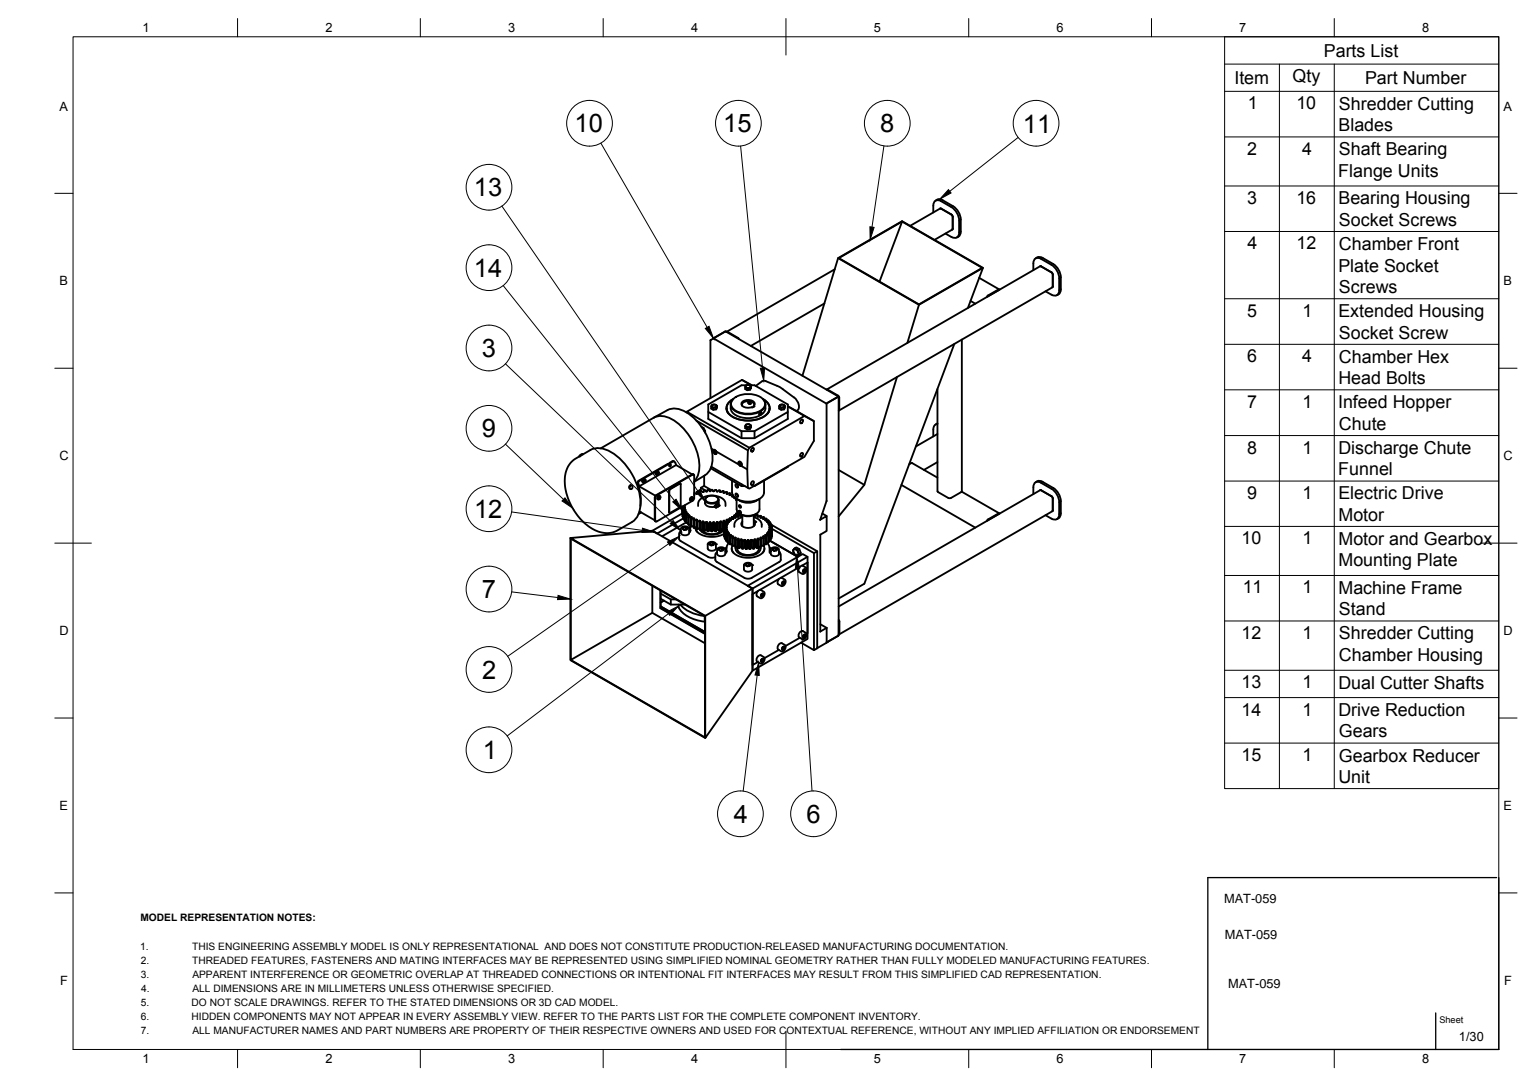
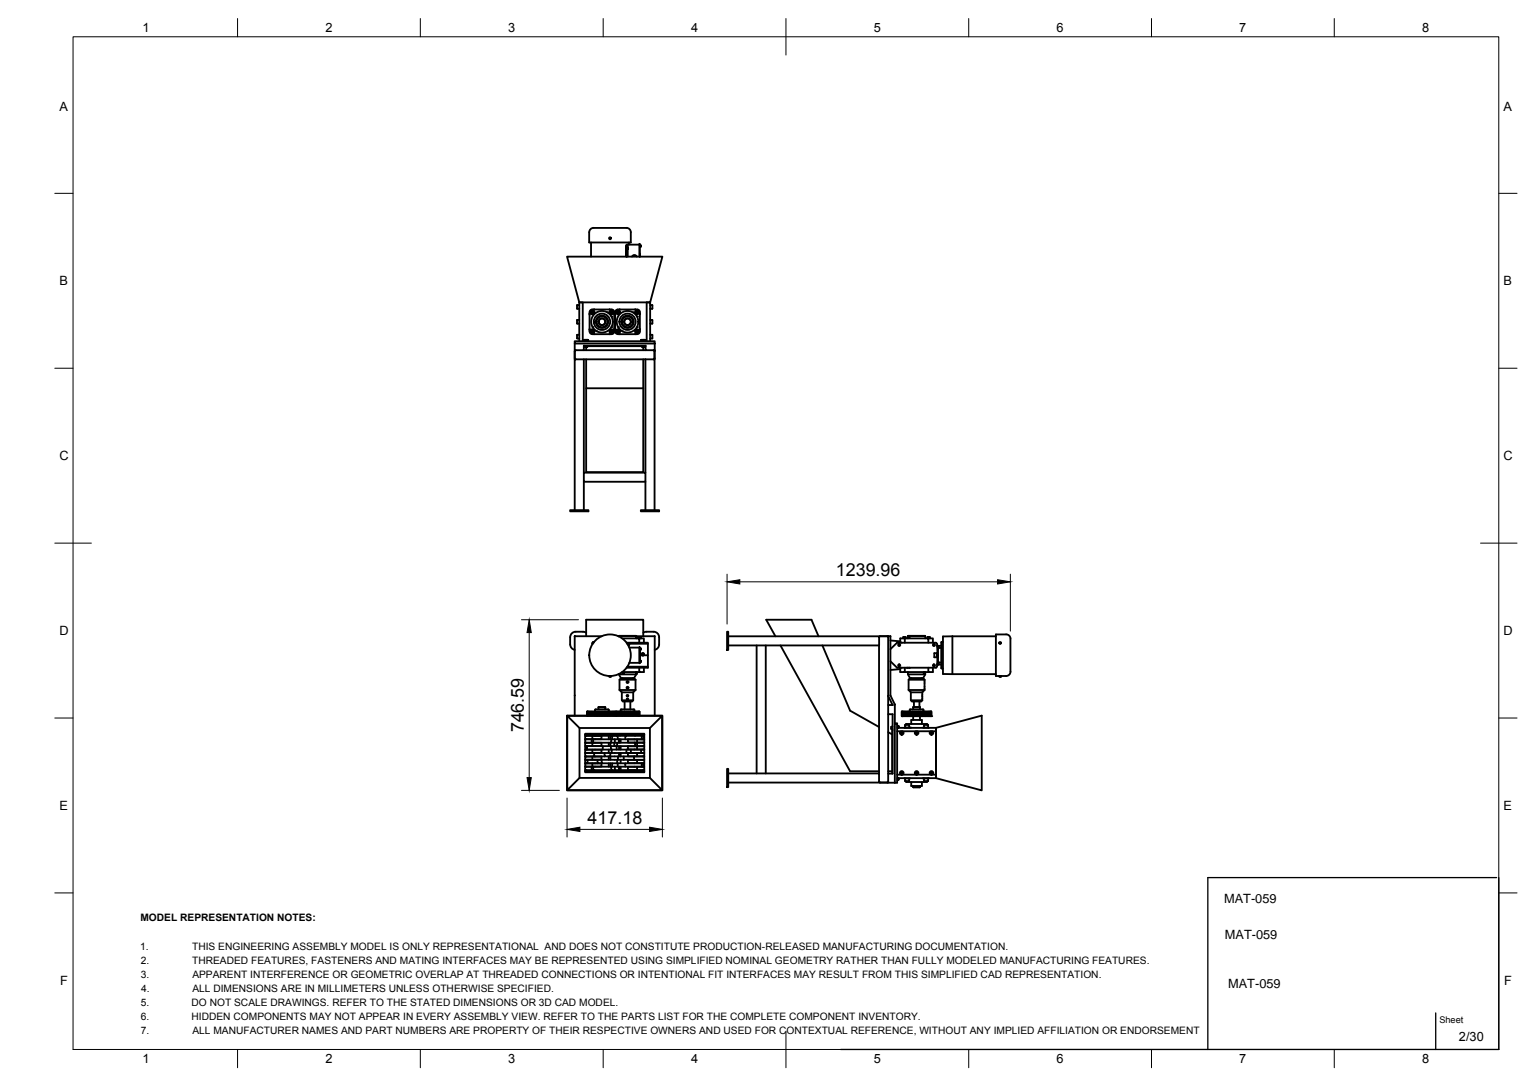
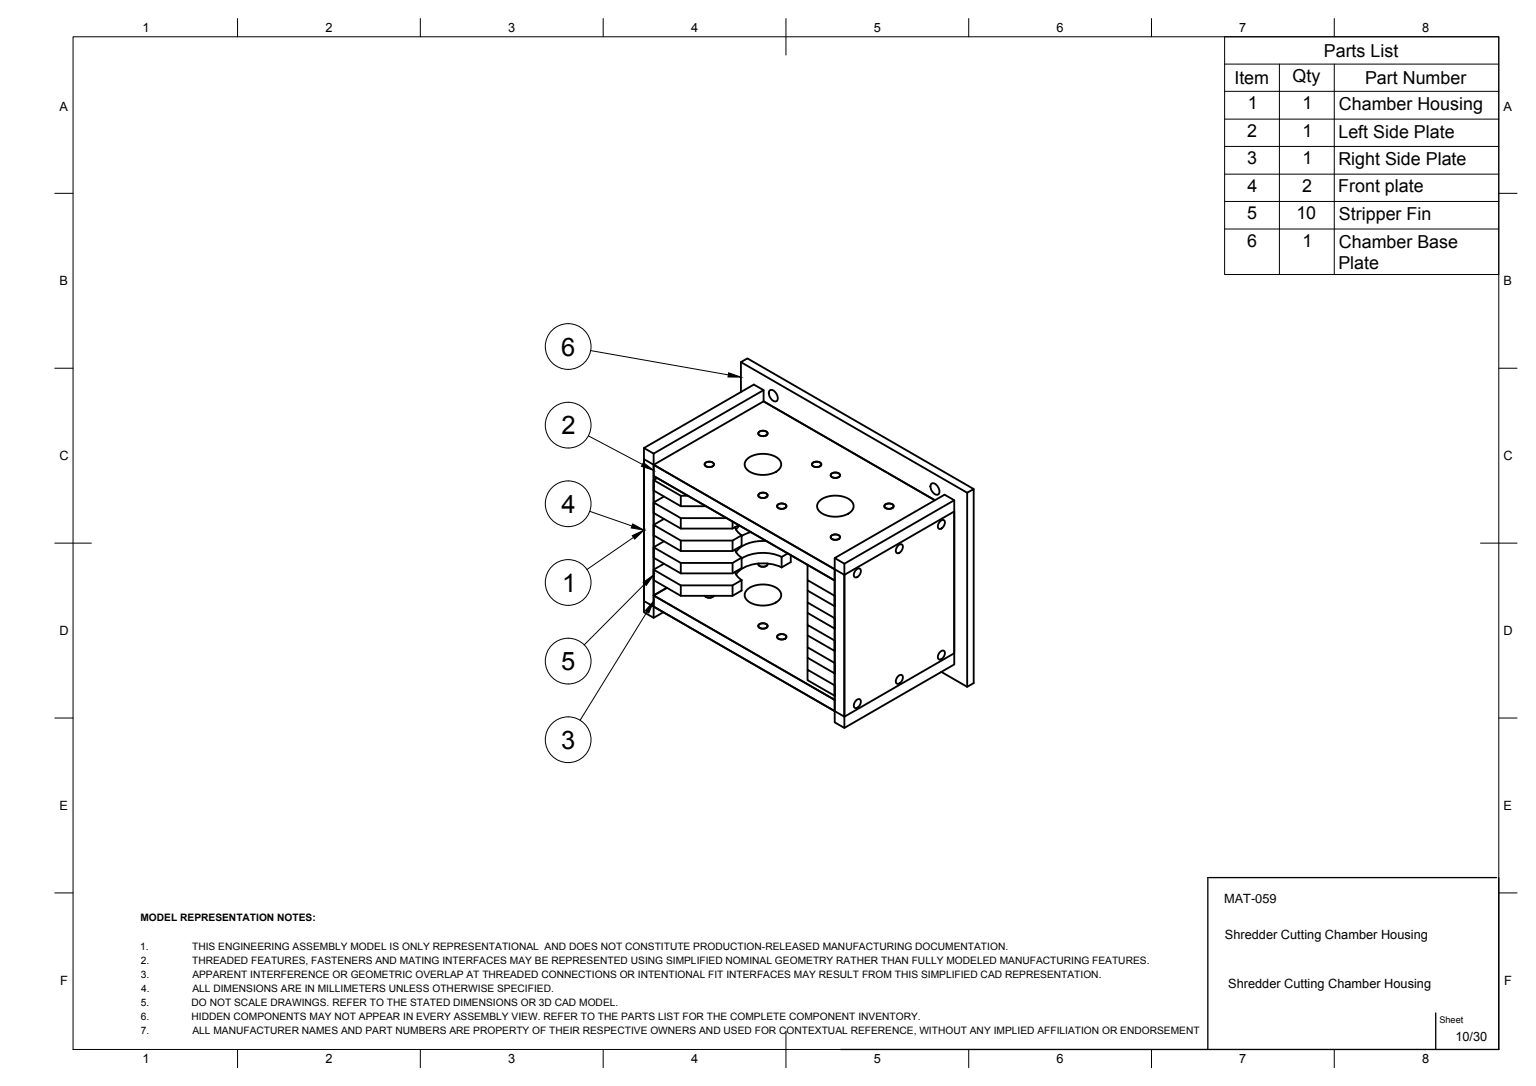
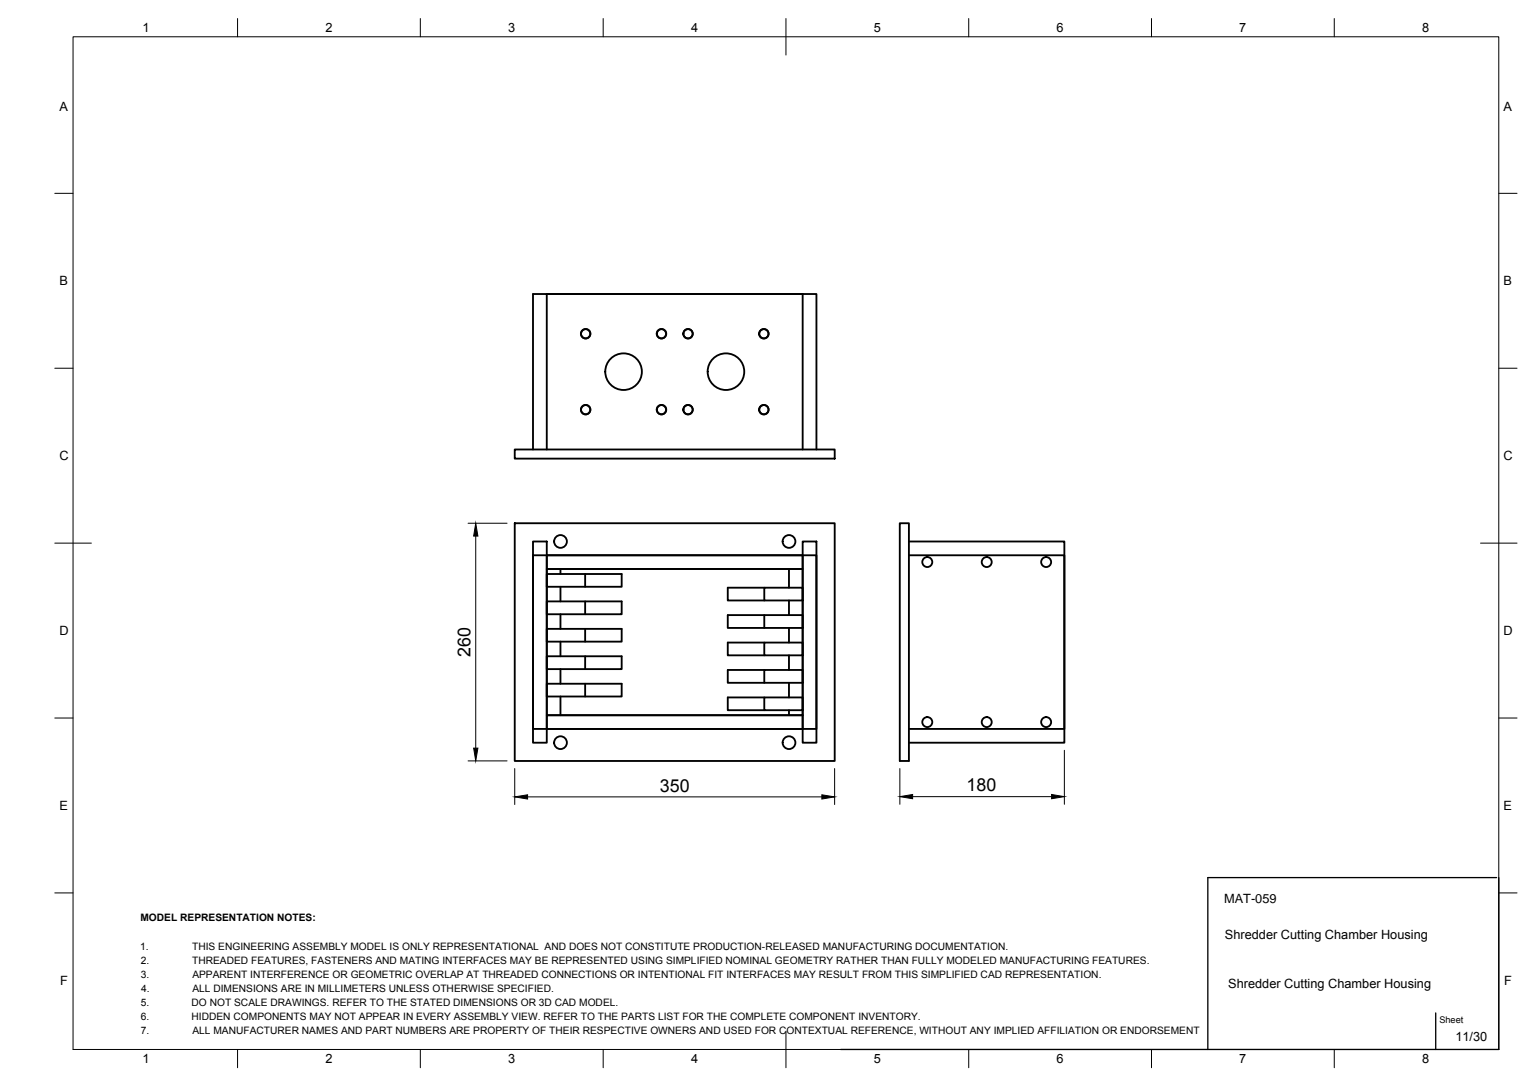
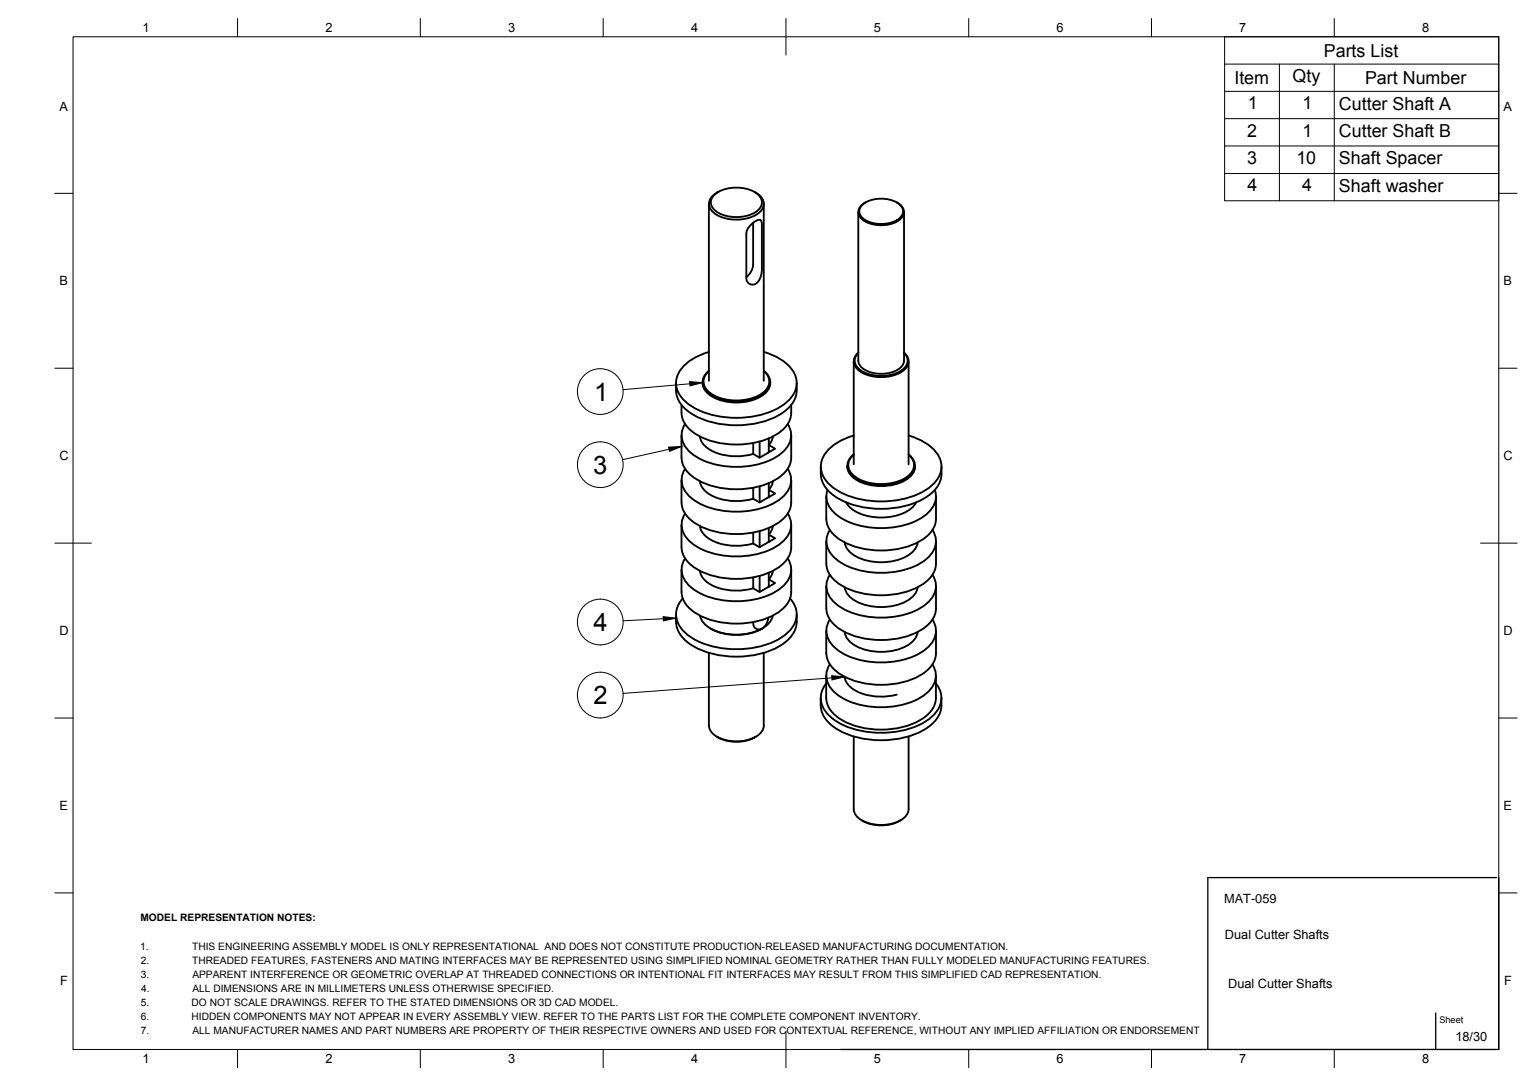
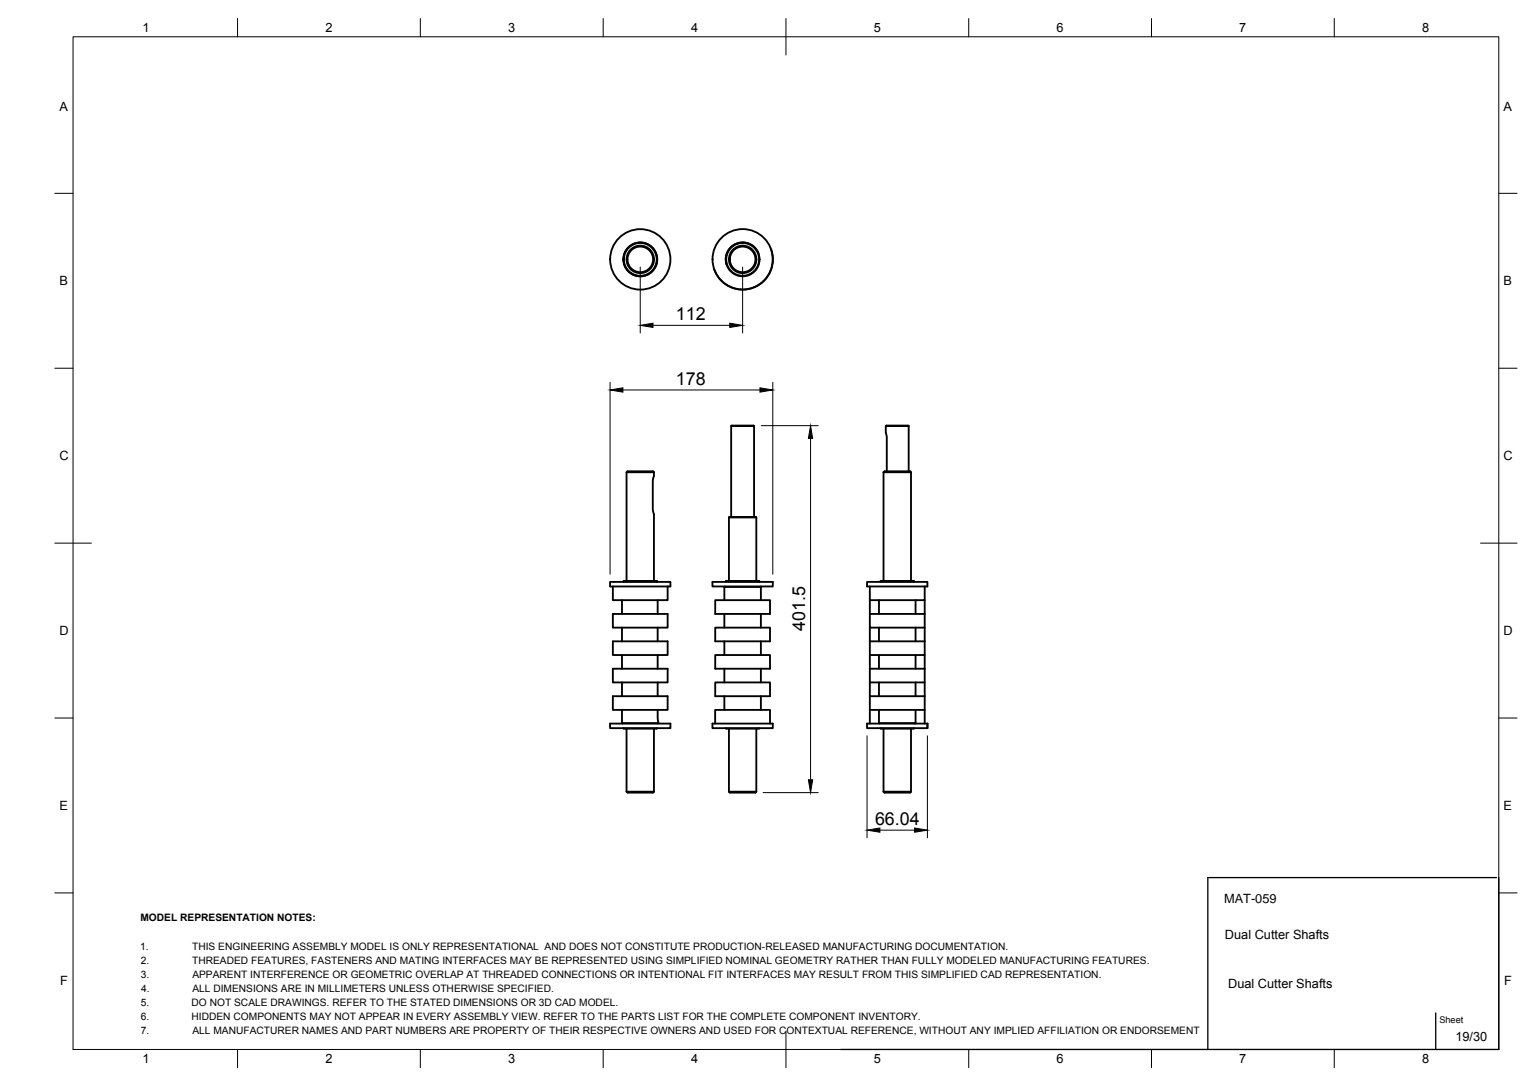
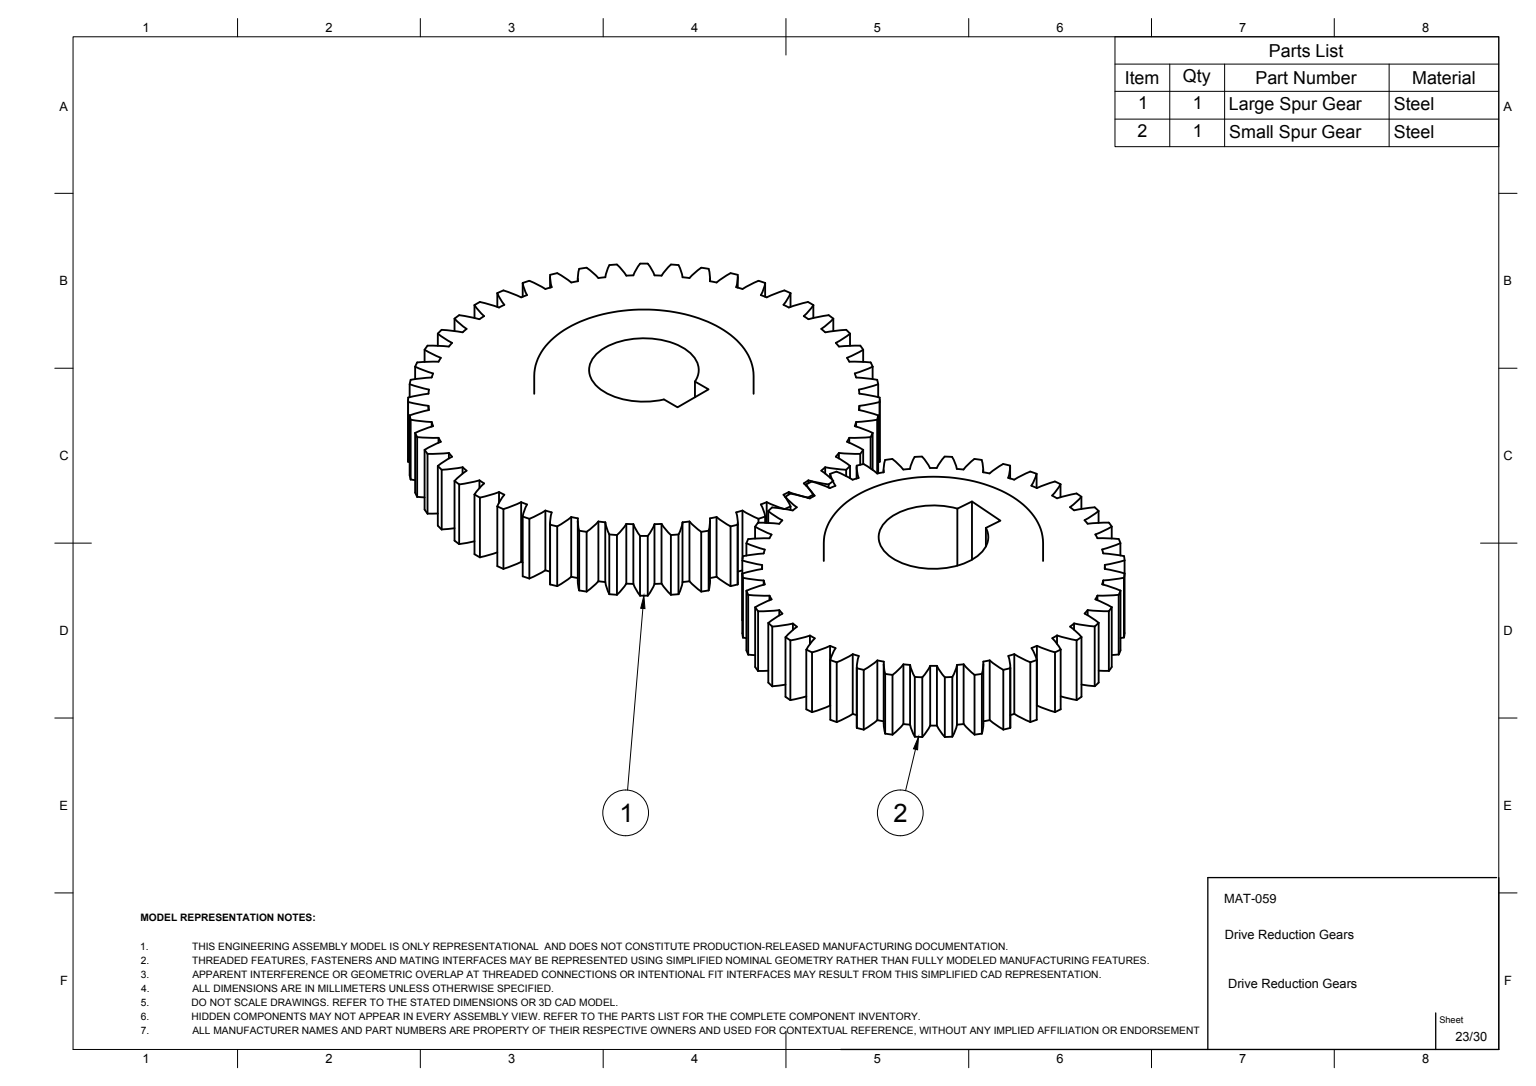
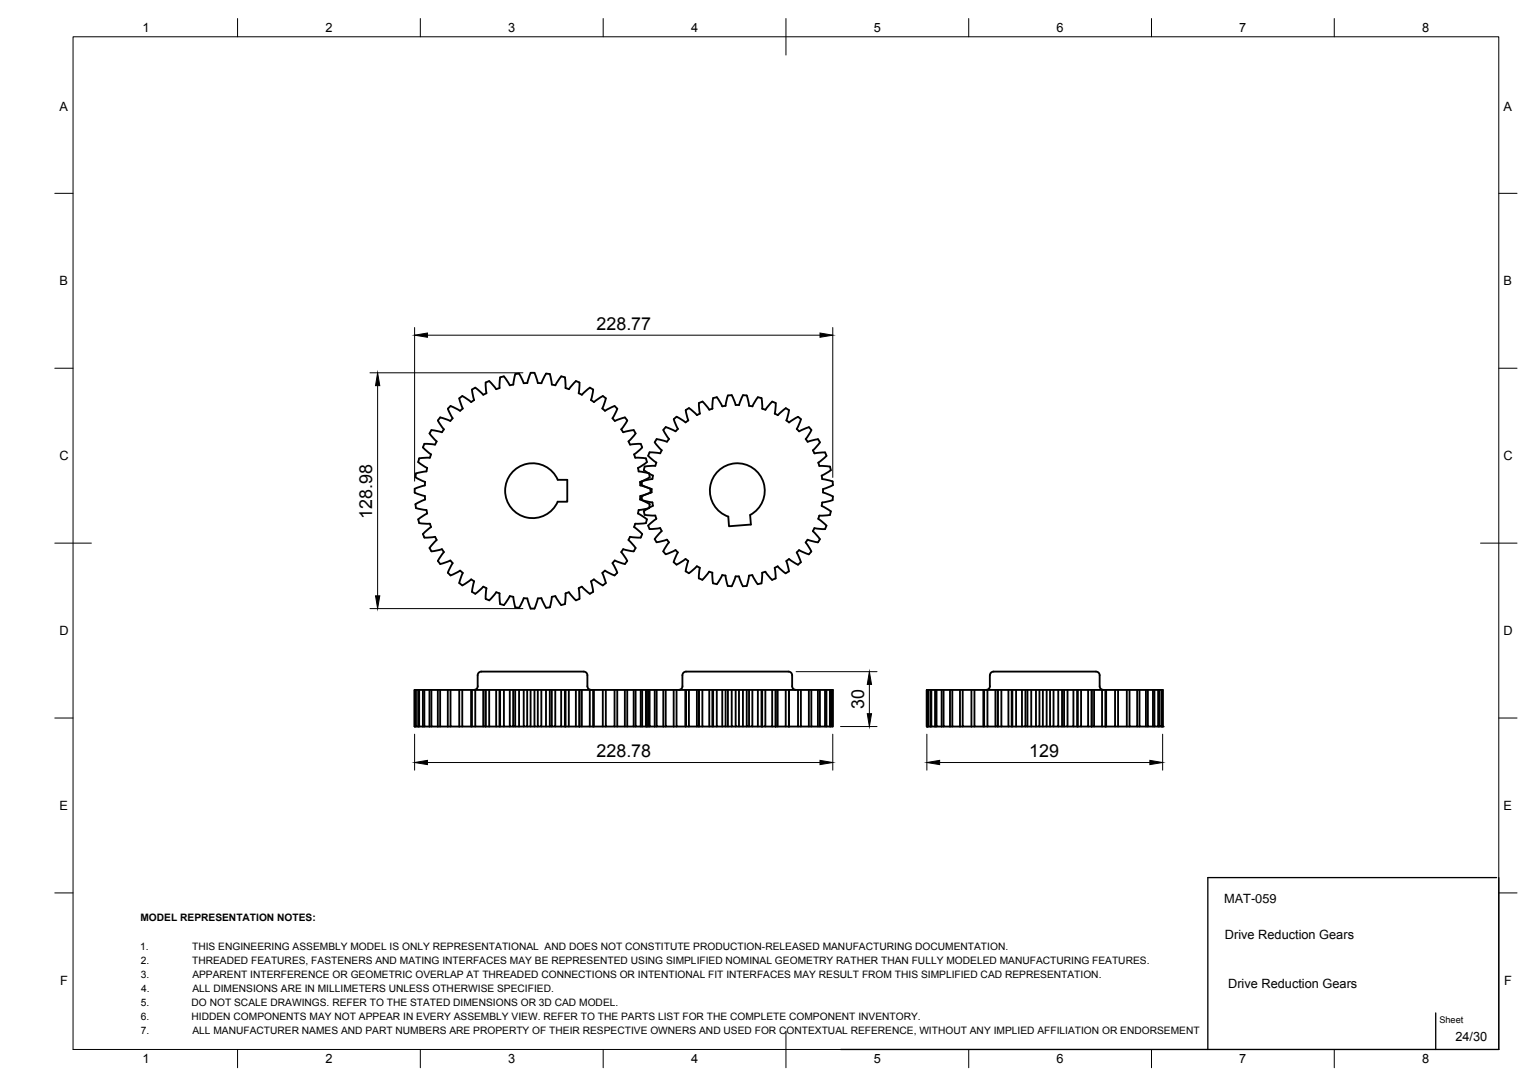
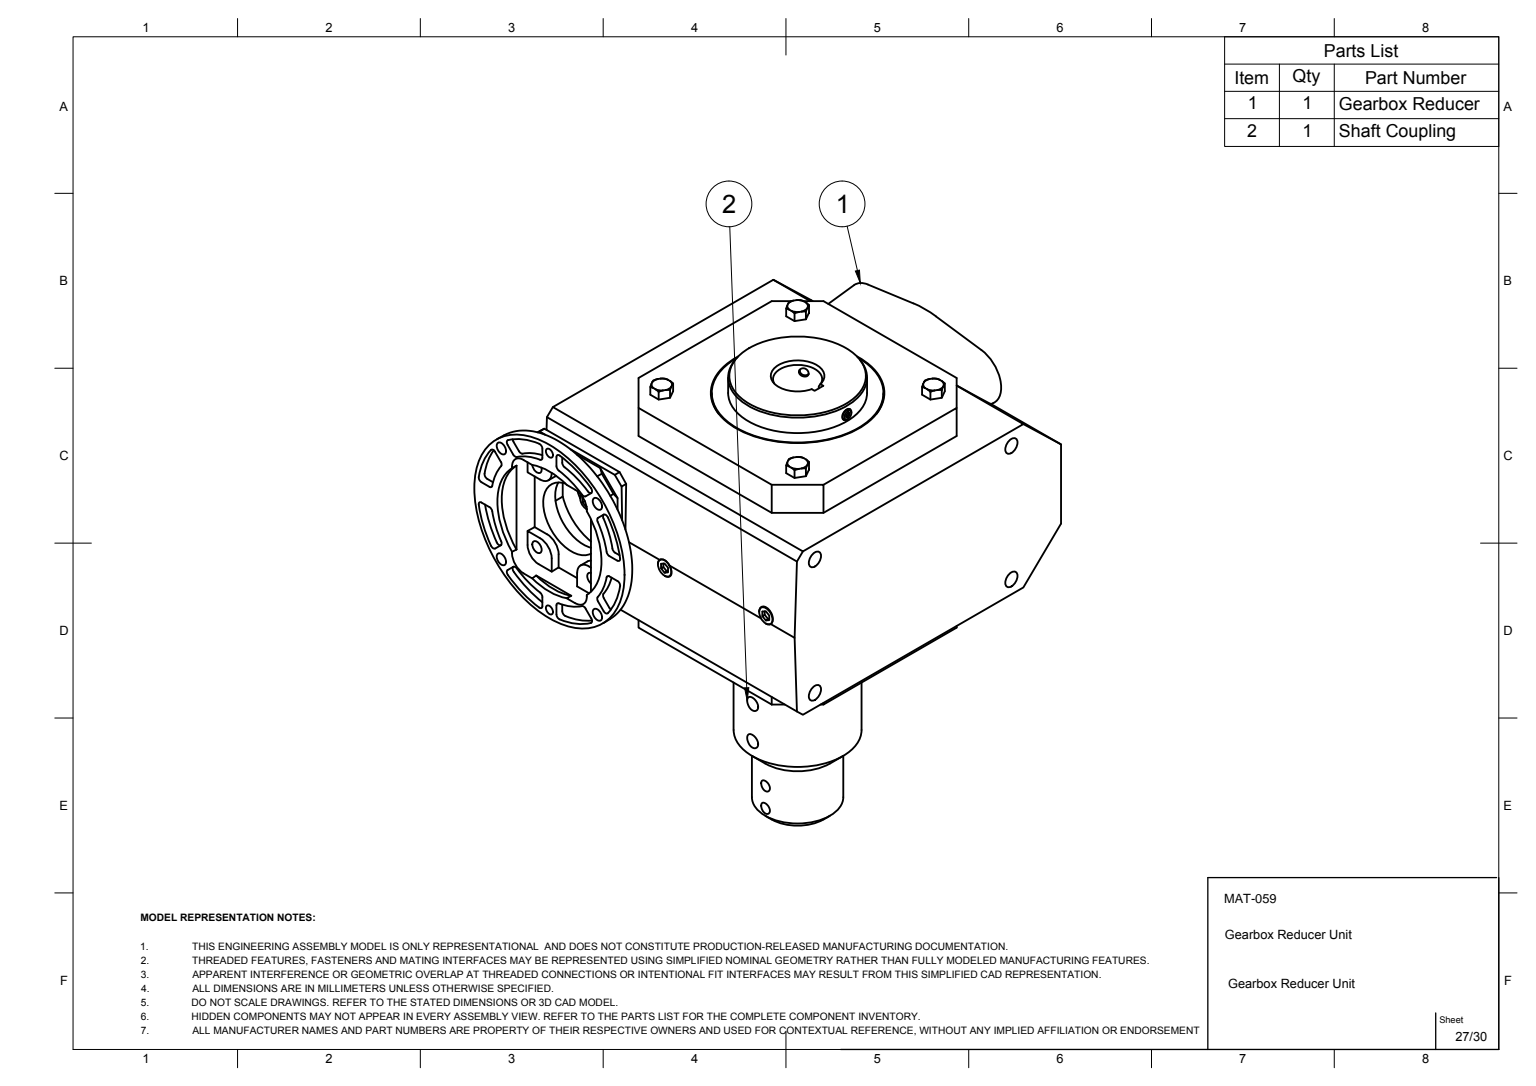
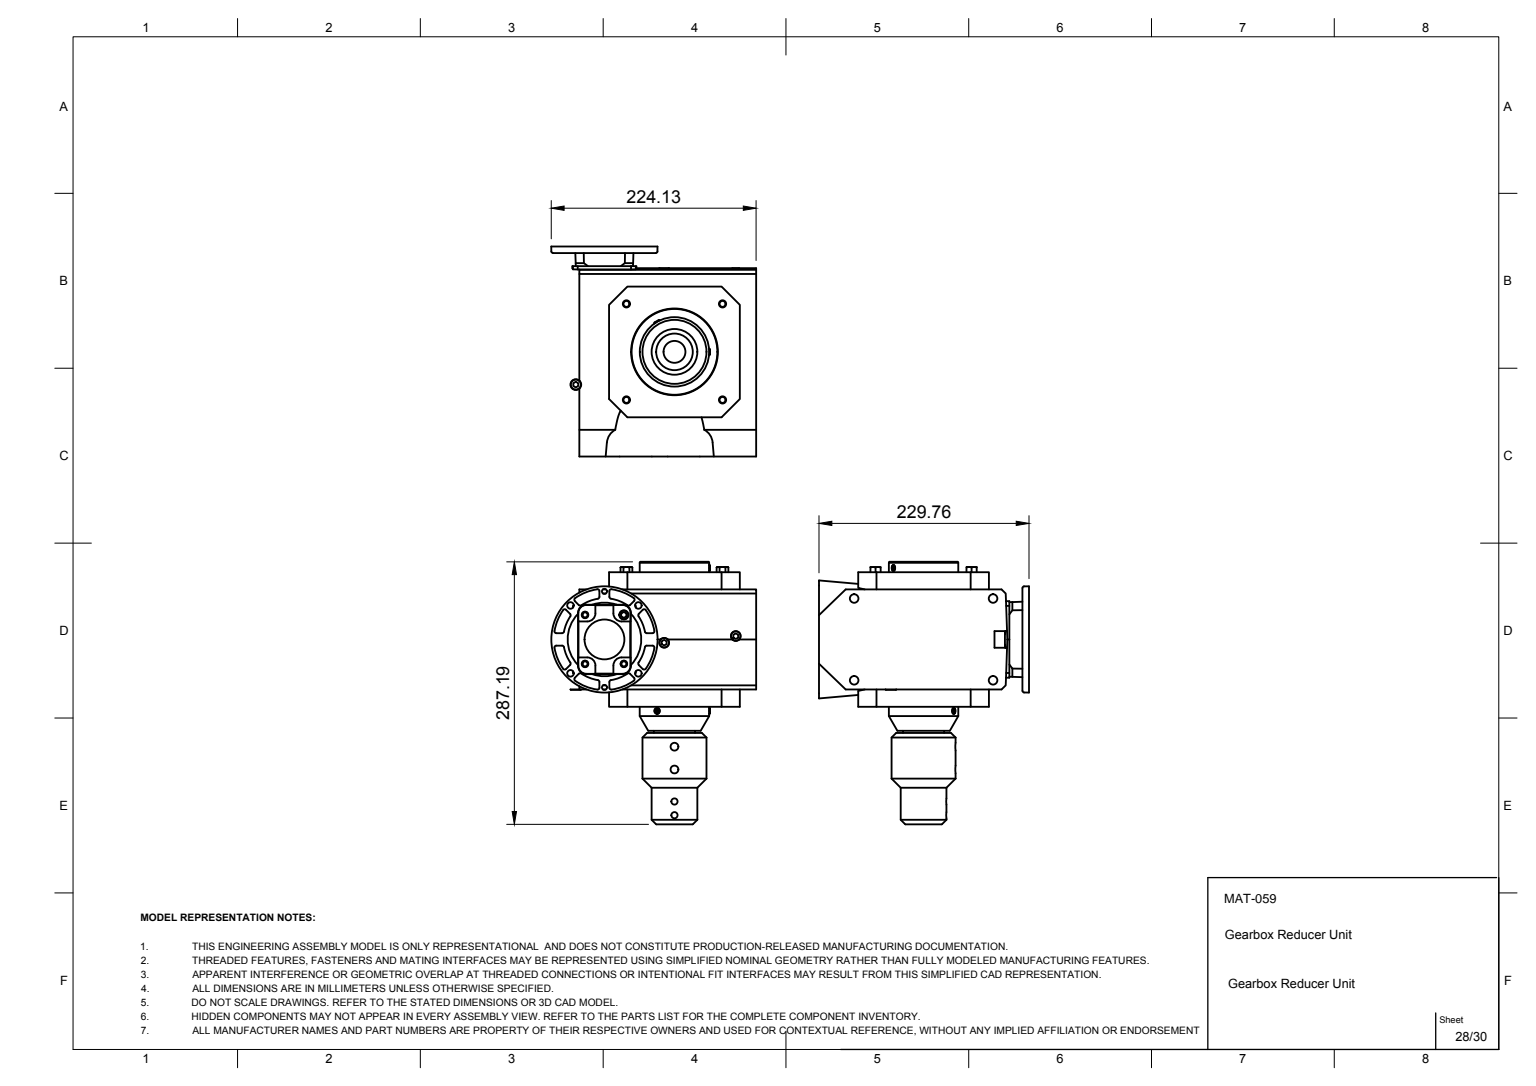
ISO-10303-21;
HEADER;
/* Generated by software containing ST-Developer
 * from STEP Tools, Inc. (www.steptools.com) 
 */

FILE_DESCRIPTION(
/* description */ ('', 'CAx-IF Rec.Pracs.---Representation and Presentation of Product Manufa
cturing Information (PMI)---4.0---2014-10-13'),
/* implementation_level */ '2;1');

FILE_NAME(
/* name */ 'MAT-059',
/* time_stamp */ '2026-10-28T23:00:48+01:00',
/* author */ (''),
/* organization */ (''),
/* preprocessor_version */ 'ST-DEVELOPER v20.2',
/* originating_system */ 'Autodesk Translation Framework v15.17.0.0',
/* authorisation */ '');

FILE_SCHEMA (('AP242_MANAGED_MODEL_BASED_3D_ENGINEERING_MIM_LF { 1 0 10303 442 2 1 4 }'));
ENDSEC;

DATA;
#10=MECHANICAL_DESIGN_GEOMETRIC_PRESENTATION_REPRESENTATION('',(#961,#962,
#963,#964,#965,#966,#967,#968,#969,#970,#971,#972,#973,#974,#975,#976,#977,
#978,#979,#980,#981,#982,#983,#984,#985,#986,#987,#988,#989,#990,#991,#992,
#993,#994,#995,#996,#997,#998,#999),#61811);
#11=ORIENTED_CLOSED_SHELL('',*,#33828,.F.);
#12=ORIENTED_CLOSED_SHELL('',*,#33829,.F.);
#13=ORIENTED_CLOSED_SHELL('',*,#33830,.F.);
#14=ORIENTED_CLOSED_SHELL('',*,#33831,.F.);
#15=ORIENTED_CLOSED_SHELL('',*,#33832,.F.);
#16=ORIENTED_CLOSED_SHELL('',*,#33833,.F.);
#17=ORIENTED_CLOSED_SHELL('',*,#33834,.F.);
#18=ORIENTED_CLOSED_SHELL('',*,#33835,.F.);
#19=ORIENTED_CLOSED_SHELL('',*,#33836,.F.);
#20=ORIENTED_CLOSED_SHELL('',*,#33837,.F.);
#21=BREP_WITH_VOIDS('Body1',#33838,(#11,#12,#13,#14,#15,#16,#17,#18,#19,
#20));
#22=ITEM_DEFINED_TRANSFORMATION($,$,#35703,#35945);
#23=ITEM_DEFINED_TRANSFORMATION($,$,#35762,#35946);
#24=ITEM_DEFINED_TRANSFORMATION($,$,#35823,#35947);
#25=ITEM_DEFINED_TRANSFORMATION($,$,#35884,#35948);
#26=ITEM_DEFINED_TRANSFORMATION($,$,#35884,#35949);
#27=ITEM_DEFINED_TRANSFORMATION($,$,#35909,#35950);
#28=ITEM_DEFINED_TRANSFORMATION($,$,#35909,#35951);
#29=ITEM_DEFINED_TRANSFORMATION($,$,#35909,#35952);
#30=ITEM_DEFINED_TRANSFORMATION($,$,#35909,#35953);
#31=ITEM_DEFINED_TRANSFORMATION($,$,#35909,#35954);
#32=ITEM_DEFINED_TRANSFORMATION($,$,#35909,#35955);
#33=ITEM_DEFINED_TRANSFORMATION($,$,#35909,#35956);
#34=ITEM_DEFINED_TRANSFORMATION($,$,#35909,#35957);
#35=ITEM_DEFINED_TRANSFORMATION($,$,#35909,#35958);
#36=ITEM_DEFINED_TRANSFORMATION($,$,#35909,#35959);
#37=ITEM_DEFINED_TRANSFORMATION($,$,#35922,#35960);
#38=ITEM_DEFINED_TRANSFORMATION($,$,#35962,#36131);
#39=ITEM_DEFINED_TRANSFORMATION($,$,#36032,#36132);
#40=ITEM_DEFINED_TRANSFORMATION($,$,#36110,#36133);
#41=ITEM_DEFINED_TRANSFORMATION($,$,#36110,#36134);
#42=ITEM_DEFINED_TRANSFORMATION($,$,#36110,#36135);
#43=ITEM_DEFINED_TRANSFORMATION($,$,#36110,#36136);
#44=ITEM_DEFINED_TRANSFORMATION($,$,#36110,#36137);
#45=ITEM_DEFINED_TRANSFORMATION($,$,#36110,#36138);
#46=ITEM_DEFINED_TRANSFORMATION($,$,#36110,#36139);
#47=ITEM_DEFINED_TRANSFORMATION($,$,#36110,#36140);
#48=ITEM_DEFINED_TRANSFORMATION($,$,#36110,#36141);
#49=ITEM_DEFINED_TRANSFORMATION($,$,#36110,#36142);
#50=ITEM_DEFINED_TRANSFORMATION($,$,#36122,#36143);
#51=ITEM_DEFINED_TRANSFORMATION($,$,#36122,#36144);
#52=ITEM_DEFINED_TRANSFORMATION($,$,#36122,#36145);
#53=ITEM_DEFINED_TRANSFORMATION($,$,#36122,#36146);
#54=ITEM_DEFINED_TRANSFORMATION($,$,#36148,#37244);
#55=ITEM_DEFINED_TRANSFORMATION($,$,#36744,#37245);
#56=ITEM_DEFINED_TRANSFORMATION($,$,#37247,#38116);
#57=ITEM_DEFINED_TRANSFORMATION($,$,#38087,#38117);
#58=ITEM_DEFINED_TRANSFORMATION($,$,#34117,#38118);
#59=ITEM_DEFINED_TRANSFORMATION($,$,#34117,#38119);
#60=ITEM_DEFINED_TRANSFORMATION($,$,#34117,#38120);
#61=ITEM_DEFINED_TRANSFORMATION($,$,#34117,#38121);
#62=ITEM_DEFINED_TRANSFORMATION($,$,#34117,#38122);
#63=ITEM_DEFINED_TRANSFORMATION($,$,#34117,#38123);
#64=ITEM_DEFINED_TRANSFORMATION($,$,#34117,#38124);
#65=ITEM_DEFINED_TRANSFORMATION($,$,#34117,#38125);
#66=ITEM_DEFINED_TRANSFORMATION($,$,#34117,#38126);
#67=ITEM_DEFINED_TRANSFORMATION($,$,#34117,#38127);
#68=ITEM_DEFINED_TRANSFORMATION($,$,#34153,#38128);
#69=ITEM_DEFINED_TRANSFORMATION($,$,#34153,#38129);
#70=ITEM_DEFINED_TRANSFORMATION($,$,#34153,#38130);
#71=ITEM_DEFINED_TRANSFORMATION($,$,#34153,#38131);
#72=ITEM_DEFINED_TRANSFORMATION($,$,#34392,#38132);
#73=ITEM_DEFINED_TRANSFORMATION($,$,#34392,#38133);
#74=ITEM_DEFINED_TRANSFORMATION($,$,#34392,#38134);
#75=ITEM_DEFINED_TRANSFORMATION($,$,#34392,#38135);
#76=ITEM_DEFINED_TRANSFORMATION($,$,#34392,#38136);
#77=ITEM_DEFINED_TRANSFORMATION($,$,#34392,#38137);
#78=ITEM_DEFINED_TRANSFORMATION($,$,#34392,#38138);
#79=ITEM_DEFINED_TRANSFORMATION($,$,#34392,#38139);
#80=ITEM_DEFINED_TRANSFORMATION($,$,#34392,#38140);
#81=ITEM_DEFINED_TRANSFORMATION($,$,#34392,#38141);
#82=ITEM_DEFINED_TRANSFORMATION($,$,#34392,#38142);
#83=ITEM_DEFINED_TRANSFORMATION($,$,#34392,#38143);
#84=ITEM_DEFINED_TRANSFORMATION($,$,#34392,#38144);
#85=ITEM_DEFINED_TRANSFORMATION($,$,#34392,#38145);
#86=ITEM_DEFINED_TRANSFORMATION($,$,#34392,#38146);
#87=ITEM_DEFINED_TRANSFORMATION($,$,#34392,#38147);
#88=ITEM_DEFINED_TRANSFORMATION($,$,#34420,#38148);
#89=ITEM_DEFINED_TRANSFORMATION($,$,#34420,#38149);
#90=ITEM_DEFINED_TRANSFORMATION($,$,#34420,#38150);
#91=ITEM_DEFINED_TRANSFORMATION($,$,#34420,#38151);
#92=ITEM_DEFINED_TRANSFORMATION($,$,#34420,#38152);
#93=ITEM_DEFINED_TRANSFORMATION($,$,#34420,#38153);
#94=ITEM_DEFINED_TRANSFORMATION($,$,#34420,#38154);
#95=ITEM_DEFINED_TRANSFORMATION($,$,#34420,#38155);
#96=ITEM_DEFINED_TRANSFORMATION($,$,#34420,#38156);
#97=ITEM_DEFINED_TRANSFORMATION($,$,#34420,#38157);
#98=ITEM_DEFINED_TRANSFORMATION($,$,#34420,#38158);
#99=ITEM_DEFINED_TRANSFORMATION($,$,#34420,#38159);
#100=ITEM_DEFINED_TRANSFORMATION($,$,#34448,#38160);
#101=ITEM_DEFINED_TRANSFORMATION($,$,#34476,#38161);
#102=ITEM_DEFINED_TRANSFORMATION($,$,#34476,#38162);
#103=ITEM_DEFINED_TRANSFORMATION($,$,#34476,#38163);
#104=ITEM_DEFINED_TRANSFORMATION($,$,#34476,#38164);
#105=ITEM_DEFINED_TRANSFORMATION($,$,#34512,#38165);
#106=ITEM_DEFINED_TRANSFORMATION($,$,#34528,#38166);
#107=ITEM_DEFINED_TRANSFORMATION($,$,#34568,#38167);
#108=ITEM_DEFINED_TRANSFORMATION($,$,#35040,#38168);
#109=ITEM_DEFINED_TRANSFORMATION($,$,#35191,#38169);
#110=ITEM_DEFINED_TRANSFORMATION($,$,#35702,#38170);
#111=ITEM_DEFINED_TRANSFORMATION($,$,#35961,#38171);
#112=ITEM_DEFINED_TRANSFORMATION($,$,#36147,#38172);
#113=ITEM_DEFINED_TRANSFORMATION($,$,#37246,#38173);
#114=(
REPRESENTATION_RELATIONSHIP($,$,#61981,#61980)
REPRESENTATION_RELATIONSHIP_WITH_TRANSFORMATION(#22)
SHAPE_REPRESENTATION_RELATIONSHIP()
);
#115=(
REPRESENTATION_RELATIONSHIP($,$,#61982,#61980)
REPRESENTATION_RELATIONSHIP_WITH_TRANSFORMATION(#23)
SHAPE_REPRESENTATION_RELATIONSHIP()
);
#116=(
REPRESENTATION_RELATIONSHIP($,$,#61983,#61980)
REPRESENTATION_RELATIONSHIP_WITH_TRANSFORMATION(#24)
SHAPE_REPRESENTATION_RELATIONSHIP()
);
#117=(
REPRESENTATION_RELATIONSHIP($,$,#61984,#61980)
REPRESENTATION_RELATIONSHIP_WITH_TRANSFORMATION(#25)
SHAPE_REPRESENTATION_RELATIONSHIP()
);
#118=(
REPRESENTATION_RELATIONSHIP($,$,#61984,#61980)
REPRESENTATION_RELATIONSHIP_WITH_TRANSFORMATION(#26)
SHAPE_REPRESENTATION_RELATIONSHIP()
);
#119=(
REPRESENTATION_RELATIONSHIP($,$,#61985,#61980)
REPRESENTATION_RELATIONSHIP_WITH_TRANSFORMATION(#27)
SHAPE_REPRESENTATION_RELATIONSHIP()
);
#120=(
REPRESENTATION_RELATIONSHIP($,$,#61985,#61980)
REPRESENTATION_RELATIONSHIP_WITH_TRANSFORMATION(#28)
SHAPE_REPRESENTATION_RELATIONSHIP()
);
#121=(
REPRESENTATION_RELATIONSHIP($,$,#61985,#61980)
REPRESENTATION_RELATIONSHIP_WITH_TRANSFORMATION(#29)
SHAPE_REPRESENTATION_RELATIONSHIP()
);
#122=(
REPRESENTATION_RELATIONSHIP($,$,#61985,#61980)
REPRESENTATION_RELATIONSHIP_WITH_TRANSFORMATION(#30)
SHAPE_REPRESENTATION_RELATIONSHIP()
);
#123=(
REPRESENTATION_RELATIONSHIP($,$,#61985,#61980)
REPRESENTATION_RELATIONSHIP_WITH_TRANSFORMATION(#31)
SHAPE_REPRESENTATION_RELATIONSHIP()
);
#124=(
REPRESENTATION_RELATIONSHIP($,$,#61985,#61980)
REPRESENTATION_RELATIONSHIP_WITH_TRANSFORMATION(#32)
SHAPE_REPRESENTATION_RELATIONSHIP()
);
#125=(
REPRESENTATION_RELATIONSHIP($,$,#61985,#61980)
REPRESENTATION_RELATIONSHIP_WITH_TRANSFORMATION(#33)
SHAPE_REPRESENTATION_RELATIONSHIP()
);
#126=(
REPRESENTATION_RELATIONSHIP($,$,#61985,#61980)
REPRESENTATION_RELATIONSHIP_WITH_TRANSFORMATION(#34)
SHAPE_REPRESENTATION_RELATIONSHIP()
);
#127=(
REPRESENTATION_RELATIONSHIP($,$,#61985,#61980)
REPRESENTATION_RELATIONSHIP_WITH_TRANSFORMATION(#35)
SHAPE_REPRESENTATION_RELATIONSHIP()
);
#128=(
REPRESENTATION_RELATIONSHIP($,$,#61985,#61980)
REPRESENTATION_RELATIONSHIP_WITH_TRANSFORMATION(#36)
SHAPE_REPRESENTATION_RELATIONSHIP()
);
#129=(
REPRESENTATION_RELATIONSHIP($,$,#61986,#61980)
REPRESENTATION_RELATIONSHIP_WITH_TRANSFORMATION(#37)
SHAPE_REPRESENTATION_RELATIONSHIP()
);
#130=(
REPRESENTATION_RELATIONSHIP($,$,#61988,#61987)
REPRESENTATION_RELATIONSHIP_WITH_TRANSFORMATION(#38)
SHAPE_REPRESENTATION_RELATIONSHIP()
);
#131=(
REPRESENTATION_RELATIONSHIP($,$,#61989,#61987)
REPRESENTATION_RELATIONSHIP_WITH_TRANSFORMATION(#39)
SHAPE_REPRESENTATION_RELATIONSHIP()
);
#132=(
REPRESENTATION_RELATIONSHIP($,$,#61990,#61987)
REPRESENTATION_RELATIONSHIP_WITH_TRANSFORMATION(#40)
SHAPE_REPRESENTATION_RELATIONSHIP()
);
#133=(
REPRESENTATION_RELATIONSHIP($,$,#61990,#61987)
REPRESENTATION_RELATIONSHIP_WITH_TRANSFORMATION(#41)
SHAPE_REPRESENTATION_RELATIONSHIP()
);
#134=(
REPRESENTATION_RELATIONSHIP($,$,#61990,#61987)
REPRESENTATION_RELATIONSHIP_WITH_TRANSFORMATION(#42)
SHAPE_REPRESENTATION_RELATIONSHIP()
);
#135=(
REPRESENTATION_RELATIONSHIP($,$,#61990,#61987)
REPRESENTATION_RELATIONSHIP_WITH_TRANSFORMATION(#43)
SHAPE_REPRESENTATION_RELATIONSHIP()
);
#136=(
REPRESENTATION_RELATIONSHIP($,$,#61990,#61987)
REPRESENTATION_RELATIONSHIP_WITH_TRANSFORMATION(#44)
SHAPE_REPRESENTATION_RELATIONSHIP()
);
#137=(
REPRESENTATION_RELATIONSHIP($,$,#61990,#61987)
REPRESENTATION_RELATIONSHIP_WITH_TRANSFORMATION(#45)
SHAPE_REPRESENTATION_RELATIONSHIP()
);
#138=(
REPRESENTATION_RELATIONSHIP($,$,#61990,#61987)
REPRESENTATION_RELATIONSHIP_WITH_TRANSFORMATION(#46)
SHAPE_REPRESENTATION_RELATIONSHIP()
);
#139=(
REPRESENTATION_RELATIONSHIP($,$,#61990,#61987)
REPRESENTATION_RELATIONSHIP_WITH_TRANSFORMATION(#47)
SHAPE_REPRESENTATION_RELATIONSHIP()
);
#140=(
REPRESENTATION_RELATIONSHIP($,$,#61990,#61987)
REPRESENTATION_RELATIONSHIP_WITH_TRANSFORMATION(#48)
SHAPE_REPRESENTATION_RELATIONSHIP()
);
#141=(
REPRESENTATION_RELATIONSHIP($,$,#61990,#61987)
REPRESENTATION_RELATIONSHIP_WITH_TRANSFORMATION(#49)
SHAPE_REPRESENTATION_RELATIONSHIP()
);
#142=(
REPRESENTATION_RELATIONSHIP($,$,#61991,#61987)
REPRESENTATION_RELATIONSHIP_WITH_TRANSFORMATION(#50)
SHAPE_REPRESENTATION_RELATIONSHIP()
);
#143=(
REPRESENTATION_RELATIONSHIP($,$,#61991,#61987)
REPRESENTATION_RELATIONSHIP_WITH_TRANSFORMATION(#51)
SHAPE_REPRESENTATION_RELATIONSHIP()
);
#144=(
REPRESENTATION_RELATIONSHIP($,$,#61991,#61987)
REPRESENTATION_RELATIONSHIP_WITH_TRANSFORMATION(#52)
SHAPE_REPRESENTATION_RELATIONSHIP()
);
#145=(
REPRESENTATION_RELATIONSHIP($,$,#61991,#61987)
REPRESENTATION_RELATIONSHIP_WITH_TRANSFORMATION(#53)
SHAPE_REPRESENTATION_RELATIONSHIP()
);
#146=(
REPRESENTATION_RELATIONSHIP($,$,#61993,#61992)
REPRESENTATION_RELATIONSHIP_WITH_TRANSFORMATION(#54)
SHAPE_REPRESENTATION_RELATIONSHIP()
);
#147=(
REPRESENTATION_RELATIONSHIP($,$,#61994,#61992)
REPRESENTATION_RELATIONSHIP_WITH_TRANSFORMATION(#55)
SHAPE_REPRESENTATION_RELATIONSHIP()
);
#148=(
REPRESENTATION_RELATIONSHIP($,$,#61996,#61995)
REPRESENTATION_RELATIONSHIP_WITH_TRANSFORMATION(#56)
SHAPE_REPRESENTATION_RELATIONSHIP()
);
#149=(
REPRESENTATION_RELATIONSHIP($,$,#61997,#61995)
REPRESENTATION_RELATIONSHIP_WITH_TRANSFORMATION(#57)
SHAPE_REPRESENTATION_RELATIONSHIP()
);
#150=(
REPRESENTATION_RELATIONSHIP($,$,#61969,#61968)
REPRESENTATION_RELATIONSHIP_WITH_TRANSFORMATION(#58)
SHAPE_REPRESENTATION_RELATIONSHIP()
);
#151=(
REPRESENTATION_RELATIONSHIP($,$,#61969,#61968)
REPRESENTATION_RELATIONSHIP_WITH_TRANSFORMATION(#59)
SHAPE_REPRESENTATION_RELATIONSHIP()
);
#152=(
REPRESENTATION_RELATIONSHIP($,$,#61969,#61968)
REPRESENTATION_RELATIONSHIP_WITH_TRANSFORMATION(#60)
SHAPE_REPRESENTATION_RELATIONSHIP()
);
#153=(
REPRESENTATION_RELATIONSHIP($,$,#61969,#61968)
REPRESENTATION_RELATIONSHIP_WITH_TRANSFORMATION(#61)
SHAPE_REPRESENTATION_RELATIONSHIP()
);
#154=(
REPRESENTATION_RELATIONSHIP($,$,#61969,#61968)
REPRESENTATION_RELATIONSHIP_WITH_TRANSFORMATION(#62)
SHAPE_REPRESENTATION_RELATIONSHIP()
);
#155=(
REPRESENTATION_RELATIONSHIP($,$,#61969,#61968)
REPRESENTATION_RELATIONSHIP_WITH_TRANSFORMATION(#63)
SHAPE_REPRESENTATION_RELATIONSHIP()
);
#156=(
REPRESENTATION_RELATIONSHIP($,$,#61969,#61968)
REPRESENTATION_RELATIONSHIP_WITH_TRANSFORMATION(#64)
SHAPE_REPRESENTATION_RELATIONSHIP()
);
#157=(
REPRESENTATION_RELATIONSHIP($,$,#61969,#61968)
REPRESENTATION_RELATIONSHIP_WITH_TRANSFORMATION(#65)
SHAPE_REPRESENTATION_RELATIONSHIP()
);
#158=(
REPRESENTATION_RELATIONSHIP($,$,#61969,#61968)
REPRESENTATION_RELATIONSHIP_WITH_TRANSFORMATION(#66)
SHAPE_REPRESENTATION_RELATIONSHIP()
);
#159=(
REPRESENTATION_RELATIONSHIP($,$,#61969,#61968)
REPRESENTATION_RELATIONSHIP_WITH_TRANSFORMATION(#67)
SHAPE_REPRESENTATION_RELATIONSHIP()
);
#160=(
REPRESENTATION_RELATIONSHIP($,$,#61970,#61968)
REPRESENTATION_RELATIONSHIP_WITH_TRANSFORMATION(#68)
SHAPE_REPRESENTATION_RELATIONSHIP()
);
#161=(
REPRESENTATION_RELATIONSHIP($,$,#61970,#61968)
REPRESENTATION_RELATIONSHIP_WITH_TRANSFORMATION(#69)
SHAPE_REPRESENTATION_RELATIONSHIP()
);
#162=(
REPRESENTATION_RELATIONSHIP($,$,#61970,#61968)
REPRESENTATION_RELATIONSHIP_WITH_TRANSFORMATION(#70)
SHAPE_REPRESENTATION_RELATIONSHIP()
);
#163=(
REPRESENTATION_RELATIONSHIP($,$,#61970,#61968)
REPRESENTATION_RELATIONSHIP_WITH_TRANSFORMATION(#71)
SHAPE_REPRESENTATION_RELATIONSHIP()
);
#164=(
REPRESENTATION_RELATIONSHIP($,$,#61971,#61968)
REPRESENTATION_RELATIONSHIP_WITH_TRANSFORMATION(#72)
SHAPE_REPRESENTATION_RELATIONSHIP()
);
#165=(
REPRESENTATION_RELATIONSHIP($,$,#61971,#61968)
REPRESENTATION_RELATIONSHIP_WITH_TRANSFORMATION(#73)
SHAPE_REPRESENTATION_RELATIONSHIP()
);
#166=(
REPRESENTATION_RELATIONSHIP($,$,#61971,#61968)
REPRESENTATION_RELATIONSHIP_WITH_TRANSFORMATION(#74)
SHAPE_REPRESENTATION_RELATIONSHIP()
);
#167=(
REPRESENTATION_RELATIONSHIP($,$,#61971,#61968)
REPRESENTATION_RELATIONSHIP_WITH_TRANSFORMATION(#75)
SHAPE_REPRESENTATION_RELATIONSHIP()
);
#168=(
REPRESENTATION_RELATIONSHIP($,$,#61971,#61968)
REPRESENTATION_RELATIONSHIP_WITH_TRANSFORMATION(#76)
SHAPE_REPRESENTATION_RELATIONSHIP()
);
#169=(
REPRESENTATION_RELATIONSHIP($,$,#61971,#61968)
REPRESENTATION_RELATIONSHIP_WITH_TRANSFORMATION(#77)
SHAPE_REPRESENTATION_RELATIONSHIP()
);
#170=(
REPRESENTATION_RELATIONSHIP($,$,#61971,#61968)
REPRESENTATION_RELATIONSHIP_WITH_TRANSFORMATION(#78)
SHAPE_REPRESENTATION_RELATIONSHIP()
);
#171=(
REPRESENTATION_RELATIONSHIP($,$,#61971,#61968)
REPRESENTATION_RELATIONSHIP_WITH_TRANSFORMATION(#79)
SHAPE_REPRESENTATION_RELATIONSHIP()
);
#172=(
REPRESENTATION_RELATIONSHIP($,$,#61971,#61968)
REPRESENTATION_RELATIONSHIP_WITH_TRANSFORMATION(#80)
SHAPE_REPRESENTATION_RELATIONSHIP()
);
#173=(
REPRESENTATION_RELATIONSHIP($,$,#61971,#61968)
REPRESENTATION_RELATIONSHIP_WITH_TRANSFORMATION(#81)
SHAPE_REPRESENTATION_RELATIONSHIP()
);
#174=(
REPRESENTATION_RELATIONSHIP($,$,#61971,#61968)
REPRESENTATION_RELATIONSHIP_WITH_TRANSFORMATION(#82)
SHAPE_REPRESENTATION_RELATIONSHIP()
);
#175=(
REPRESENTATION_RELATIONSHIP($,$,#61971,#61968)
REPRESENTATION_RELATIONSHIP_WITH_TRANSFORMATION(#83)
SHAPE_REPRESENTATION_RELATIONSHIP()
);
#176=(
REPRESENTATION_RELATIONSHIP($,$,#61971,#61968)
REPRESENTATION_RELATIONSHIP_WITH_TRANSFORMATION(#84)
SHAPE_REPRESENTATION_RELATIONSHIP()
);
#177=(
REPRESENTATION_RELATIONSHIP($,$,#61971,#61968)
REPRESENTATION_RELATIONSHIP_WITH_TRANSFORMATION(#85)
SHAPE_REPRESENTATION_RELATIONSHIP()
);
#178=(
REPRESENTATION_RELATIONSHIP($,$,#61971,#61968)
REPRESENTATION_RELATIONSHIP_WITH_TRANSFORMATION(#86)
SHAPE_REPRESENTATION_RELATIONSHIP()
);
#179=(
REPRESENTATION_RELATIONSHIP($,$,#61971,#61968)
REPRESENTATION_RELATIONSHIP_WITH_TRANSFORMATION(#87)
SHAPE_REPRESENTATION_RELATIONSHIP()
);
#180=(
REPRESENTATION_RELATIONSHIP($,$,#61972,#61968)
REPRESENTATION_RELATIONSHIP_WITH_TRANSFORMATION(#88)
SHAPE_REPRESENTATION_RELATIONSHIP()
);
#181=(
REPRESENTATION_RELATIONSHIP($,$,#61972,#61968)
REPRESENTATION_RELATIONSHIP_WITH_TRANSFORMATION(#89)
SHAPE_REPRESENTATION_RELATIONSHIP()
);
#182=(
REPRESENTATION_RELATIONSHIP($,$,#61972,#61968)
REPRESENTATION_RELATIONSHIP_WITH_TRANSFORMATION(#90)
SHAPE_REPRESENTATION_RELATIONSHIP()
);
#183=(
REPRESENTATION_RELATIONSHIP($,$,#61972,#61968)
REPRESENTATION_RELATIONSHIP_WITH_TRANSFORMATION(#91)
SHAPE_REPRESENTATION_RELATIONSHIP()
);
#184=(
REPRESENTATION_RELATIONSHIP($,$,#61972,#61968)
REPRESENTATION_RELATIONSHIP_WITH_TRANSFORMATION(#92)
SHAPE_REPRESENTATION_RELATIONSHIP()
);
#185=(
REPRESENTATION_RELATIONSHIP($,$,#61972,#61968)
REPRESENTATION_RELATIONSHIP_WITH_TRANSFORMATION(#93)
SHAPE_REPRESENTATION_RELATIONSHIP()
);
#186=(
REPRESENTATION_RELATIONSHIP($,$,#61972,#61968)
REPRESENTATION_RELATIONSHIP_WITH_TRANSFORMATION(#94)
SHAPE_REPRESENTATION_RELATIONSHIP()
);
#187=(
REPRESENTATION_RELATIONSHIP($,$,#61972,#61968)
REPRESENTATION_RELATIONSHIP_WITH_TRANSFORMATION(#95)
SHAPE_REPRESENTATION_RELATIONSHIP()
);
#188=(
REPRESENTATION_RELATIONSHIP($,$,#61972,#61968)
REPRESENTATION_RELATIONSHIP_WITH_TRANSFORMATION(#96)
SHAPE_REPRESENTATION_RELATIONSHIP()
);
#189=(
REPRESENTATION_RELATIONSHIP($,$,#61972,#61968)
REPRESENTATION_RELATIONSHIP_WITH_TRANSFORMATION(#97)
SHAPE_REPRESENTATION_RELATIONSHIP()
);
#190=(
REPRESENTATION_RELATIONSHIP($,$,#61972,#61968)
REPRESENTATION_RELATIONSHIP_WITH_TRANSFORMATION(#98)
SHAPE_REPRESENTATION_RELATIONSHIP()
);
#191=(
REPRESENTATION_RELATIONSHIP($,$,#61972,#61968)
REPRESENTATION_RELATIONSHIP_WITH_TRANSFORMATION(#99)
SHAPE_REPRESENTATION_RELATIONSHIP()
);
#192=(
REPRESENTATION_RELATIONSHIP($,$,#61973,#61968)
REPRESENTATION_RELATIONSHIP_WITH_TRANSFORMATION(#100)
SHAPE_REPRESENTATION_RELATIONSHIP()
);
#193=(
REPRESENTATION_RELATIONSHIP($,$,#61974,#61968)
REPRESENTATION_RELATIONSHIP_WITH_TRANSFORMATION(#101)
SHAPE_REPRESENTATION_RELATIONSHIP()
);
#194=(
REPRESENTATION_RELATIONSHIP($,$,#61974,#61968)
REPRESENTATION_RELATIONSHIP_WITH_TRANSFORMATION(#102)
SHAPE_REPRESENTATION_RELATIONSHIP()
);
#195=(
REPRESENTATION_RELATIONSHIP($,$,#61974,#61968)
REPRESENTATION_RELATIONSHIP_WITH_TRANSFORMATION(#103)
SHAPE_REPRESENTATION_RELATIONSHIP()
);
#196=(
REPRESENTATION_RELATIONSHIP($,$,#61974,#61968)
REPRESENTATION_RELATIONSHIP_WITH_TRANSFORMATION(#104)
SHAPE_REPRESENTATION_RELATIONSHIP()
);
#197=(
REPRESENTATION_RELATIONSHIP($,$,#61975,#61968)
REPRESENTATION_RELATIONSHIP_WITH_TRANSFORMATION(#105)
SHAPE_REPRESENTATION_RELATIONSHIP()
);
#198=(
REPRESENTATION_RELATIONSHIP($,$,#61976,#61968)
REPRESENTATION_RELATIONSHIP_WITH_TRANSFORMATION(#106)
SHAPE_REPRESENTATION_RELATIONSHIP()
);
#199=(
REPRESENTATION_RELATIONSHIP($,$,#61977,#61968)
REPRESENTATION_RELATIONSHIP_WITH_TRANSFORMATION(#107)
SHAPE_REPRESENTATION_RELATIONSHIP()
);
#200=(
REPRESENTATION_RELATIONSHIP($,$,#61978,#61968)
REPRESENTATION_RELATIONSHIP_WITH_TRANSFORMATION(#108)
SHAPE_REPRESENTATION_RELATIONSHIP()
);
#201=(
REPRESENTATION_RELATIONSHIP($,$,#61979,#61968)
REPRESENTATION_RELATIONSHIP_WITH_TRANSFORMATION(#109)
SHAPE_REPRESENTATION_RELATIONSHIP()
);
#202=(
REPRESENTATION_RELATIONSHIP($,$,#61980,#61968)
REPRESENTATION_RELATIONSHIP_WITH_TRANSFORMATION(#110)
SHAPE_REPRESENTATION_RELATIONSHIP()
);
#203=(
REPRESENTATION_RELATIONSHIP($,$,#61987,#61968)
REPRESENTATION_RELATIONSHIP_WITH_TRANSFORMATION(#111)
SHAPE_REPRESENTATION_RELATIONSHIP()
);
#204=(
REPRESENTATION_RELATIONSHIP($,$,#61992,#61968)
REPRESENTATION_RELATIONSHIP_WITH_TRANSFORMATION(#112)
SHAPE_REPRESENTATION_RELATIONSHIP()
);
#205=(
REPRESENTATION_RELATIONSHIP($,$,#61995,#61968)
REPRESENTATION_RELATIONSHIP_WITH_TRANSFORMATION(#113)
SHAPE_REPRESENTATION_RELATIONSHIP()
);
#206=CONTEXT_DEPENDENT_SHAPE_REPRESENTATION(#114,#61865);
#207=CONTEXT_DEPENDENT_SHAPE_REPRESENTATION(#115,#61866);
#208=CONTEXT_DEPENDENT_SHAPE_REPRESENTATION(#116,#61867);
#209=CONTEXT_DEPENDENT_SHAPE_REPRESENTATION(#117,#61868);
#210=CONTEXT_DEPENDENT_SHAPE_REPRESENTATION(#118,#61869);
#211=CONTEXT_DEPENDENT_SHAPE_REPRESENTATION(#119,#61870);
#212=CONTEXT_DEPENDENT_SHAPE_REPRESENTATION(#120,#61871);
#213=CONTEXT_DEPENDENT_SHAPE_REPRESENTATION(#121,#61872);
#214=CONTEXT_DEPENDENT_SHAPE_REPRESENTATION(#122,#61873);
#215=CONTEXT_DEPENDENT_SHAPE_REPRESENTATION(#123,#61874);
#216=CONTEXT_DEPENDENT_SHAPE_REPRESENTATION(#124,#61875);
#217=CONTEXT_DEPENDENT_SHAPE_REPRESENTATION(#125,#61876);
#218=CONTEXT_DEPENDENT_SHAPE_REPRESENTATION(#126,#61877);
#219=CONTEXT_DEPENDENT_SHAPE_REPRESENTATION(#127,#61878);
#220=CONTEXT_DEPENDENT_SHAPE_REPRESENTATION(#128,#61879);
#221=CONTEXT_DEPENDENT_SHAPE_REPRESENTATION(#129,#61880);
#222=CONTEXT_DEPENDENT_SHAPE_REPRESENTATION(#130,#61886);
#223=CONTEXT_DEPENDENT_SHAPE_REPRESENTATION(#131,#61887);
#224=CONTEXT_DEPENDENT_SHAPE_REPRESENTATION(#132,#61888);
#225=CONTEXT_DEPENDENT_SHAPE_REPRESENTATION(#133,#61889);
#226=CONTEXT_DEPENDENT_SHAPE_REPRESENTATION(#134,#61890);
#227=CONTEXT_DEPENDENT_SHAPE_REPRESENTATION(#135,#61891);
#228=CONTEXT_DEPENDENT_SHAPE_REPRESENTATION(#136,#61892);
#229=CONTEXT_DEPENDENT_SHAPE_REPRESENTATION(#137,#61893);
#230=CONTEXT_DEPENDENT_SHAPE_REPRESENTATION(#138,#61894);
#231=CONTEXT_DEPENDENT_SHAPE_REPRESENTATION(#139,#61895);
#232=CONTEXT_DEPENDENT_SHAPE_REPRESENTATION(#140,#61896);
#233=CONTEXT_DEPENDENT_SHAPE_REPRESENTATION(#141,#61897);
#234=CONTEXT_DEPENDENT_SHAPE_REPRESENTATION(#142,#61898);
#235=CONTEXT_DEPENDENT_SHAPE_REPRESENTATION(#143,#61899);
#236=CONTEXT_DEPENDENT_SHAPE_REPRESENTATION(#144,#61900);
#237=CONTEXT_DEPENDENT_SHAPE_REPRESENTATION(#145,#61901);
#238=CONTEXT_DEPENDENT_SHAPE_REPRESENTATION(#146,#61905);
#239=CONTEXT_DEPENDENT_SHAPE_REPRESENTATION(#147,#61906);
#240=CONTEXT_DEPENDENT_SHAPE_REPRESENTATION(#148,#61910);
#241=CONTEXT_DEPENDENT_SHAPE_REPRESENTATION(#149,#61911);
#242=CONTEXT_DEPENDENT_SHAPE_REPRESENTATION(#150,#61912);
#243=CONTEXT_DEPENDENT_SHAPE_REPRESENTATION(#151,#61913);
#244=CONTEXT_DEPENDENT_SHAPE_REPRESENTATION(#152,#61914);
#245=CONTEXT_DEPENDENT_SHAPE_REPRESENTATION(#153,#61915);
#246=CONTEXT_DEPENDENT_SHAPE_REPRESENTATION(#154,#61916);
#247=CONTEXT_DEPENDENT_SHAPE_REPRESENTATION(#155,#61917);
#248=CONTEXT_DEPENDENT_SHAPE_REPRESENTATION(#156,#61918);
#249=CONTEXT_DEPENDENT_SHAPE_REPRESENTATION(#157,#61919);
#250=CONTEXT_DEPENDENT_SHAPE_REPRESENTATION(#158,#61920);
#251=CONTEXT_DEPENDENT_SHAPE_REPRESENTATION(#159,#61921);
#252=CONTEXT_DEPENDENT_SHAPE_REPRESENTATION(#160,#61922);
#253=CONTEXT_DEPENDENT_SHAPE_REPRESENTATION(#161,#61923);
#254=CONTEXT_DEPENDENT_SHAPE_REPRESENTATION(#162,#61924);
#255=CONTEXT_DEPENDENT_SHAPE_REPRESENTATION(#163,#61925);
#256=CONTEXT_DEPENDENT_SHAPE_REPRESENTATION(#164,#61926);
#257=CONTEXT_DEPENDENT_SHAPE_REPRESENTATION(#165,#61927);
#258=CONTEXT_DEPENDENT_SHAPE_REPRESENTATION(#166,#61928);
#259=CONTEXT_DEPENDENT_SHAPE_REPRESENTATION(#167,#61929);
#260=CONTEXT_DEPENDENT_SHAPE_REPRESENTATION(#168,#61930);
#261=CONTEXT_DEPENDENT_SHAPE_REPRESENTATION(#169,#61931);
#262=CONTEXT_DEPENDENT_SHAPE_REPRESENTATION(#170,#61932);
#263=CONTEXT_DEPENDENT_SHAPE_REPRESENTATION(#171,#61933);
#264=CONTEXT_DEPENDENT_SHAPE_REPRESENTATION(#172,#61934);
#265=CONTEXT_DEPENDENT_SHAPE_REPRESENTATION(#173,#61935);
#266=CONTEXT_DEPENDENT_SHAPE_REPRESENTATION(#174,#61936);
#267=CONTEXT_DEPENDENT_SHAPE_REPRESENTATION(#175,#61937);
#268=CONTEXT_DEPENDENT_SHAPE_REPRESENTATION(#176,#61938);
#269=CONTEXT_DEPENDENT_SHAPE_REPRESENTATION(#177,#61939);
#270=CONTEXT_DEPENDENT_SHAPE_REPRESENTATION(#178,#61940);
#271=CONTEXT_DEPENDENT_SHAPE_REPRESENTATION(#179,#61941);
#272=CONTEXT_DEPENDENT_SHAPE_REPRESENTATION(#180,#61942);
#273=CONTEXT_DEPENDENT_SHAPE_REPRESENTATION(#181,#61943);
#274=CONTEXT_DEPENDENT_SHAPE_REPRESENTATION(#182,#61944);
#275=CONTEXT_DEPENDENT_SHAPE_REPRESENTATION(#183,#61945);
#276=CONTEXT_DEPENDENT_SHAPE_REPRESENTATION(#184,#61946);
#277=CONTEXT_DEPENDENT_SHAPE_REPRESENTATION(#185,#61947);
#278=CONTEXT_DEPENDENT_SHAPE_REPRESENTATION(#186,#61948);
#279=CONTEXT_DEPENDENT_SHAPE_REPRESENTATION(#187,#61949);
#280=CONTEXT_DEPENDENT_SHAPE_REPRESENTATION(#188,#61950);
#281=CONTEXT_DEPENDENT_SHAPE_REPRESENTATION(#189,#61951);
#282=CONTEXT_DEPENDENT_SHAPE_REPRESENTATION(#190,#61952);
#283=CONTEXT_DEPENDENT_SHAPE_REPRESENTATION(#191,#61953);
#284=CONTEXT_DEPENDENT_SHAPE_REPRESENTATION(#192,#61954);
#285=CONTEXT_DEPENDENT_SHAPE_REPRESENTATION(#193,#61955);
#286=CONTEXT_DEPENDENT_SHAPE_REPRESENTATION(#194,#61956);
#287=CONTEXT_DEPENDENT_SHAPE_REPRESENTATION(#195,#61957);
#288=CONTEXT_DEPENDENT_SHAPE_REPRESENTATION(#196,#61958);
#289=CONTEXT_DEPENDENT_SHAPE_REPRESENTATION(#197,#61959);
#290=CONTEXT_DEPENDENT_SHAPE_REPRESENTATION(#198,#61960);
#291=CONTEXT_DEPENDENT_SHAPE_REPRESENTATION(#199,#61961);
#292=CONTEXT_DEPENDENT_SHAPE_REPRESENTATION(#200,#61962);
#293=CONTEXT_DEPENDENT_SHAPE_REPRESENTATION(#201,#61963);
#294=CONTEXT_DEPENDENT_SHAPE_REPRESENTATION(#202,#61964);
#295=CONTEXT_DEPENDENT_SHAPE_REPRESENTATION(#203,#61965);
#296=CONTEXT_DEPENDENT_SHAPE_REPRESENTATION(#204,#61966);
#297=CONTEXT_DEPENDENT_SHAPE_REPRESENTATION(#205,#61967);
#298=NEXT_ASSEMBLY_USAGE_OCCURRENCE('Chamber Housing:1',
'Chamber Housing:1','Chamber Housing:1',#62011,#62012,
'Chamber Housing:1');
#299=NEXT_ASSEMBLY_USAGE_OCCURRENCE('Left Side Plate:1',
'Left Side Plate:1','Left Side Plate:1',#62011,#62013,
'Left Side Plate:1');
#300=NEXT_ASSEMBLY_USAGE_OCCURRENCE('Right Side Plate:1',
'Right Side Plate:1','Right Side Plate:1',#62011,#62014,
'Right Side Plate:1');
#301=NEXT_ASSEMBLY_USAGE_OCCURRENCE('Front Plate:1','Front Plate:1',
'Front Plate:1',#62011,#62015,'Front Plate:1');
#302=NEXT_ASSEMBLY_USAGE_OCCURRENCE('Front Plate:2','Front Plate:2',
'Front Plate:2',#62011,#62015,'Front Plate:2');
#303=NEXT_ASSEMBLY_USAGE_OCCURRENCE('Stripper Fin:1','Stripper Fin:1',
'Stripper Fin:1',#62011,#62016,'Stripper Fin:1');
#304=NEXT_ASSEMBLY_USAGE_OCCURRENCE('Stripper Fin:2','Stripper Fin:2',
'Stripper Fin:2',#62011,#62016,'Stripper Fin:2');
#305=NEXT_ASSEMBLY_USAGE_OCCURRENCE('Stripper Fin:3','Stripper Fin:3',
'Stripper Fin:3',#62011,#62016,'Stripper Fin:3');
#306=NEXT_ASSEMBLY_USAGE_OCCURRENCE('Stripper Fin:4','Stripper Fin:4',
'Stripper Fin:4',#62011,#62016,'Stripper Fin:4');
#307=NEXT_ASSEMBLY_USAGE_OCCURRENCE('Stripper Fin:5','Stripper Fin:5',
'Stripper Fin:5',#62011,#62016,'Stripper Fin:5');
#308=NEXT_ASSEMBLY_USAGE_OCCURRENCE('Stripper Fin:6','Stripper Fin:6',
'Stripper Fin:6',#62011,#62016,'Stripper Fin:6');
#309=NEXT_ASSEMBLY_USAGE_OCCURRENCE('Stripper Fin:7','Stripper Fin:7',
'Stripper Fin:7',#62011,#62016,'Stripper Fin:7');
#310=NEXT_ASSEMBLY_USAGE_OCCURRENCE('Stripper Fin:8','Stripper Fin:8',
'Stripper Fin:8',#62011,#62016,'Stripper Fin:8');
#311=NEXT_ASSEMBLY_USAGE_OCCURRENCE('Stripper Fin:9','Stripper Fin:9',
'Stripper Fin:9',#62011,#62016,'Stripper Fin:9');
#312=NEXT_ASSEMBLY_USAGE_OCCURRENCE('Stripper Fin:10','Stripper Fin:10',
'Stripper Fin:10',#62011,#62016,'Stripper Fin:10');
#313=NEXT_ASSEMBLY_USAGE_OCCURRENCE('Chamber Base Plate:1',
'Chamber Base Plate:1','Chamber Base Plate:1',#62011,#62017,
'Chamber Base Plate:1');
#314=NEXT_ASSEMBLY_USAGE_OCCURRENCE('Cutter Shaft A:1',
'Cutter Shaft A:1','Cutter Shaft A:1',#62018,#62019,'Cutter Shaft A:1');
#315=NEXT_ASSEMBLY_USAGE_OCCURRENCE('Cutter Shaft B:1',
'Cutter Shaft B:1','Cutter Shaft B:1',#62018,#62020,'Cutter Shaft B:1');
#316=NEXT_ASSEMBLY_USAGE_OCCURRENCE('Shaft Spacer:1','Shaft Spacer:1',
'Shaft Spacer:1',#62018,#62021,'Shaft Spacer:1');
#317=NEXT_ASSEMBLY_USAGE_OCCURRENCE('Shaft Spacer:2','Shaft Spacer:2',
'Shaft Spacer:2',#62018,#62021,'Shaft Spacer:2');
#318=NEXT_ASSEMBLY_USAGE_OCCURRENCE('Shaft Spacer:3','Shaft Spacer:3',
'Shaft Spacer:3',#62018,#62021,'Shaft Spacer:3');
#319=NEXT_ASSEMBLY_USAGE_OCCURRENCE('Shaft Spacer:4','Shaft Spacer:4',
'Shaft Spacer:4',#62018,#62021,'Shaft Spacer:4');
#320=NEXT_ASSEMBLY_USAGE_OCCURRENCE('Shaft Spacer:5','Shaft Spacer:5',
'Shaft Spacer:5',#62018,#62021,'Shaft Spacer:5');
#321=NEXT_ASSEMBLY_USAGE_OCCURRENCE('Shaft Spacer:6','Shaft Spacer:6',
'Shaft Spacer:6',#62018,#62021,'Shaft Spacer:6');
#322=NEXT_ASSEMBLY_USAGE_OCCURRENCE('Shaft Spacer:7','Shaft Spacer:7',
'Shaft Spacer:7',#62018,#62021,'Shaft Spacer:7');
#323=NEXT_ASSEMBLY_USAGE_OCCURRENCE('Shaft Spacer:8','Shaft Spacer:8',
'Shaft Spacer:8',#62018,#62021,'Shaft Spacer:8');
#324=NEXT_ASSEMBLY_USAGE_OCCURRENCE('Shaft Spacer:9','Shaft Spacer:9',
'Shaft Spacer:9',#62018,#62021,'Shaft Spacer:9');
#325=NEXT_ASSEMBLY_USAGE_OCCURRENCE('Shaft Spacer:10','Shaft Spacer:10',
'Shaft Spacer:10',#62018,#62021,'Shaft Spacer:10');
#326=NEXT_ASSEMBLY_USAGE_OCCURRENCE('Shaft Washer:1','Shaft Washer:1',
'Shaft Washer:1',#62018,#62022,'Shaft Washer:1');
#327=NEXT_ASSEMBLY_USAGE_OCCURRENCE('Shaft Washer:2','Shaft Washer:2',
'Shaft Washer:2',#62018,#62022,'Shaft Washer:2');
#328=NEXT_ASSEMBLY_USAGE_OCCURRENCE('Shaft Washer:3','Shaft Washer:3',
'Shaft Washer:3',#62018,#62022,'Shaft Washer:3');
#329=NEXT_ASSEMBLY_USAGE_OCCURRENCE('Shaft Washer:4','Shaft Washer:4',
'Shaft Washer:4',#62018,#62022,'Shaft Washer:4');
#330=NEXT_ASSEMBLY_USAGE_OCCURRENCE('Large Spur Gear:1',
'Large Spur Gear:1','Large Spur Gear:1',#62023,#62024,
'Large Spur Gear:1');
#331=NEXT_ASSEMBLY_USAGE_OCCURRENCE('Small Spur Gear:1',
'Small Spur Gear:1','Small Spur Gear:1',#62023,#62025,
'Small Spur Gear:1');
#332=NEXT_ASSEMBLY_USAGE_OCCURRENCE('Gearbox Reducer:1',
'Gearbox Reducer:1','Gearbox Reducer:1',#62026,#62027,
'Gearbox Reducer:1');
#333=NEXT_ASSEMBLY_USAGE_OCCURRENCE('Shaft Coupling:1',
'Shaft Coupling:1','Shaft Coupling:1',#62026,#62028,'Shaft Coupling:1');
#334=NEXT_ASSEMBLY_USAGE_OCCURRENCE('Shredder Cutting Blades:1',
'Shredder Cutting Blades:1','Shredder Cutting Blades:1',#61999,#62000,
'Shredder Cutting Blades:1');
#335=NEXT_ASSEMBLY_USAGE_OCCURRENCE('Shredder Cutting Blades:2',
'Shredder Cutting Blades:2','Shredder Cutting Blades:2',#61999,#62000,
'Shredder Cutting Blades:2');
#336=NEXT_ASSEMBLY_USAGE_OCCURRENCE('Shredder Cutting Blades:3',
'Shredder Cutting Blades:3','Shredder Cutting Blades:3',#61999,#62000,
'Shredder Cutting Blades:3');
#337=NEXT_ASSEMBLY_USAGE_OCCURRENCE('Shredder Cutting Blades:4',
'Shredder Cutting Blades:4','Shredder Cutting Blades:4',#61999,#62000,
'Shredder Cutting Blades:4');
#338=NEXT_ASSEMBLY_USAGE_OCCURRENCE('Shredder Cutting Blades:5',
'Shredder Cutting Blades:5','Shredder Cutting Blades:5',#61999,#62000,
'Shredder Cutting Blades:5');
#339=NEXT_ASSEMBLY_USAGE_OCCURRENCE('Shredder Cutting Blades:6',
'Shredder Cutting Blades:6','Shredder Cutting Blades:6',#61999,#62000,
'Shredder Cutting Blades:6');
#340=NEXT_ASSEMBLY_USAGE_OCCURRENCE('Shredder Cutting Blades:7',
'Shredder Cutting Blades:7','Shredder Cutting Blades:7',#61999,#62000,
'Shredder Cutting Blades:7');
#341=NEXT_ASSEMBLY_USAGE_OCCURRENCE('Shredder Cutting Blades:8',
'Shredder Cutting Blades:8','Shredder Cutting Blades:8',#61999,#62000,
'Shredder Cutting Blades:8');
#342=NEXT_ASSEMBLY_USAGE_OCCURRENCE('Shredder Cutting Blades:9',
'Shredder Cutting Blades:9','Shredder Cutting Blades:9',#61999,#62000,
'Shredder Cutting Blades:9');
#343=NEXT_ASSEMBLY_USAGE_OCCURRENCE('Shredder Cutting Blades:10',
'Shredder Cutting Blades:10','Shredder Cutting Blades:10',#61999,#62000,
'Shredder Cutting Blades:10');
#344=NEXT_ASSEMBLY_USAGE_OCCURRENCE('Shaft Bearing Flange Units:1',
'Shaft Bearing Flange Units:1','Shaft Bearing Flange Units:1',#61999,#62001,
'Shaft Bearing Flange Units:1');
#345=NEXT_ASSEMBLY_USAGE_OCCURRENCE('Shaft Bearing Flange Units:2',
'Shaft Bearing Flange Units:2','Shaft Bearing Flange Units:2',#61999,#62001,
'Shaft Bearing Flange Units:2');
#346=NEXT_ASSEMBLY_USAGE_OCCURRENCE('Shaft Bearing Flange Units:3',
'Shaft Bearing Flange Units:3','Shaft Bearing Flange Units:3',#61999,#62001,
'Shaft Bearing Flange Units:3');
#347=NEXT_ASSEMBLY_USAGE_OCCURRENCE('Shaft Bearing Flange Units:4',
'Shaft Bearing Flange Units:4','Shaft Bearing Flange Units:4',#61999,#62001,
'Shaft Bearing Flange Units:4');
#348=NEXT_ASSEMBLY_USAGE_OCCURRENCE('Bearing Housing Socket Screws:1',
'Bearing Housing Socket Screws:1','Bearing Housing Socket Screws:1',#61999,
#62002,'Bearing Housing Socket Screws:1');
#349=NEXT_ASSEMBLY_USAGE_OCCURRENCE('Bearing Housing Socket Screws:2',
'Bearing Housing Socket Screws:2','Bearing Housing Socket Screws:2',#61999,
#62002,'Bearing Housing Socket Screws:2');
#350=NEXT_ASSEMBLY_USAGE_OCCURRENCE('Bearing Housing Socket Screws:3',
'Bearing Housing Socket Screws:3','Bearing Housing Socket Screws:3',#61999,
#62002,'Bearing Housing Socket Screws:3');
#351=NEXT_ASSEMBLY_USAGE_OCCURRENCE('Bearing Housing Socket Screws:4',
'Bearing Housing Socket Screws:4','Bearing Housing Socket Screws:4',#61999,
#62002,'Bearing Housing Socket Screws:4');
#352=NEXT_ASSEMBLY_USAGE_OCCURRENCE('Bearing Housing Socket Screws:5',
'Bearing Housing Socket Screws:5','Bearing Housing Socket Screws:5',#61999,
#62002,'Bearing Housing Socket Screws:5');
#353=NEXT_ASSEMBLY_USAGE_OCCURRENCE('Bearing Housing Socket Screws:6',
'Bearing Housing Socket Screws:6','Bearing Housing Socket Screws:6',#61999,
#62002,'Bearing Housing Socket Screws:6');
#354=NEXT_ASSEMBLY_USAGE_OCCURRENCE('Bearing Housing Socket Screws:7',
'Bearing Housing Socket Screws:7','Bearing Housing Socket Screws:7',#61999,
#62002,'Bearing Housing Socket Screws:7');
#355=NEXT_ASSEMBLY_USAGE_OCCURRENCE('Bearing Housing Socket Screws:8',
'Bearing Housing Socket Screws:8','Bearing Housing Socket Screws:8',#61999,
#62002,'Bearing Housing Socket Screws:8');
#356=NEXT_ASSEMBLY_USAGE_OCCURRENCE('Bearing Housing Socket Screws:9',
'Bearing Housing Socket Screws:9','Bearing Housing Socket Screws:9',#61999,
#62002,'Bearing Housing Socket Screws:9');
#357=NEXT_ASSEMBLY_USAGE_OCCURRENCE('Bearing Housing Socket Screws:10',
'Bearing Housing Socket Screws:10','Bearing Housing Socket Screws:10',#61999,
#62002,'Bearing Housing Socket Screws:10');
#358=NEXT_ASSEMBLY_USAGE_OCCURRENCE('Bearing Housing Socket Screws:11',
'Bearing Housing Socket Screws:11','Bearing Housing Socket Screws:11',#61999,
#62002,'Bearing Housing Socket Screws:11');
#359=NEXT_ASSEMBLY_USAGE_OCCURRENCE('Bearing Housing Socket Screws:12',
'Bearing Housing Socket Screws:12','Bearing Housing Socket Screws:12',#61999,
#62002,'Bearing Housing Socket Screws:12');
#360=NEXT_ASSEMBLY_USAGE_OCCURRENCE('Bearing Housing Socket Screws:13',
'Bearing Housing Socket Screws:13','Bearing Housing Socket Screws:13',#61999,
#62002,'Bearing Housing Socket Screws:13');
#361=NEXT_ASSEMBLY_USAGE_OCCURRENCE('Bearing Housing Socket Screws:14',
'Bearing Housing Socket Screws:14','Bearing Housing Socket Screws:14',#61999,
#62002,'Bearing Housing Socket Screws:14');
#362=NEXT_ASSEMBLY_USAGE_OCCURRENCE('Bearing Housing Socket Screws:15',
'Bearing Housing Socket Screws:15','Bearing Housing Socket Screws:15',#61999,
#62002,'Bearing Housing Socket Screws:15');
#363=NEXT_ASSEMBLY_USAGE_OCCURRENCE('Bearing Housing Socket Screws:16',
'Bearing Housing Socket Screws:16','Bearing Housing Socket Screws:16',#61999,
#62002,'Bearing Housing Socket Screws:16');
#364=NEXT_ASSEMBLY_USAGE_OCCURRENCE(
'Chamber Front Plate Socket Screws:1',
'Chamber Front Plate Socket Screws:1',
'Chamber Front Plate Socket Screws:1',#61999,#62003,
'Chamber Front Plate Socket Screws:1');
#365=NEXT_ASSEMBLY_USAGE_OCCURRENCE(
'Chamber Front Plate Socket Screws:2',
'Chamber Front Plate Socket Screws:2',
'Chamber Front Plate Socket Screws:2',#61999,#62003,
'Chamber Front Plate Socket Screws:2');
#366=NEXT_ASSEMBLY_USAGE_OCCURRENCE(
'Chamber Front Plate Socket Screws:3',
'Chamber Front Plate Socket Screws:3',
'Chamber Front Plate Socket Screws:3',#61999,#62003,
'Chamber Front Plate Socket Screws:3');
#367=NEXT_ASSEMBLY_USAGE_OCCURRENCE(
'Chamber Front Plate Socket Screws:4',
'Chamber Front Plate Socket Screws:4',
'Chamber Front Plate Socket Screws:4',#61999,#62003,
'Chamber Front Plate Socket Screws:4');
#368=NEXT_ASSEMBLY_USAGE_OCCURRENCE(
'Chamber Front Plate Socket Screws:5',
'Chamber Front Plate Socket Screws:5',
'Chamber Front Plate Socket Screws:5',#61999,#62003,
'Chamber Front Plate Socket Screws:5');
#369=NEXT_ASSEMBLY_USAGE_OCCURRENCE(
'Chamber Front Plate Socket Screws:6',
'Chamber Front Plate Socket Screws:6',
'Chamber Front Plate Socket Screws:6',#61999,#62003,
'Chamber Front Plate Socket Screws:6');
#370=NEXT_ASSEMBLY_USAGE_OCCURRENCE(
'Chamber Front Plate Socket Screws:7',
'Chamber Front Plate Socket Screws:7',
'Chamber Front Plate Socket Screws:7',#61999,#62003,
'Chamber Front Plate Socket Screws:7');
#371=NEXT_ASSEMBLY_USAGE_OCCURRENCE(
'Chamber Front Plate Socket Screws:8',
'Chamber Front Plate Socket Screws:8',
'Chamber Front Plate Socket Screws:8',#61999,#62003,
'Chamber Front Plate Socket Screws:8');
#372=NEXT_ASSEMBLY_USAGE_OCCURRENCE(
'Chamber Front Plate Socket Screws:9',
'Chamber Front Plate Socket Screws:9',
'Chamber Front Plate Socket Screws:9',#61999,#62003,
'Chamber Front Plate Socket Screws:9');
#373=NEXT_ASSEMBLY_USAGE_OCCURRENCE(
'Chamber Front Plate Socket Screws:10',
'Chamber Front Plate Socket Screws:10',
'Chamber Front Plate Socket Screws:10',#61999,#62003,
'Chamber Front Plate Socket Screws:10');
#374=NEXT_ASSEMBLY_USAGE_OCCURRENCE(
'Chamber Front Plate Socket Screws:11',
'Chamber Front Plate Socket Screws:11',
'Chamber Front Plate Socket Screws:11',#61999,#62003,
'Chamber Front Plate Socket Screws:11');
#375=NEXT_ASSEMBLY_USAGE_OCCURRENCE(
'Chamber Front Plate Socket Screws:12',
'Chamber Front Plate Socket Screws:12',
'Chamber Front Plate Socket Screws:12',#61999,#62003,
'Chamber Front Plate Socket Screws:12');
#376=NEXT_ASSEMBLY_USAGE_OCCURRENCE('Extended Housing Socket Screw:1',
'Extended Housing Socket Screw:1','Extended Housing Socket Screw:1',#61999,
#62004,'Extended Housing Socket Screw:1');
#377=NEXT_ASSEMBLY_USAGE_OCCURRENCE('Chamber Hex Head Bolts:1',
'Chamber Hex Head Bolts:1','Chamber Hex Head Bolts:1',#61999,#62005,
'Chamber Hex Head Bolts:1');
#378=NEXT_ASSEMBLY_USAGE_OCCURRENCE('Chamber Hex Head Bolts:2',
'Chamber Hex Head Bolts:2','Chamber Hex Head Bolts:2',#61999,#62005,
'Chamber Hex Head Bolts:2');
#379=NEXT_ASSEMBLY_USAGE_OCCURRENCE('Chamber Hex Head Bolts:3',
'Chamber Hex Head Bolts:3','Chamber Hex Head Bolts:3',#61999,#62005,
'Chamber Hex Head Bolts:3');
#380=NEXT_ASSEMBLY_USAGE_OCCURRENCE('Chamber Hex Head Bolts:4',
'Chamber Hex Head Bolts:4','Chamber Hex Head Bolts:4',#61999,#62005,
'Chamber Hex Head Bolts:4');
#381=NEXT_ASSEMBLY_USAGE_OCCURRENCE('Infeed Hopper Chute:1',
'Infeed Hopper Chute:1','Infeed Hopper Chute:1',#61999,#62006,
'Infeed Hopper Chute:1');
#382=NEXT_ASSEMBLY_USAGE_OCCURRENCE('Discharge Chute Funnel:1',
'Discharge Chute Funnel:1','Discharge Chute Funnel:1',#61999,#62007,
'Discharge Chute Funnel:1');
#383=NEXT_ASSEMBLY_USAGE_OCCURRENCE('Electric Drive Motor:1',
'Electric Drive Motor:1','Electric Drive Motor:1',#61999,#62008,
'Electric Drive Motor:1');
#384=NEXT_ASSEMBLY_USAGE_OCCURRENCE(
'Motor and Gearbox Mounting Plate:1',
'Motor and Gearbox Mounting Plate:1',
'Motor and Gearbox Mounting Plate:1',#61999,#62009,
'Motor and Gearbox Mounting Plate:1');
#385=NEXT_ASSEMBLY_USAGE_OCCURRENCE('Machine Frame Stand:1',
'Machine Frame Stand:1','Machine Frame Stand:1',#61999,#62010,
'Machine Frame Stand:1');
#386=NEXT_ASSEMBLY_USAGE_OCCURRENCE(
'Shredder Cutting Chamber Housing:1',
'Shredder Cutting Chamber Housing:1',
'Shredder Cutting Chamber Housing:1',#61999,#62011,
'Shredder Cutting Chamber Housing:1');
#387=NEXT_ASSEMBLY_USAGE_OCCURRENCE('Dual Cutter Shafts:1',
'Dual Cutter Shafts:1','Dual Cutter Shafts:1',#61999,#62018,
'Dual Cutter Shafts:1');
#388=NEXT_ASSEMBLY_USAGE_OCCURRENCE('Drive Reduction Gears:1',
'Drive Reduction Gears:1','Drive Reduction Gears:1',#61999,#62023,
'Drive Reduction Gears:1');
#389=NEXT_ASSEMBLY_USAGE_OCCURRENCE('Gearbox Reducer Unit:1',
'Gearbox Reducer Unit:1','Gearbox Reducer Unit:1',#61999,#62026,
'Gearbox Reducer Unit:1');
#390=ELLIPSE('',#35059,1.14442790218193,0.499999999899238);
#391=ELLIPSE('',#35060,1.14442790225741,0.499999999917943);
#392=ELLIPSE('',#35063,0.555857993550966,0.5);
#393=ELLIPSE('',#35139,0.555857993550966,0.5);
#394=ELLIPSE('',#35329,5.65685424949238,4.);
#395=ELLIPSE('',#35330,5.65685424949238,4.);
#396=ELLIPSE('',#35331,5.65685424949238,4.);
#397=ELLIPSE('',#35332,5.65685424949238,4.);
#398=ELLIPSE('',#35333,2.82842712474619,2.);
#399=ELLIPSE('',#35334,2.82842712474619,2.);
#400=ELLIPSE('',#35335,2.82842712474619,2.);
#401=ELLIPSE('',#35336,2.82842712474619,2.);
#402=ELLIPSE('',#35339,2.82842712474716,2.);
#403=ELLIPSE('',#35342,2.82842712474716,2.);
#404=ELLIPSE('',#35344,5.65685424949433,4.);
#405=ELLIPSE('',#35346,5.65685424949433,4.);
#406=ELLIPSE('',#35349,5.65685424949433,4.);
#407=ELLIPSE('',#35350,5.65685424949433,4.);
#408=ELLIPSE('',#35351,2.82842712474716,2.);
#409=ELLIPSE('',#35352,2.82842712474716,2.);
#410=ELLIPSE('',#35363,5.65685424949238,4.);
#411=ELLIPSE('',#35364,5.65685424949238,4.);
#412=ELLIPSE('',#35365,5.65685424949238,4.);
#413=ELLIPSE('',#35366,5.65685424949238,4.);
#414=ELLIPSE('',#35367,2.82842712474619,2.);
#415=ELLIPSE('',#35368,2.82842712474619,2.);
#416=ELLIPSE('',#35369,2.82842712474619,2.);
#417=ELLIPSE('',#35370,2.82842712474619,2.);
#418=ELLIPSE('',#35373,2.82842712474716,2.);
#419=ELLIPSE('',#35376,2.82842712474716,2.);
#420=ELLIPSE('',#35378,5.65685424949433,4.);
#421=ELLIPSE('',#35381,5.65685424949433,4.);
#422=ELLIPSE('',#35384,5.65685424949433,4.);
#423=ELLIPSE('',#35385,5.65685424949433,4.);
#424=ELLIPSE('',#35386,2.82842712474716,2.);
#425=ELLIPSE('',#35387,2.82842712474716,2.);
#426=ELLIPSE('',#35397,5.65685424949043,4.);
#427=ELLIPSE('',#35398,5.65685424949043,4.);
#428=ELLIPSE('',#35399,5.65685424949043,4.);
#429=ELLIPSE('',#35400,5.65685424949043,4.);
#430=ELLIPSE('',#35401,2.82842712474521,2.);
#431=ELLIPSE('',#35402,2.82842712474521,2.);
#432=ELLIPSE('',#35403,2.82842712474521,2.);
#433=ELLIPSE('',#35404,2.82842712474521,2.);
#434=ELLIPSE('',#35407,2.82842712474521,2.);
#435=ELLIPSE('',#35410,2.82842712474521,2.);
#436=ELLIPSE('',#35413,5.65685424949043,4.);
#437=ELLIPSE('',#35416,5.65685424949043,4.);
#438=ELLIPSE('',#35418,5.65685424949043,4.);
#439=ELLIPSE('',#35419,5.65685424949043,4.);
#440=ELLIPSE('',#35420,2.82842712474521,2.);
#441=ELLIPSE('',#35421,2.82842712474521,2.);
#442=ELLIPSE('',#35431,5.65685424949238,4.);
#443=ELLIPSE('',#35432,5.65685424949238,4.);
#444=ELLIPSE('',#35433,5.65685424949238,4.);
#445=ELLIPSE('',#35434,5.65685424949238,4.);
#446=ELLIPSE('',#35435,2.82842712474619,2.);
#447=ELLIPSE('',#35436,2.82842712474619,2.);
#448=ELLIPSE('',#35437,2.82842712474619,2.);
#449=ELLIPSE('',#35438,2.82842712474619,2.);
#450=ELLIPSE('',#35441,2.82842712474619,2.);
#451=ELLIPSE('',#35444,2.82842712474619,2.);
#452=ELLIPSE('',#35447,5.65685424949238,4.);
#453=ELLIPSE('',#35450,5.65685424949238,4.);
#454=ELLIPSE('',#35452,5.65685424949238,4.);
#455=ELLIPSE('',#35453,5.65685424949238,4.);
#456=ELLIPSE('',#35454,2.82842712474619,2.);
#457=ELLIPSE('',#35455,2.82842712474619,2.);
#458=ELLIPSE('',#37359,23.7795204048042,16.4507119775366);
#459=ELLIPSE('',#37368,23.7795204048042,16.4507119775362);
#460=ELLIPSE('',#37370,5.0654611915013,5.05947474242203);
#461=ELLIPSE('',#37371,5.307986116055,5.30171304685244);
#462=ELLIPSE('',#37381,5.06546119150016,5.0594747424216);
#463=ELLIPSE('',#37382,5.30798611605508,5.3017130468524);
#464=ELLIPSE('',#37390,28.8874406483305,28.8698432);
#465=ELLIPSE('',#37391,28.8874406483305,28.8698432);
#466=ELLIPSE('',#37396,28.8695481487031,28.8519616);
#467=ELLIPSE('',#37397,28.8695481487031,28.8519616);
#468=ELLIPSE('',#37482,23.7795204048045,16.4507119775369);
#469=ELLIPSE('',#37484,23.7795204048049,16.4507119775379);
#470=ELLIPSE('',#37887,838.618438479801,28.7580992116283);
#471=ELLIPSE('',#37889,839.102181389802,28.77690685743);
#472=ELLIPSE('',#37898,838.752454381848,28.7633083459289);
#473=ELLIPSE('',#37900,838.930999847209,28.7702505633731);
#474=B_SPLINE_SURFACE_WITH_KNOTS('',3,3,((#53444,#53445,#53446,#53447),
(#53448,#53449,#53450,#53451),(#53452,#53453,#53454,#53455),(#53456,#53457,
#53458,#53459)),.UNSPECIFIED.,.F.,.F.,.F.,(4,4),(4,4),(0.513291621409645,
1.),(-0.0253523930614869,0.),.UNSPECIFIED.);
#475=B_SPLINE_SURFACE_WITH_KNOTS('',3,3,((#53472,#53473,#53474,#53475),
(#53476,#53477,#53478,#53479),(#53480,#53481,#53482,#53483),(#53484,#53485,
#53486,#53487)),.UNSPECIFIED.,.F.,.F.,.F.,(4,4),(4,4),(0.513291621409645,
1.),(0.,0.0253730124676109),.UNSPECIFIED.);
#476=(
BOUNDED_CURVE()
B_SPLINE_CURVE(2,(#51009,#51010,#51011),.UNSPECIFIED.,.F.,.F.)
B_SPLINE_CURVE_WITH_KNOTS((3,3),(0.,0.58421806903896),.UNSPECIFIED.)
CURVE()
GEOMETRIC_REPRESENTATION_ITEM()
RATIONAL_B_SPLINE_CURVE((1.,1.15470053837925,1.))
REPRESENTATION_ITEM('')
);
#477=(
BOUNDED_CURVE()
B_SPLINE_CURVE(2,(#51016,#51017,#51018),.UNSPECIFIED.,.F.,.F.)
B_SPLINE_CURVE_WITH_KNOTS((3,3),(0.,0.584218069038959),.UNSPECIFIED.)
CURVE()
GEOMETRIC_REPRESENTATION_ITEM()
RATIONAL_B_SPLINE_CURVE((1.,1.15470053837925,1.))
REPRESENTATION_ITEM('')
);
#478=(
BOUNDED_CURVE()
B_SPLINE_CURVE(2,(#51022,#51023,#51024),.UNSPECIFIED.,.F.,.F.)
B_SPLINE_CURVE_WITH_KNOTS((3,3),(0.,0.584218069038959),.UNSPECIFIED.)
CURVE()
GEOMETRIC_REPRESENTATION_ITEM()
RATIONAL_B_SPLINE_CURVE((1.,1.15470053837925,1.))
REPRESENTATION_ITEM('')
);
#479=(
BOUNDED_CURVE()
B_SPLINE_CURVE(2,(#51028,#51029,#51030),.UNSPECIFIED.,.F.,.F.)
B_SPLINE_CURVE_WITH_KNOTS((3,3),(0.,0.58421806903896),.UNSPECIFIED.)
CURVE()
GEOMETRIC_REPRESENTATION_ITEM()
RATIONAL_B_SPLINE_CURVE((1.,1.15470053837925,1.))
REPRESENTATION_ITEM('')
);
#480=(
BOUNDED_CURVE()
B_SPLINE_CURVE(2,(#51034,#51035,#51036),.UNSPECIFIED.,.F.,.F.)
B_SPLINE_CURVE_WITH_KNOTS((3,3),(0.,0.292109034519478),.UNSPECIFIED.)
CURVE()
GEOMETRIC_REPRESENTATION_ITEM()
RATIONAL_B_SPLINE_CURVE((1.,1.07735026918962,1.07735026918962))
REPRESENTATION_ITEM('')
);
#481=(
BOUNDED_CURVE()
B_SPLINE_CURVE(2,(#51039,#51040,#51041),.UNSPECIFIED.,.F.,.F.)
B_SPLINE_CURVE_WITH_KNOTS((3,3),(0.292109034519478,0.584218069038959),
 .UNSPECIFIED.)
CURVE()
GEOMETRIC_REPRESENTATION_ITEM()
RATIONAL_B_SPLINE_CURVE((1.07735026918962,1.07735026918963,1.))
REPRESENTATION_ITEM('')
);
#482=(
BOUNDED_CURVE()
B_SPLINE_CURVE(2,(#51043,#51044,#51045),.UNSPECIFIED.,.F.,.F.)
B_SPLINE_CURVE_WITH_KNOTS((3,3),(0.,0.584218069038959),.UNSPECIFIED.)
CURVE()
GEOMETRIC_REPRESENTATION_ITEM()
RATIONAL_B_SPLINE_CURVE((1.,1.15470053837925,1.))
REPRESENTATION_ITEM('')
);
#483=(
BOUNDED_CURVE()
B_SPLINE_CURVE(2,(#51098,#51099,#51100),.UNSPECIFIED.,.F.,.F.)
B_SPLINE_CURVE_WITH_KNOTS((3,3),(0.,0.467374455231167),.UNSPECIFIED.)
CURVE()
GEOMETRIC_REPRESENTATION_ITEM()
RATIONAL_B_SPLINE_CURVE((1.,1.15470053837925,1.))
REPRESENTATION_ITEM('')
);
#484=(
BOUNDED_CURVE()
B_SPLINE_CURVE(2,(#51105,#51106,#51107),.UNSPECIFIED.,.F.,.F.)
B_SPLINE_CURVE_WITH_KNOTS((3,3),(0.,0.467374455231167),.UNSPECIFIED.)
CURVE()
GEOMETRIC_REPRESENTATION_ITEM()
RATIONAL_B_SPLINE_CURVE((1.,1.15470053837925,1.))
REPRESENTATION_ITEM('')
);
#485=(
BOUNDED_CURVE()
B_SPLINE_CURVE(2,(#51111,#51112,#51113),.UNSPECIFIED.,.F.,.F.)
B_SPLINE_CURVE_WITH_KNOTS((3,3),(0.,0.467374455231166),.UNSPECIFIED.)
CURVE()
GEOMETRIC_REPRESENTATION_ITEM()
RATIONAL_B_SPLINE_CURVE((1.,1.15470053837925,1.))
REPRESENTATION_ITEM('')
);
#486=(
BOUNDED_CURVE()
B_SPLINE_CURVE(2,(#51117,#51118,#51119),.UNSPECIFIED.,.F.,.F.)
B_SPLINE_CURVE_WITH_KNOTS((3,3),(0.,0.467374455231167),.UNSPECIFIED.)
CURVE()
GEOMETRIC_REPRESENTATION_ITEM()
RATIONAL_B_SPLINE_CURVE((1.,1.15470053837926,1.))
REPRESENTATION_ITEM('')
);
#487=(
BOUNDED_CURVE()
B_SPLINE_CURVE(2,(#51123,#51124,#51125),.UNSPECIFIED.,.F.,.F.)
B_SPLINE_CURVE_WITH_KNOTS((3,3),(0.,0.233687227615585),.UNSPECIFIED.)
CURVE()
GEOMETRIC_REPRESENTATION_ITEM()
RATIONAL_B_SPLINE_CURVE((1.,1.07735026918963,1.07735026918963))
REPRESENTATION_ITEM('')
);
#488=(
BOUNDED_CURVE()
B_SPLINE_CURVE(2,(#51128,#51129,#51130),.UNSPECIFIED.,.F.,.F.)
B_SPLINE_CURVE_WITH_KNOTS((3,3),(0.233687227615585,0.467374455231167),
 .UNSPECIFIED.)
CURVE()
GEOMETRIC_REPRESENTATION_ITEM()
RATIONAL_B_SPLINE_CURVE((1.07735026918963,1.07735026918962,1.))
REPRESENTATION_ITEM('')
);
#489=(
BOUNDED_CURVE()
B_SPLINE_CURVE(2,(#51132,#51133,#51134),.UNSPECIFIED.,.F.,.F.)
B_SPLINE_CURVE_WITH_KNOTS((3,3),(0.,0.467374455231167),.UNSPECIFIED.)
CURVE()
GEOMETRIC_REPRESENTATION_ITEM()
RATIONAL_B_SPLINE_CURVE((1.,1.15470053837925,1.))
REPRESENTATION_ITEM('')
);
#490=(
BOUNDED_CURVE()
B_SPLINE_CURVE(2,(#51187,#51188,#51189),.UNSPECIFIED.,.F.,.F.)
B_SPLINE_CURVE_WITH_KNOTS((3,3),(0.,0.467374455231167),.UNSPECIFIED.)
CURVE()
GEOMETRIC_REPRESENTATION_ITEM()
RATIONAL_B_SPLINE_CURVE((1.,1.15470053837925,1.))
REPRESENTATION_ITEM('')
);
#491=(
BOUNDED_CURVE()
B_SPLINE_CURVE(2,(#51194,#51195,#51196),.UNSPECIFIED.,.F.,.F.)
B_SPLINE_CURVE_WITH_KNOTS((3,3),(0.,0.467374455231167),.UNSPECIFIED.)
CURVE()
GEOMETRIC_REPRESENTATION_ITEM()
RATIONAL_B_SPLINE_CURVE((1.,1.15470053837925,1.))
REPRESENTATION_ITEM('')
);
#492=(
BOUNDED_CURVE()
B_SPLINE_CURVE(2,(#51200,#51201,#51202),.UNSPECIFIED.,.F.,.F.)
B_SPLINE_CURVE_WITH_KNOTS((3,3),(0.,0.467374455231166),.UNSPECIFIED.)
CURVE()
GEOMETRIC_REPRESENTATION_ITEM()
RATIONAL_B_SPLINE_CURVE((1.,1.15470053837925,1.))
REPRESENTATION_ITEM('')
);
#493=(
BOUNDED_CURVE()
B_SPLINE_CURVE(2,(#51206,#51207,#51208),.UNSPECIFIED.,.F.,.F.)
B_SPLINE_CURVE_WITH_KNOTS((3,3),(0.,0.467374455231167),.UNSPECIFIED.)
CURVE()
GEOMETRIC_REPRESENTATION_ITEM()
RATIONAL_B_SPLINE_CURVE((1.,1.15470053837926,1.))
REPRESENTATION_ITEM('')
);
#494=(
BOUNDED_CURVE()
B_SPLINE_CURVE(2,(#51212,#51213,#51214),.UNSPECIFIED.,.F.,.F.)
B_SPLINE_CURVE_WITH_KNOTS((3,3),(0.,0.233687227615584),.UNSPECIFIED.)
CURVE()
GEOMETRIC_REPRESENTATION_ITEM()
RATIONAL_B_SPLINE_CURVE((1.,1.07735026918963,1.07735026918963))
REPRESENTATION_ITEM('')
);
#495=(
BOUNDED_CURVE()
B_SPLINE_CURVE(2,(#51217,#51218,#51219),.UNSPECIFIED.,.F.,.F.)
B_SPLINE_CURVE_WITH_KNOTS((3,3),(0.233687227615584,0.467374455231167),
 .UNSPECIFIED.)
CURVE()
GEOMETRIC_REPRESENTATION_ITEM()
RATIONAL_B_SPLINE_CURVE((1.07735026918963,1.07735026918962,1.))
REPRESENTATION_ITEM('')
);
#496=(
BOUNDED_CURVE()
B_SPLINE_CURVE(2,(#51221,#51222,#51223),.UNSPECIFIED.,.F.,.F.)
B_SPLINE_CURVE_WITH_KNOTS((3,3),(0.,0.467374455231167),.UNSPECIFIED.)
CURVE()
GEOMETRIC_REPRESENTATION_ITEM()
RATIONAL_B_SPLINE_CURVE((1.,1.15470053837925,1.))
REPRESENTATION_ITEM('')
);
#497=(
BOUNDED_CURVE()
B_SPLINE_CURVE(2,(#51253,#51254,#51255),.UNSPECIFIED.,.F.,.F.)
B_SPLINE_CURVE_WITH_KNOTS((3,3),(0.46856777502019,0.937135550040381),
 .UNSPECIFIED.)
CURVE()
GEOMETRIC_REPRESENTATION_ITEM()
RATIONAL_B_SPLINE_CURVE((1.,1.03795484930203,1.))
REPRESENTATION_ITEM('')
);
#498=(
BOUNDED_CURVE()
B_SPLINE_CURVE(2,(#51258,#51259,#51260),.UNSPECIFIED.,.F.,.F.)
B_SPLINE_CURVE_WITH_KNOTS((3,3),(0.,0.468567775020191),.UNSPECIFIED.)
CURVE()
GEOMETRIC_REPRESENTATION_ITEM()
RATIONAL_B_SPLINE_CURVE((1.,1.03795484930204,1.))
REPRESENTATION_ITEM('')
);
#499=(
BOUNDED_CURVE()
B_SPLINE_CURVE(2,(#51264,#51265,#51266),.UNSPECIFIED.,.F.,.F.)
B_SPLINE_CURVE_WITH_KNOTS((3,3),(0.,0.468567775020191),.UNSPECIFIED.)
CURVE()
GEOMETRIC_REPRESENTATION_ITEM()
RATIONAL_B_SPLINE_CURVE((1.,1.03795484930204,1.))
REPRESENTATION_ITEM('')
);
#500=(
BOUNDED_CURVE()
B_SPLINE_CURVE(2,(#51267,#51268,#51269),.UNSPECIFIED.,.F.,.F.)
B_SPLINE_CURVE_WITH_KNOTS((3,3),(0.468567775020191,0.937135550040382),
 .UNSPECIFIED.)
CURVE()
GEOMETRIC_REPRESENTATION_ITEM()
RATIONAL_B_SPLINE_CURVE((1.,1.03795484930205,1.))
REPRESENTATION_ITEM('')
);
#501=(
BOUNDED_CURVE()
B_SPLINE_CURVE(2,(#51274,#51275,#51276),.UNSPECIFIED.,.F.,.F.)
B_SPLINE_CURVE_WITH_KNOTS((3,3),(0.468567775020191,0.937135550040382),
 .UNSPECIFIED.)
CURVE()
GEOMETRIC_REPRESENTATION_ITEM()
RATIONAL_B_SPLINE_CURVE((1.,1.03795484930204,1.))
REPRESENTATION_ITEM('')
);
#502=(
BOUNDED_CURVE()
B_SPLINE_CURVE(2,(#51278,#51279,#51280),.UNSPECIFIED.,.F.,.F.)
B_SPLINE_CURVE_WITH_KNOTS((3,3),(0.,0.46856777502019),.UNSPECIFIED.)
CURVE()
GEOMETRIC_REPRESENTATION_ITEM()
RATIONAL_B_SPLINE_CURVE((1.,1.03795484930204,1.))
REPRESENTATION_ITEM('')
);
#503=(
BOUNDED_CURVE()
B_SPLINE_CURVE(2,(#51284,#51285,#51286),.UNSPECIFIED.,.F.,.F.)
B_SPLINE_CURVE_WITH_KNOTS((3,3),(0.,0.468567775020191),.UNSPECIFIED.)
CURVE()
GEOMETRIC_REPRESENTATION_ITEM()
RATIONAL_B_SPLINE_CURVE((1.,1.03795484930203,1.))
REPRESENTATION_ITEM('')
);
#504=(
BOUNDED_CURVE()
B_SPLINE_CURVE(2,(#51287,#51288,#51289),.UNSPECIFIED.,.F.,.F.)
B_SPLINE_CURVE_WITH_KNOTS((3,3),(0.468567775020191,0.937135550040381),
 .UNSPECIFIED.)
CURVE()
GEOMETRIC_REPRESENTATION_ITEM()
RATIONAL_B_SPLINE_CURVE((1.,1.03795484930204,1.))
REPRESENTATION_ITEM('')
);
#505=(
BOUNDED_CURVE()
B_SPLINE_CURVE(2,(#51294,#51295,#51296),.UNSPECIFIED.,.F.,.F.)
B_SPLINE_CURVE_WITH_KNOTS((3,3),(0.468567775020191,0.937135550040381),
 .UNSPECIFIED.)
CURVE()
GEOMETRIC_REPRESENTATION_ITEM()
RATIONAL_B_SPLINE_CURVE((1.,1.03795484930203,1.))
REPRESENTATION_ITEM('')
);
#506=(
BOUNDED_CURVE()
B_SPLINE_CURVE(2,(#51298,#51299,#51300),.UNSPECIFIED.,.F.,.F.)
B_SPLINE_CURVE_WITH_KNOTS((3,3),(0.,0.468567775020191),.UNSPECIFIED.)
CURVE()
GEOMETRIC_REPRESENTATION_ITEM()
RATIONAL_B_SPLINE_CURVE((1.,1.03795484930204,1.))
REPRESENTATION_ITEM('')
);
#507=(
BOUNDED_CURVE()
B_SPLINE_CURVE(2,(#51303,#51304,#51305),.UNSPECIFIED.,.F.,.F.)
B_SPLINE_CURVE_WITH_KNOTS((3,3),(0.,0.468567775020191),.UNSPECIFIED.)
CURVE()
GEOMETRIC_REPRESENTATION_ITEM()
RATIONAL_B_SPLINE_CURVE((1.,1.03795484930203,1.))
REPRESENTATION_ITEM('')
);
#508=(
BOUNDED_CURVE()
B_SPLINE_CURVE(2,(#51306,#51307,#51308),.UNSPECIFIED.,.F.,.F.)
B_SPLINE_CURVE_WITH_KNOTS((3,3),(0.468567775020191,0.937135550040382),
 .UNSPECIFIED.)
CURVE()
GEOMETRIC_REPRESENTATION_ITEM()
RATIONAL_B_SPLINE_CURVE((1.,1.03795484930205,1.))
REPRESENTATION_ITEM('')
);
#509=(
BOUNDED_CURVE()
B_SPLINE_CURVE(2,(#51599,#51600,#51601),.UNSPECIFIED.,.F.,.F.)
B_SPLINE_CURVE_WITH_KNOTS((3,3),(-1.09670001953998,-0.838836123214499),
 .UNSPECIFIED.)
CURVE()
GEOMETRIC_REPRESENTATION_ITEM()
RATIONAL_B_SPLINE_CURVE((0.975084512183132,0.979302933905043,1.))
REPRESENTATION_ITEM('')
);
#510=(
BOUNDED_CURVE()
B_SPLINE_CURVE(2,(#52725,#52726,#52727,#52728,#52729),.UNSPECIFIED.,.F.,
 .F.)
B_SPLINE_CURVE_WITH_KNOTS((3,2,3),(4.71238779043687,5.49778654880823,6.28318530717959),
 .UNSPECIFIED.)
CURVE()
GEOMETRIC_REPRESENTATION_ITEM()
RATIONAL_B_SPLINE_CURVE((1.,0.923879418659198,1.,0.923879418650411,1.))
REPRESENTATION_ITEM('')
);
#511=(
BOUNDED_CURVE()
B_SPLINE_CURVE(2,(#58779,#58780,#58781),.UNSPECIFIED.,.F.,.F.)
B_SPLINE_CURVE_WITH_KNOTS((3,3),(-1.96119676425552,-0.523147579176476),
 .UNSPECIFIED.)
CURVE()
GEOMETRIC_REPRESENTATION_ITEM()
RATIONAL_B_SPLINE_CURVE((1.06676786887492,1.04969648457804,1.02176211535249))
REPRESENTATION_ITEM('')
);
#512=(
BOUNDED_CURVE()
B_SPLINE_CURVE(2,(#58801,#58802,#58803),.UNSPECIFIED.,.F.,.F.)
B_SPLINE_CURVE_WITH_KNOTS((3,3),(-7.9190884120588,-5.23007186679282),
 .UNSPECIFIED.)
CURVE()
GEOMETRIC_REPRESENTATION_ITEM()
RATIONAL_B_SPLINE_CURVE((1.02176211535249,1.07399675503552,1.08824844879795))
REPRESENTATION_ITEM('')
);
#513=(
BOUNDED_CURVE()
B_SPLINE_CURVE(2,(#58988,#58989,#58990),.UNSPECIFIED.,.F.,.F.)
B_SPLINE_CURVE_WITH_KNOTS((3,3),(5.23007186679282,7.9190884120588),
 .UNSPECIFIED.)
CURVE()
GEOMETRIC_REPRESENTATION_ITEM()
RATIONAL_B_SPLINE_CURVE((1.08824844879795,1.07399675503552,1.02176211535249))
REPRESENTATION_ITEM('')
);
#514=(
BOUNDED_CURVE()
B_SPLINE_CURVE(2,(#59004,#59005,#59006),.UNSPECIFIED.,.F.,.F.)
B_SPLINE_CURVE_WITH_KNOTS((3,3),(0.523147579176475,1.96119676425551),
 .UNSPECIFIED.)
CURVE()
GEOMETRIC_REPRESENTATION_ITEM()
RATIONAL_B_SPLINE_CURVE((1.02176211535249,1.04969648457805,1.06676786887492))
REPRESENTATION_ITEM('')
);
#515=(
BOUNDED_CURVE()
B_SPLINE_CURVE(2,(#59072,#59073,#59074),.UNSPECIFIED.,.F.,.F.)
B_SPLINE_CURVE_WITH_KNOTS((3,3),(0.,0.357592968100342),.UNSPECIFIED.)
CURVE()
GEOMETRIC_REPRESENTATION_ITEM()
RATIONAL_B_SPLINE_CURVE((1.,1.00186100329507,1.))
REPRESENTATION_ITEM('')
);
#516=(
BOUNDED_CURVE()
B_SPLINE_CURVE(2,(#59077,#59078,#59079),.UNSPECIFIED.,.F.,.F.)
B_SPLINE_CURVE_WITH_KNOTS((3,3),(0.,0.357592968100342),.UNSPECIFIED.)
CURVE()
GEOMETRIC_REPRESENTATION_ITEM()
RATIONAL_B_SPLINE_CURVE((1.,1.00186100329509,1.))
REPRESENTATION_ITEM('')
);
#517=(
BOUNDED_CURVE()
B_SPLINE_CURVE(2,(#59162,#59163,#59164),.UNSPECIFIED.,.F.,.F.)
B_SPLINE_CURVE_WITH_KNOTS((3,3),(1.4922333840247,2.15631214646323),
 .UNSPECIFIED.)
CURVE()
GEOMETRIC_REPRESENTATION_ITEM()
RATIONAL_B_SPLINE_CURVE((1.8473383335981,1.95114786800464,1.97954092996664))
REPRESENTATION_ITEM('')
);
#518=(
BOUNDED_CURVE()
B_SPLINE_CURVE(2,(#59168,#59169,#59170),.UNSPECIFIED.,.F.,.F.)
B_SPLINE_CURVE_WITH_KNOTS((3,3),(2.65634161849746,3.32042038093599),
 .UNSPECIFIED.)
CURVE()
GEOMETRIC_REPRESENTATION_ITEM()
RATIONAL_B_SPLINE_CURVE((1.97954092996664,1.95114786800464,1.8473383335981))
REPRESENTATION_ITEM('')
);
#519=(
BOUNDED_CURVE()
B_SPLINE_CURVE(2,(#59179,#59180,#59181),.UNSPECIFIED.,.F.,.F.)
B_SPLINE_CURVE_WITH_KNOTS((3,3),(1.4922333840247,2.15631214646323),
 .UNSPECIFIED.)
CURVE()
GEOMETRIC_REPRESENTATION_ITEM()
RATIONAL_B_SPLINE_CURVE((1.8473383335981,1.95114786800464,1.97954092996664))
REPRESENTATION_ITEM('')
);
#520=(
BOUNDED_CURVE()
B_SPLINE_CURVE(2,(#59184,#59185,#59186),.UNSPECIFIED.,.F.,.F.)
B_SPLINE_CURVE_WITH_KNOTS((3,3),(2.65634161849746,3.32042038093599),
 .UNSPECIFIED.)
CURVE()
GEOMETRIC_REPRESENTATION_ITEM()
RATIONAL_B_SPLINE_CURVE((1.97954092996664,1.95114786800464,1.8473383335981))
REPRESENTATION_ITEM('')
);
#521=(
BOUNDED_CURVE()
B_SPLINE_CURVE(2,(#59193,#59194,#59195),.UNSPECIFIED.,.F.,.F.)
B_SPLINE_CURVE_WITH_KNOTS((3,3),(1.4922333840247,2.15631214646323),
 .UNSPECIFIED.)
CURVE()
GEOMETRIC_REPRESENTATION_ITEM()
RATIONAL_B_SPLINE_CURVE((1.8473383335981,1.95114786800464,1.97954092996664))
REPRESENTATION_ITEM('')
);
#522=(
BOUNDED_CURVE()
B_SPLINE_CURVE(2,(#59198,#59199,#59200),.UNSPECIFIED.,.F.,.F.)
B_SPLINE_CURVE_WITH_KNOTS((3,3),(2.65634161849746,3.32042038093599),
 .UNSPECIFIED.)
CURVE()
GEOMETRIC_REPRESENTATION_ITEM()
RATIONAL_B_SPLINE_CURVE((1.97954092996664,1.95114786800464,1.8473383335981))
REPRESENTATION_ITEM('')
);
#523=(
BOUNDED_CURVE()
B_SPLINE_CURVE(2,(#59207,#59208,#59209),.UNSPECIFIED.,.F.,.F.)
B_SPLINE_CURVE_WITH_KNOTS((3,3),(1.4922333840247,2.15631214646323),
 .UNSPECIFIED.)
CURVE()
GEOMETRIC_REPRESENTATION_ITEM()
RATIONAL_B_SPLINE_CURVE((1.8473383335981,1.95114786800464,1.97954092996664))
REPRESENTATION_ITEM('')
);
#524=(
BOUNDED_CURVE()
B_SPLINE_CURVE(2,(#59212,#59213,#59214),.UNSPECIFIED.,.F.,.F.)
B_SPLINE_CURVE_WITH_KNOTS((3,3),(2.65634161849746,3.32042038093599),
 .UNSPECIFIED.)
CURVE()
GEOMETRIC_REPRESENTATION_ITEM()
RATIONAL_B_SPLINE_CURVE((1.97954092996664,1.95114786800464,1.8473383335981))
REPRESENTATION_ITEM('')
);
#525=(
BOUNDED_CURVE()
B_SPLINE_CURVE(2,(#59220,#59221,#59222),.UNSPECIFIED.,.F.,.F.)
B_SPLINE_CURVE_WITH_KNOTS((3,3),(-2.15631214646323,-1.4922333840247),
 .UNSPECIFIED.)
CURVE()
GEOMETRIC_REPRESENTATION_ITEM()
RATIONAL_B_SPLINE_CURVE((1.97954092996664,1.95114786800464,1.8473383335981))
REPRESENTATION_ITEM('')
);
#526=(
BOUNDED_CURVE()
B_SPLINE_CURVE(2,(#59229,#59230,#59231),.UNSPECIFIED.,.F.,.F.)
B_SPLINE_CURVE_WITH_KNOTS((3,3),(-3.32042038093599,-2.65634161849746),
 .UNSPECIFIED.)
CURVE()
GEOMETRIC_REPRESENTATION_ITEM()
RATIONAL_B_SPLINE_CURVE((1.8473383335981,1.95114786800464,1.97954092996664))
REPRESENTATION_ITEM('')
);
#527=(
BOUNDED_CURVE()
B_SPLINE_CURVE(2,(#59233,#59234,#59235),.UNSPECIFIED.,.F.,.F.)
B_SPLINE_CURVE_WITH_KNOTS((3,3),(-2.15631214646323,-1.4922333840247),
 .UNSPECIFIED.)
CURVE()
GEOMETRIC_REPRESENTATION_ITEM()
RATIONAL_B_SPLINE_CURVE((1.97954092996664,1.95114786800464,1.8473383335981))
REPRESENTATION_ITEM('')
);
#528=(
BOUNDED_CURVE()
B_SPLINE_CURVE(2,(#59239,#59240,#59241),.UNSPECIFIED.,.F.,.F.)
B_SPLINE_CURVE_WITH_KNOTS((3,3),(-3.32042038093599,-2.65634161849746),
 .UNSPECIFIED.)
CURVE()
GEOMETRIC_REPRESENTATION_ITEM()
RATIONAL_B_SPLINE_CURVE((1.8473383335981,1.95114786800464,1.97954092996664))
REPRESENTATION_ITEM('')
);
#529=(
BOUNDED_CURVE()
B_SPLINE_CURVE(2,(#59259,#59260,#59261),.UNSPECIFIED.,.F.,.F.)
B_SPLINE_CURVE_WITH_KNOTS((3,3),(1.4922333840247,2.15631214646323),
 .UNSPECIFIED.)
CURVE()
GEOMETRIC_REPRESENTATION_ITEM()
RATIONAL_B_SPLINE_CURVE((1.8473383335981,1.95114786800464,1.97954092996664))
REPRESENTATION_ITEM('')
);
#530=(
BOUNDED_CURVE()
B_SPLINE_CURVE(2,(#59265,#59266,#59267),.UNSPECIFIED.,.F.,.F.)
B_SPLINE_CURVE_WITH_KNOTS((3,3),(2.65634161849746,3.32042038093599),
 .UNSPECIFIED.)
CURVE()
GEOMETRIC_REPRESENTATION_ITEM()
RATIONAL_B_SPLINE_CURVE((1.97954092996664,1.95114786800464,1.8473383335981))
REPRESENTATION_ITEM('')
);
#531=(
BOUNDED_CURVE()
B_SPLINE_CURVE(2,(#59276,#59277,#59278),.UNSPECIFIED.,.F.,.F.)
B_SPLINE_CURVE_WITH_KNOTS((3,3),(1.4922333840247,2.15631214646323),
 .UNSPECIFIED.)
CURVE()
GEOMETRIC_REPRESENTATION_ITEM()
RATIONAL_B_SPLINE_CURVE((1.8473383335981,1.95114786800464,1.97954092996664))
REPRESENTATION_ITEM('')
);
#532=(
BOUNDED_CURVE()
B_SPLINE_CURVE(2,(#59281,#59282,#59283),.UNSPECIFIED.,.F.,.F.)
B_SPLINE_CURVE_WITH_KNOTS((3,3),(2.65634161849746,3.32042038093599),
 .UNSPECIFIED.)
CURVE()
GEOMETRIC_REPRESENTATION_ITEM()
RATIONAL_B_SPLINE_CURVE((1.97954092996664,1.95114786800464,1.8473383335981))
REPRESENTATION_ITEM('')
);
#533=(
BOUNDED_CURVE()
B_SPLINE_CURVE(2,(#59290,#59291,#59292),.UNSPECIFIED.,.F.,.F.)
B_SPLINE_CURVE_WITH_KNOTS((3,3),(1.4922333840247,2.15631214646323),
 .UNSPECIFIED.)
CURVE()
GEOMETRIC_REPRESENTATION_ITEM()
RATIONAL_B_SPLINE_CURVE((1.8473383335981,1.95114786800464,1.97954092996664))
REPRESENTATION_ITEM('')
);
#534=(
BOUNDED_CURVE()
B_SPLINE_CURVE(2,(#59295,#59296,#59297),.UNSPECIFIED.,.F.,.F.)
B_SPLINE_CURVE_WITH_KNOTS((3,3),(2.65634161849746,3.32042038093599),
 .UNSPECIFIED.)
CURVE()
GEOMETRIC_REPRESENTATION_ITEM()
RATIONAL_B_SPLINE_CURVE((1.97954092996664,1.95114786800464,1.8473383335981))
REPRESENTATION_ITEM('')
);
#535=(
BOUNDED_CURVE()
B_SPLINE_CURVE(2,(#59304,#59305,#59306),.UNSPECIFIED.,.F.,.F.)
B_SPLINE_CURVE_WITH_KNOTS((3,3),(1.4922333840247,2.15631214646323),
 .UNSPECIFIED.)
CURVE()
GEOMETRIC_REPRESENTATION_ITEM()
RATIONAL_B_SPLINE_CURVE((1.8473383335981,1.95114786800464,1.97954092996664))
REPRESENTATION_ITEM('')
);
#536=(
BOUNDED_CURVE()
B_SPLINE_CURVE(2,(#59309,#59310,#59311),.UNSPECIFIED.,.F.,.F.)
B_SPLINE_CURVE_WITH_KNOTS((3,3),(2.65634161849746,3.32042038093599),
 .UNSPECIFIED.)
CURVE()
GEOMETRIC_REPRESENTATION_ITEM()
RATIONAL_B_SPLINE_CURVE((1.97954092996664,1.95114786800464,1.8473383335981))
REPRESENTATION_ITEM('')
);
#537=(
BOUNDED_CURVE()
B_SPLINE_CURVE(2,(#59317,#59318,#59319),.UNSPECIFIED.,.F.,.F.)
B_SPLINE_CURVE_WITH_KNOTS((3,3),(-2.15631214646323,-1.4922333840247),
 .UNSPECIFIED.)
CURVE()
GEOMETRIC_REPRESENTATION_ITEM()
RATIONAL_B_SPLINE_CURVE((1.97954092996664,1.95114786800464,1.8473383335981))
REPRESENTATION_ITEM('')
);
#538=(
BOUNDED_CURVE()
B_SPLINE_CURVE(2,(#59326,#59327,#59328),.UNSPECIFIED.,.F.,.F.)
B_SPLINE_CURVE_WITH_KNOTS((3,3),(-3.32042038093599,-2.65634161849746),
 .UNSPECIFIED.)
CURVE()
GEOMETRIC_REPRESENTATION_ITEM()
RATIONAL_B_SPLINE_CURVE((1.8473383335981,1.95114786800464,1.97954092996664))
REPRESENTATION_ITEM('')
);
#539=(
BOUNDED_CURVE()
B_SPLINE_CURVE(2,(#59330,#59331,#59332),.UNSPECIFIED.,.F.,.F.)
B_SPLINE_CURVE_WITH_KNOTS((3,3),(-2.15631214646323,-1.4922333840247),
 .UNSPECIFIED.)
CURVE()
GEOMETRIC_REPRESENTATION_ITEM()
RATIONAL_B_SPLINE_CURVE((1.97954092996664,1.95114786800464,1.8473383335981))
REPRESENTATION_ITEM('')
);
#540=(
BOUNDED_CURVE()
B_SPLINE_CURVE(2,(#59336,#59337,#59338),.UNSPECIFIED.,.F.,.F.)
B_SPLINE_CURVE_WITH_KNOTS((3,3),(-3.32042038093599,-2.65634161849746),
 .UNSPECIFIED.)
CURVE()
GEOMETRIC_REPRESENTATION_ITEM()
RATIONAL_B_SPLINE_CURVE((1.8473383335981,1.95114786800464,1.97954092996664))
REPRESENTATION_ITEM('')
);
#541=(
BOUNDED_CURVE()
B_SPLINE_CURVE(2,(#60436,#60437,#60438),.UNSPECIFIED.,.F.,.F.)
B_SPLINE_CURVE_WITH_KNOTS((3,3),(1.4922333840247,2.15631214646323),
 .UNSPECIFIED.)
CURVE()
GEOMETRIC_REPRESENTATION_ITEM()
RATIONAL_B_SPLINE_CURVE((1.8473383335981,1.95114786800464,1.97954092996664))
REPRESENTATION_ITEM('')
);
#542=(
BOUNDED_CURVE()
B_SPLINE_CURVE(2,(#60439,#60440,#60441),.UNSPECIFIED.,.F.,.F.)
B_SPLINE_CURVE_WITH_KNOTS((3,3),(2.65634161849746,3.32042038093599),
 .UNSPECIFIED.)
CURVE()
GEOMETRIC_REPRESENTATION_ITEM()
RATIONAL_B_SPLINE_CURVE((1.97954092996664,1.95114786800464,1.8473383335981))
REPRESENTATION_ITEM('')
);
#543=(
BOUNDED_CURVE()
B_SPLINE_CURVE(2,(#60444,#60445,#60446),.UNSPECIFIED.,.F.,.F.)
B_SPLINE_CURVE_WITH_KNOTS((3,3),(-3.32042038093599,-2.65634161849746),
 .UNSPECIFIED.)
CURVE()
GEOMETRIC_REPRESENTATION_ITEM()
RATIONAL_B_SPLINE_CURVE((1.8473383335981,1.95114786800464,1.97954092996664))
REPRESENTATION_ITEM('')
);
#544=(
BOUNDED_CURVE()
B_SPLINE_CURVE(2,(#60448,#60449,#60450),.UNSPECIFIED.,.F.,.F.)
B_SPLINE_CURVE_WITH_KNOTS((3,3),(-2.15631214646323,-1.4922333840247),
 .UNSPECIFIED.)
CURVE()
GEOMETRIC_REPRESENTATION_ITEM()
RATIONAL_B_SPLINE_CURVE((1.97954092996664,1.95114786800464,1.8473383335981))
REPRESENTATION_ITEM('')
);
#545=(
BOUNDED_CURVE()
B_SPLINE_CURVE(2,(#60455,#60456,#60457),.UNSPECIFIED.,.F.,.F.)
B_SPLINE_CURVE_WITH_KNOTS((3,3),(-3.32042038093599,-2.65634161849746),
 .UNSPECIFIED.)
CURVE()
GEOMETRIC_REPRESENTATION_ITEM()
RATIONAL_B_SPLINE_CURVE((1.8473383335981,1.95114786800464,1.97954092996664))
REPRESENTATION_ITEM('')
);
#546=(
BOUNDED_CURVE()
B_SPLINE_CURVE(2,(#60458,#60459,#60460),.UNSPECIFIED.,.F.,.F.)
B_SPLINE_CURVE_WITH_KNOTS((3,3),(-2.15631214646323,-1.4922333840247),
 .UNSPECIFIED.)
CURVE()
GEOMETRIC_REPRESENTATION_ITEM()
RATIONAL_B_SPLINE_CURVE((1.97954092996664,1.95114786800464,1.8473383335981))
REPRESENTATION_ITEM('')
);
#547=(
BOUNDED_CURVE()
B_SPLINE_CURVE(2,(#60464,#60465,#60466),.UNSPECIFIED.,.F.,.F.)
B_SPLINE_CURVE_WITH_KNOTS((3,3),(2.65634161849746,3.32042038093599),
 .UNSPECIFIED.)
CURVE()
GEOMETRIC_REPRESENTATION_ITEM()
RATIONAL_B_SPLINE_CURVE((1.97954092996664,1.95114786800464,1.8473383335981))
REPRESENTATION_ITEM('')
);
#548=(
BOUNDED_CURVE()
B_SPLINE_CURVE(2,(#60467,#60468,#60469),.UNSPECIFIED.,.F.,.F.)
B_SPLINE_CURVE_WITH_KNOTS((3,3),(1.4922333840247,2.15631214646323),
 .UNSPECIFIED.)
CURVE()
GEOMETRIC_REPRESENTATION_ITEM()
RATIONAL_B_SPLINE_CURVE((1.8473383335981,1.95114786800464,1.97954092996664))
REPRESENTATION_ITEM('')
);
#549=(
BOUNDED_CURVE()
B_SPLINE_CURVE(2,(#60471,#60472,#60473),.UNSPECIFIED.,.F.,.F.)
B_SPLINE_CURVE_WITH_KNOTS((3,3),(2.65634161849746,3.32042038093599),
 .UNSPECIFIED.)
CURVE()
GEOMETRIC_REPRESENTATION_ITEM()
RATIONAL_B_SPLINE_CURVE((1.97954092996664,1.95114786800464,1.8473383335981))
REPRESENTATION_ITEM('')
);
#550=(
BOUNDED_CURVE()
B_SPLINE_CURVE(2,(#60477,#60478,#60479),.UNSPECIFIED.,.F.,.F.)
B_SPLINE_CURVE_WITH_KNOTS((3,3),(2.65634161849746,3.32042038093599),
 .UNSPECIFIED.)
CURVE()
GEOMETRIC_REPRESENTATION_ITEM()
RATIONAL_B_SPLINE_CURVE((1.97954092996664,1.95114786800464,1.8473383335981))
REPRESENTATION_ITEM('')
);
#551=(
BOUNDED_CURVE()
B_SPLINE_CURVE(2,(#60480,#60481,#60482),.UNSPECIFIED.,.F.,.F.)
B_SPLINE_CURVE_WITH_KNOTS((3,3),(1.4922333840247,2.15631214646323),
 .UNSPECIFIED.)
CURVE()
GEOMETRIC_REPRESENTATION_ITEM()
RATIONAL_B_SPLINE_CURVE((1.8473383335981,1.95114786800464,1.97954092996664))
REPRESENTATION_ITEM('')
);
#552=(
BOUNDED_CURVE()
B_SPLINE_CURVE(2,(#60484,#60485,#60486),.UNSPECIFIED.,.F.,.F.)
B_SPLINE_CURVE_WITH_KNOTS((3,3),(1.4922333840247,2.15631214646323),
 .UNSPECIFIED.)
CURVE()
GEOMETRIC_REPRESENTATION_ITEM()
RATIONAL_B_SPLINE_CURVE((1.8473383335981,1.95114786800464,1.97954092996664))
REPRESENTATION_ITEM('')
);
#553=(
BOUNDED_CURVE()
B_SPLINE_CURVE(2,(#60521,#60522,#60523),.UNSPECIFIED.,.F.,.F.)
B_SPLINE_CURVE_WITH_KNOTS((3,3),(1.4922333840247,2.15631214646323),
 .UNSPECIFIED.)
CURVE()
GEOMETRIC_REPRESENTATION_ITEM()
RATIONAL_B_SPLINE_CURVE((1.8473383335981,1.95114786800464,1.97954092996664))
REPRESENTATION_ITEM('')
);
#554=(
BOUNDED_CURVE()
B_SPLINE_CURVE(2,(#60524,#60525,#60526),.UNSPECIFIED.,.F.,.F.)
B_SPLINE_CURVE_WITH_KNOTS((3,3),(2.65634161849746,3.32042038093599),
 .UNSPECIFIED.)
CURVE()
GEOMETRIC_REPRESENTATION_ITEM()
RATIONAL_B_SPLINE_CURVE((1.97954092996664,1.95114786800464,1.8473383335981))
REPRESENTATION_ITEM('')
);
#555=(
BOUNDED_CURVE()
B_SPLINE_CURVE(2,(#60529,#60530,#60531),.UNSPECIFIED.,.F.,.F.)
B_SPLINE_CURVE_WITH_KNOTS((3,3),(-3.32042038093599,-2.65634161849746),
 .UNSPECIFIED.)
CURVE()
GEOMETRIC_REPRESENTATION_ITEM()
RATIONAL_B_SPLINE_CURVE((1.8473383335981,1.95114786800464,1.97954092996664))
REPRESENTATION_ITEM('')
);
#556=(
BOUNDED_CURVE()
B_SPLINE_CURVE(2,(#60533,#60534,#60535),.UNSPECIFIED.,.F.,.F.)
B_SPLINE_CURVE_WITH_KNOTS((3,3),(-2.15631214646323,-1.4922333840247),
 .UNSPECIFIED.)
CURVE()
GEOMETRIC_REPRESENTATION_ITEM()
RATIONAL_B_SPLINE_CURVE((1.97954092996664,1.95114786800464,1.8473383335981))
REPRESENTATION_ITEM('')
);
#557=(
BOUNDED_CURVE()
B_SPLINE_CURVE(2,(#60540,#60541,#60542),.UNSPECIFIED.,.F.,.F.)
B_SPLINE_CURVE_WITH_KNOTS((3,3),(-3.32042038093599,-2.65634161849746),
 .UNSPECIFIED.)
CURVE()
GEOMETRIC_REPRESENTATION_ITEM()
RATIONAL_B_SPLINE_CURVE((1.8473383335981,1.95114786800464,1.97954092996664))
REPRESENTATION_ITEM('')
);
#558=(
BOUNDED_CURVE()
B_SPLINE_CURVE(2,(#60543,#60544,#60545),.UNSPECIFIED.,.F.,.F.)
B_SPLINE_CURVE_WITH_KNOTS((3,3),(-2.15631214646323,-1.4922333840247),
 .UNSPECIFIED.)
CURVE()
GEOMETRIC_REPRESENTATION_ITEM()
RATIONAL_B_SPLINE_CURVE((1.97954092996664,1.95114786800464,1.8473383335981))
REPRESENTATION_ITEM('')
);
#559=(
BOUNDED_CURVE()
B_SPLINE_CURVE(2,(#60549,#60550,#60551),.UNSPECIFIED.,.F.,.F.)
B_SPLINE_CURVE_WITH_KNOTS((3,3),(2.65634161849746,3.32042038093599),
 .UNSPECIFIED.)
CURVE()
GEOMETRIC_REPRESENTATION_ITEM()
RATIONAL_B_SPLINE_CURVE((1.97954092996664,1.95114786800464,1.8473383335981))
REPRESENTATION_ITEM('')
);
#560=(
BOUNDED_CURVE()
B_SPLINE_CURVE(2,(#60552,#60553,#60554),.UNSPECIFIED.,.F.,.F.)
B_SPLINE_CURVE_WITH_KNOTS((3,3),(1.4922333840247,2.15631214646323),
 .UNSPECIFIED.)
CURVE()
GEOMETRIC_REPRESENTATION_ITEM()
RATIONAL_B_SPLINE_CURVE((1.8473383335981,1.95114786800464,1.97954092996664))
REPRESENTATION_ITEM('')
);
#561=(
BOUNDED_CURVE()
B_SPLINE_CURVE(2,(#60556,#60557,#60558),.UNSPECIFIED.,.F.,.F.)
B_SPLINE_CURVE_WITH_KNOTS((3,3),(2.65634161849746,3.32042038093599),
 .UNSPECIFIED.)
CURVE()
GEOMETRIC_REPRESENTATION_ITEM()
RATIONAL_B_SPLINE_CURVE((1.97954092996664,1.95114786800464,1.8473383335981))
REPRESENTATION_ITEM('')
);
#562=(
BOUNDED_CURVE()
B_SPLINE_CURVE(2,(#60562,#60563,#60564),.UNSPECIFIED.,.F.,.F.)
B_SPLINE_CURVE_WITH_KNOTS((3,3),(2.65634161849746,3.32042038093599),
 .UNSPECIFIED.)
CURVE()
GEOMETRIC_REPRESENTATION_ITEM()
RATIONAL_B_SPLINE_CURVE((1.97954092996664,1.95114786800464,1.8473383335981))
REPRESENTATION_ITEM('')
);
#563=(
BOUNDED_CURVE()
B_SPLINE_CURVE(2,(#60565,#60566,#60567),.UNSPECIFIED.,.F.,.F.)
B_SPLINE_CURVE_WITH_KNOTS((3,3),(1.4922333840247,2.15631214646323),
 .UNSPECIFIED.)
CURVE()
GEOMETRIC_REPRESENTATION_ITEM()
RATIONAL_B_SPLINE_CURVE((1.8473383335981,1.95114786800464,1.97954092996664))
REPRESENTATION_ITEM('')
);
#564=(
BOUNDED_CURVE()
B_SPLINE_CURVE(2,(#60569,#60570,#60571),.UNSPECIFIED.,.F.,.F.)
B_SPLINE_CURVE_WITH_KNOTS((3,3),(1.4922333840247,2.15631214646323),
 .UNSPECIFIED.)
CURVE()
GEOMETRIC_REPRESENTATION_ITEM()
RATIONAL_B_SPLINE_CURVE((1.8473383335981,1.95114786800464,1.97954092996664))
REPRESENTATION_ITEM('')
);
#565=CONICAL_SURFACE('',#34403,5.46323125,0.785398163397447);
#566=CONICAL_SURFACE('',#34419,2.88675134594813,1.0471975511966);
#567=CONICAL_SURFACE('',#34431,4.5399125,0.785398163397448);
#568=CONICAL_SURFACE('',#34447,2.3094010767585,1.0471975511966);
#569=CONICAL_SURFACE('',#34459,4.5399125,0.785398163397448);
#570=CONICAL_SURFACE('',#34475,2.3094010767585,1.0471975511966);
#571=CONICAL_SURFACE('',#34487,4.5399125,0.785343828859754);
#572=CONICAL_SURFACE('',#34490,8.618802153517,1.0471975511966);
#573=CONICAL_SURFACE('',#34492,8.618802153517,1.0471975511966);
#574=CONICAL_SURFACE('',#34494,8.618802153517,1.0471975511966);
#575=CONICAL_SURFACE('',#34496,8.618802153517,1.0471975511966);
#576=CONICAL_SURFACE('',#34498,8.618802153517,1.0471975511966);
#577=CONICAL_SURFACE('',#34500,8.618802153517,1.0471975511966);
#578=CONICAL_SURFACE('',#34877,3.98868900000005,0.78539816339748);
#579=CONICAL_SURFACE('',#34884,3.98868900000002,0.785398163397457);
#580=CONICAL_SURFACE('',#34891,3.98868900000004,0.785398163397464);
#581=CONICAL_SURFACE('',#34898,3.98868900000001,0.785398163397455);
#582=CONICAL_SURFACE('',#34900,82.8587325401841,0.0174532925199438);
#583=CONICAL_SURFACE('',#35152,5.68799999999971,0.785398163207466);
#584=CONICAL_SURFACE('',#35157,5.68799999999971,0.785398163337269);
#585=CONICAL_SURFACE('',#35162,5.68799999999971,0.785398163337269);
#586=CONICAL_SURFACE('',#35167,5.68799999999971,0.785398163207466);
#587=CONICAL_SURFACE('',#35172,5.688,0.785398163397448);
#588=CONICAL_SURFACE('',#35173,5.688,0.785398163397442);
#589=CONICAL_SURFACE('',#35174,5.688,0.785398163397442);
#590=CONICAL_SURFACE('',#35175,5.688,0.785398163397448);
#591=CONICAL_SURFACE('',#35772,2.094,1.02974425867665);
#592=CONICAL_SURFACE('',#35775,2.094,1.02974425867665);
#593=CONICAL_SURFACE('',#35778,2.094,1.02974425867665);
#594=CONICAL_SURFACE('',#35781,2.094,1.02974425867665);
#595=CONICAL_SURFACE('',#35784,2.094,1.02974425867665);
#596=CONICAL_SURFACE('',#35787,2.094,1.02974425867665);
#597=CONICAL_SURFACE('',#35833,2.094,1.02974425867665);
#598=CONICAL_SURFACE('',#35836,2.094,1.02974425867665);
#599=CONICAL_SURFACE('',#35839,2.094,1.02974425867665);
#600=CONICAL_SURFACE('',#35842,2.094,1.02974425867665);
#601=CONICAL_SURFACE('',#35845,2.094,1.02974425867665);
#602=CONICAL_SURFACE('',#35848,2.094,1.02974425867665);
#603=CONICAL_SURFACE('',#35992,18.25,0.785398163397426);
#604=CONICAL_SURFACE('',#35998,18.25,0.78539816339745);
#605=CONICAL_SURFACE('',#36004,14.5,0.785398163397442);
#606=CONICAL_SURFACE('',#36017,14.5,0.785398163397442);
#607=CONICAL_SURFACE('',#36025,19.75,0.78539816339745);
#608=CONICAL_SURFACE('',#36026,19.75,0.78539816339745);
#609=CONICAL_SURFACE('',#36036,12.25,0.785398163397429);
#610=CONICAL_SURFACE('',#36043,14.75,0.785398163397442);
#611=CONICAL_SURFACE('',#36058,18.25,0.785398163397442);
#612=CONICAL_SURFACE('',#36079,18.25,0.78539816339745);
#613=CONICAL_SURFACE('',#36085,14.5,0.785398163397445);
#614=CONICAL_SURFACE('',#36103,19.75,0.78539816339745);
#615=CONICAL_SURFACE('',#36104,19.75,0.78539816339745);
#616=CONICAL_SURFACE('',#37248,3.21359174399996,0.785398163397452);
#617=CONICAL_SURFACE('',#37253,0.322047616000012,1.0471975511966);
#618=CONICAL_SURFACE('',#37265,3.21359174400012,0.785398163397384);
#619=CONICAL_SURFACE('',#37270,0.322047616,1.04719755119659);
#620=CONICAL_SURFACE('',#37282,2.74142809600001,0.785398163397436);
#621=CONICAL_SURFACE('',#37290,0.274750783999988,1.04719755119659);
#622=CONICAL_SURFACE('',#37307,3.21359174400008,0.785398163397464);
#623=CONICAL_SURFACE('',#37315,0.322047616,1.04719755119659);
#624=CONICAL_SURFACE('',#37324,3.21359174399998,0.785398163397522);
#625=CONICAL_SURFACE('',#37332,0.322047616000012,1.04719755119659);
#626=CONICAL_SURFACE('',#37334,62.4381557149574,0.0364929375524579);
#627=CONICAL_SURFACE('',#37338,62.4381557149626,0.0364929375527776);
#628=CONICAL_SURFACE('',#37404,28.7625535999985,0.785398163397467);
#629=CONICAL_SURFACE('',#37440,6.37205498762855,1.04719755119635);
#630=CONICAL_SURFACE('',#37442,6.37205498762726,1.04719755119649);
#631=CONICAL_SURFACE('',#37444,6.37205498762869,1.04719755119634);
#632=CONICAL_SURFACE('',#37446,6.37205498762701,1.04719755119652);
#633=CONICAL_SURFACE('',#37448,6.37205498762724,1.04719755119655);
#634=CONICAL_SURFACE('',#37452,6.37205498762882,1.04719755119634);
#635=CONICAL_SURFACE('',#37459,6.37205498762342,1.04719755119681);
#636=CONICAL_SURFACE('',#37461,6.37205498762507,1.04719755119686);
#637=CONICAL_SURFACE('',#37463,6.37205498763146,1.04719755119606);
#638=CONICAL_SURFACE('',#37465,6.37205498762404,1.04719755119683);
#639=CONICAL_SURFACE('',#37467,6.37205498762824,1.04719755119636);
#640=CONICAL_SURFACE('',#37471,6.37205498763465,1.04719755119586);
#641=CONICAL_SURFACE('',#37485,17.3000533734216,0.0872664625997182);
#642=CONICAL_SURFACE('',#37486,5.46753820577589,0.769793460898297);
#643=CONICAL_SURFACE('',#37488,5.24100524633615,0.769793460899118);
#644=CONICAL_SURFACE('',#37497,5.24100524634338,0.769793460898339);
#645=CONICAL_SURFACE('',#37507,5.46753820577565,0.769793460898311);
#646=CONICAL_SURFACE('',#37515,5.83240278777977,0.769793460898674);
#647=CONICAL_SURFACE('',#37516,0.274750783999998,1.04719755119659);
#648=CONICAL_SURFACE('',#37522,2.80803705600002,0.785398163397436);
#649=CONICAL_SURFACE('',#37524,0.274750783999993,1.04719755119659);
#650=CONICAL_SURFACE('',#37530,2.808037056,0.785398163397464);
#651=CONICAL_SURFACE('',#37532,0.274750783999995,1.04719755119659);
#652=CONICAL_SURFACE('',#37538,2.80803705600003,0.785398163397438);
#653=CONICAL_SURFACE('',#37540,3.28958854399998,0.78539816339744);
#654=CONICAL_SURFACE('',#37547,0.322047616000123,1.04719755119657);
#655=CONICAL_SURFACE('',#37548,3.2895885439999,0.785398163397438);
#656=CONICAL_SURFACE('',#37555,0.322047615999997,1.04719755119659);
#657=CONICAL_SURFACE('',#37556,3.289588544,0.78539816339742);
#658=CONICAL_SURFACE('',#37563,0.322047616000094,1.04719755119659);
#659=CONICAL_SURFACE('',#37564,3.2895885439999,0.78539816339744);
#660=CONICAL_SURFACE('',#37571,0.32204761600005,1.04719755119655);
#661=CONICAL_SURFACE('',#37572,0.470822528000023,1.04719755119659);
#662=CONICAL_SURFACE('',#37573,0.470822528000024,1.04719755119659);
#663=CONICAL_SURFACE('',#37574,0.470822528000001,1.04719755119667);
#664=CONICAL_SURFACE('',#37575,0.470822528000002,1.04719755119667);
#665=CONICAL_SURFACE('',#37576,0.47082252800002,1.04719755119667);
#666=CONICAL_SURFACE('',#37577,0.470822528000018,1.04719755119667);
#667=CONICAL_SURFACE('',#37578,0.470822528000013,1.04719755119659);
#668=CONICAL_SURFACE('',#37579,0.470822528000016,1.04719755119659);
#669=CONICAL_SURFACE('',#37594,46.9997605328678,0.523598775598269);
#670=CONICAL_SURFACE('',#37609,17.3000533734219,0.0872664625997327);
#671=CONICAL_SURFACE('',#37610,67.117943679437,0.523598775598465);
#672=CONICAL_SURFACE('',#37615,28.921462932868,0.52359877559825);
#673=CONICAL_SURFACE('',#37618,17.3539050991947,0.0872664625997172);
#674=CONICAL_SURFACE('',#37619,17.3539050991947,0.0872664625997133);
#675=CONICAL_SURFACE('',#37623,46.9997605328686,0.523598775598271);
#676=CONICAL_SURFACE('',#37637,37.927515520559,0.523598775598339);
#677=CONICAL_SURFACE('',#37643,13.5507337588825,0.523598775598299);
#678=CONICAL_SURFACE('',#37670,3.2861910399999,0.785398163397455);
#679=CONICAL_SURFACE('',#37674,2.74142809599801,0.78539816339774);
#680=CONICAL_SURFACE('',#37681,3.28619103999997,0.78539816339744);
#681=CONICAL_SURFACE('',#37700,3.28619104000002,0.785398163397459);
#682=CONICAL_SURFACE('',#37704,2.74142809600037,0.785398163397935);
#683=CONICAL_SURFACE('',#37711,3.28619104000001,0.785398163397442);
#684=CONICAL_SURFACE('',#37715,2.74142809599998,0.78539816339744);
#685=CONICAL_SURFACE('',#37722,2.74142809599988,0.785398163397487);
#686=CONICAL_SURFACE('',#37728,37.0614901167744,0.523598775598295);
#687=CONICAL_SURFACE('',#37730,13.5507337588825,0.523598775598308);
#688=CONICAL_SURFACE('',#37752,6.37205498763392,1.04719755119592);
#689=CONICAL_SURFACE('',#37755,6.37205498762829,1.04719755119636);
#690=CONICAL_SURFACE('',#37756,6.37205498762407,1.04719755119683);
#691=CONICAL_SURFACE('',#37757,6.3720549876336,1.04719755119585);
#692=CONICAL_SURFACE('',#37758,6.3720549876249,1.04719755119687);
#693=CONICAL_SURFACE('',#37759,6.37205498762508,1.04719755119666);
#694=CONICAL_SURFACE('',#37771,6.37205498762851,1.04719755119636);
#695=CONICAL_SURFACE('',#37774,6.372054987629,1.04719755119631);
#696=CONICAL_SURFACE('',#37775,6.37205498762379,1.04719755119685);
#697=CONICAL_SURFACE('',#37776,6.37205498762845,1.04719755119638);
#698=CONICAL_SURFACE('',#37777,6.37205498762874,1.04719755119636);
#699=CONICAL_SURFACE('',#37778,6.37205498762885,1.04719755119632);
#700=CONICAL_SURFACE('',#37913,58.1057817920919,0.0174532925199245);
#701=CONICAL_SURFACE('',#37922,8.57550304943042,0.0349065850398547);
#702=CONICAL_SURFACE('',#37925,8.57550304942994,0.0349065850398894);
#703=CONICAL_SURFACE('',#37928,8.57550304942982,0.0349065850398904);
#704=CONICAL_SURFACE('',#37934,8.57550304942991,0.034906585039891);
#705=CONICAL_SURFACE('',#38071,4.98002560000028,0.785398163397452);
#706=CONICAL_SURFACE('',#38078,5.01355360000019,0.785398163397488);
#707=CONICAL_SURFACE('',#38104,20.4999999999999,0.785398163397433);
#708=CONICAL_SURFACE('',#38107,30.4999999999998,0.785398163397455);
#709=CONICAL_SURFACE('',#38115,26.0000000000003,0.785398163397453);
#710=SPHERICAL_SURFACE('',#34223,2.54);
#711=SPHERICAL_SURFACE('',#34226,2.54);
#712=SPHERICAL_SURFACE('',#34247,2.54);
#713=SPHERICAL_SURFACE('',#34253,2.54);
#714=SPHERICAL_SURFACE('',#34261,2.54);
#715=SPHERICAL_SURFACE('',#34268,2.54);
#716=SPHERICAL_SURFACE('',#34273,2.54);
#717=SPHERICAL_SURFACE('',#34278,2.54);
#718=SPHERICAL_SURFACE('',#34289,2.54);
#719=SPHERICAL_SURFACE('',#34304,2.54);
#720=SPHERICAL_SURFACE('',#34315,2.54);
#721=SPHERICAL_SURFACE('',#34321,2.54);
#722=SPHERICAL_SURFACE('',#34322,2.54);
#723=SPHERICAL_SURFACE('',#34332,2.54);
#724=SPHERICAL_SURFACE('',#34340,2.54);
#725=SPHERICAL_SURFACE('',#34343,2.54);
#726=SPHERICAL_SURFACE('',#34596,6.41240517241364);
#727=SPHERICAL_SURFACE('',#34645,6.41240517241439);
#728=SPHERICAL_SURFACE('',#34685,6.4992807017556);
#729=SPHERICAL_SURFACE('',#34700,6.49928070175542);
#730=SPHERICAL_SURFACE('',#34786,6.41240517241381);
#731=SPHERICAL_SURFACE('',#34971,5.68734575000013);
#732=SPHERICAL_SURFACE('',#34992,5.68734575000012);
#733=SPHERICAL_SURFACE('',#35068,0.499999999999998);
#734=SPHERICAL_SURFACE('',#35072,0.499999999999972);
#735=SPHERICAL_SURFACE('',#35076,0.499999999999972);
#736=SPHERICAL_SURFACE('',#35080,0.499999999999972);
#737=SPHERICAL_SURFACE('',#35084,0.499999999999998);
#738=SPHERICAL_SURFACE('',#35088,0.499999999999972);
#739=SPHERICAL_SURFACE('',#35101,0.5);
#740=SPHERICAL_SURFACE('',#35105,0.5);
#741=SPHERICAL_SURFACE('',#35112,0.499999999999998);
#742=SPHERICAL_SURFACE('',#35118,0.499999999999972);
#743=B_SPLINE_CURVE_WITH_KNOTS('',3,(#49121,#49122,#49123,#49124,#49125,
#49126,#49127,#49128,#49129),.UNSPECIFIED.,.F.,.F.,(4,1,1,1,1,1,4),(2.41610505192759E-5,
0.1666666666667,0.3333333333333,0.5,0.6666666666667,0.8333333333333,1.),
 .UNSPECIFIED.);
#744=B_SPLINE_CURVE_WITH_KNOTS('',3,(#49132,#49133,#49134,#49135,#49136,
#49137,#49138,#49139,#49140,#49141,#49142,#49143,#49144,#49145,#49146,#49147,
#49148,#49149,#49150,#49151,#49152,#49153),.UNSPECIFIED.,.F.,.F.,(4,2,2,
2,2,2,2,2,2,2,4),(0.,0.122614489199661,0.166666475605304,0.333332951210507,
0.341573133516598,0.499999426815811,0.560641811243984,0.666665902421115,
0.779351949400631,0.833332378026318,0.999998853631622),.UNSPECIFIED.);
#745=B_SPLINE_CURVE_WITH_KNOTS('',3,(#49162,#49163,#49164,#49165,#49166,
#49167,#49168,#49169,#49170),.UNSPECIFIED.,.F.,.F.,(4,1,1,1,1,1,4),(0.,
0.1666666666667,0.3333333333333,0.5,0.6666666666667,0.8333333333333,1.),
 .UNSPECIFIED.);
#746=B_SPLINE_CURVE_WITH_KNOTS('',3,(#49174,#49175,#49176,#49177,#49178,
#49179,#49180,#49181,#49182),.UNSPECIFIED.,.F.,.F.,(4,1,1,1,1,1,4),(2.85381265954449E-5,
0.1666666666667,0.3333333333333,0.5,0.6666666666667,0.8333333333333,1.),
 .UNSPECIFIED.);
#747=B_SPLINE_CURVE_WITH_KNOTS('',3,(#49186,#49187,#49188,#49189,#49190,
#49191,#49192,#49193,#49194),.UNSPECIFIED.,.F.,.F.,(4,1,1,1,1,1,4),(0.,
0.1666666666667,0.3333333333333,0.5,0.6666666666667,0.8333333333333,1.),
 .UNSPECIFIED.);
#748=B_SPLINE_CURVE_WITH_KNOTS('',3,(#49198,#49199,#49200,#49201,#49202,
#49203,#49204,#49205,#49206),.UNSPECIFIED.,.F.,.F.,(4,1,1,1,1,1,4),(2.416105051936E-5,
0.1666666666667,0.3333333333333,0.5,0.6666666666667,0.8333333333333,1.),
 .UNSPECIFIED.);
#749=B_SPLINE_CURVE_WITH_KNOTS('',3,(#49210,#49211,#49212,#49213,#49214,
#49215,#49216,#49217,#49218),.UNSPECIFIED.,.F.,.F.,(4,1,1,1,1,1,4),(0.,
0.1666666666667,0.3333333333333,0.5,0.6666666666667,0.8333333333333,1.),
 .UNSPECIFIED.);
#750=B_SPLINE_CURVE_WITH_KNOTS('',3,(#49222,#49223,#49224,#49225,#49226,
#49227,#49228,#49229,#49230),.UNSPECIFIED.,.F.,.F.,(4,1,1,1,1,1,4),(2.85380852244383E-5,
0.1666666666667,0.3333333333333,0.5,0.6666666666667,0.8333333333333,1.),
 .UNSPECIFIED.);
#751=B_SPLINE_CURVE_WITH_KNOTS('',3,(#49234,#49235,#49236,#49237,#49238,
#49239,#49240,#49241,#49242),.UNSPECIFIED.,.F.,.F.,(4,1,1,1,1,1,4),(0.,
0.1666666666667,0.3333333333333,0.5,0.6666666666667,0.8333333333333,0.999977439421937),
 .UNSPECIFIED.);
#752=B_SPLINE_CURVE_WITH_KNOTS('',3,(#49287,#49288,#49289,#49290,#49291,
#49292,#49293,#49294,#49295,#49296,#49297,#49298,#49299,#49300,#49301,#49302,
#49303,#49304,#49305,#49306,#49307,#49308,#49309,#49310,#49311,#49312,#49313,
#49314,#49315,#49316,#49317,#49318,#49319,#49320,#49321,#49322,#49323,#49324,
#49325,#49326,#49327,#49328,#49329,#49330,#49331,#49332,#49333,#49334,#49335,
#49336,#49337,#49338,#49339,#49340,#49341),.UNSPECIFIED.,.F.,.F.,(4,3,3,
3,3,3,3,3,3,3,3,3,3,3,3,3,3,3,4),(0.,0.0980466098756701,0.1428571428571,
0.235655762730469,0.2857142857143,0.360443887258383,0.4285714285714,0.5,
0.566042537085864,0.5714285714286,0.636887704333111,0.700301860505849,0.7142857142857,
0.779698786568794,0.844149904052703,0.8571428571429,0.915815433596542,0.97252549736179,
0.999999999993428),.UNSPECIFIED.);
#753=B_SPLINE_CURVE_WITH_KNOTS('',3,(#49366,#49367,#49368,#49369,#49370,
#49371,#49372,#49373,#49374,#49375),.UNSPECIFIED.,.F.,.F.,(4,1,1,1,1,1,
1,4),(0.,0.1428571428571,0.2857142857143,0.4285714285714,0.5714285714286,
0.7142857142857,0.8571428571429,1.),.UNSPECIFIED.);
#754=B_SPLINE_CURVE_WITH_KNOTS('',3,(#49379,#49380,#49381,#49382,#49383,
#49384,#49385,#49386,#49387,#49388),.UNSPECIFIED.,.F.,.F.,(4,1,1,1,1,1,
1,4),(0.,0.1428571428571,0.2857142857143,0.4285714285714,0.5714285714286,
0.7142857142857,0.8571428571429,1.),.UNSPECIFIED.);
#755=B_SPLINE_CURVE_WITH_KNOTS('',3,(#49403,#49404,#49405,#49406,#49407,
#49408,#49409,#49410,#49411,#49412),.UNSPECIFIED.,.F.,.F.,(4,1,1,1,1,1,
1,4),(0.,0.1428571428571,0.2857142857143,0.4285714285714,0.5714285714286,
0.7142857142857,0.8571428571429,1.),.UNSPECIFIED.);
#756=B_SPLINE_CURVE_WITH_KNOTS('',3,(#49415,#49416,#49417,#49418,#49419,
#49420,#49421,#49422,#49423,#49424),.UNSPECIFIED.,.F.,.F.,(4,1,1,1,1,1,
1,4),(0.,0.1428571428571,0.2857142857143,0.4285714285714,0.5714285714286,
0.7142857142857,0.8571428571429,1.),.UNSPECIFIED.);
#757=B_SPLINE_CURVE_WITH_KNOTS('',3,(#49471,#49472,#49473,#49474,#49475,
#49476,#49477,#49478,#49479,#49480,#49481,#49482,#49483,#49484,#49485,#49486,
#49487,#49488,#49489,#49490,#49491,#49492,#49493,#49494,#49495,#49496,#49497,
#49498,#49499,#49500,#49501,#49502,#49503,#49504,#49505,#49506,#49507,#49508,
#49509,#49510,#49511,#49512,#49513,#49514,#49515,#49516,#49517,#49518,#49519,
#49520,#49521,#49522,#49523,#49524,#49525,#49526,#49527,#49528,#49529,#49530,
#49531,#49532,#49533,#49534),.UNSPECIFIED.,.F.,.F.,(4,3,3,3,3,3,3,3,3,3,
3,3,3,3,3,3,3,3,3,3,3,4),(0.,0.022524348752069,0.0826907458045845,0.1428571428571,
0.183969209185199,0.24216625125188,0.2857142857143,0.344939441940217,0.408805968765505,
0.4285714285714,0.494637391748715,0.505902092667849,0.5714285714286,0.644329623937483,
0.666612808947293,0.7142857142857,0.786343515622748,0.827515831049201,0.8571428571429,
0.931638703404591,0.988736971542743,1.),.UNSPECIFIED.);
#758=B_SPLINE_CURVE_WITH_KNOTS('',3,(#49535,#49536,#49537,#49538,#49539,
#49540,#49541,#49542,#49543,#49544,#49545,#49546,#49547,#49548,#49549,#49550,
#49551,#49552,#49553,#49554,#49555,#49556,#49557,#49558,#49559,#49560,#49561,
#49562,#49563,#49564,#49565,#49566,#49567,#49568,#49569,#49570,#49571,#49572,
#49573,#49574,#49575,#49576,#49577),.UNSPECIFIED.,.F.,.F.,(4,3,3,3,3,3,
3,3,3,3,3,3,3,3,4),(0.,0.0708403169631036,0.141196221399192,0.211480985838496,
0.25,0.351421886552124,0.450884598470819,0.5,0.591484098710409,0.684303235352195,
0.75,0.824311643104987,0.900296423629433,0.978409207800814,0.999992340412632),
 .UNSPECIFIED.);
#759=B_SPLINE_CURVE_WITH_KNOTS('',3,(#49622,#49623,#49624,#49625,#49626,
#49627,#49628,#49629,#49630,#49631,#49632,#49633,#49634,#49635,#49636,#49637,
#49638,#49639,#49640,#49641,#49642,#49643),.UNSPECIFIED.,.F.,.F.,(4,2,2,
2,2,2,2,2,2,2,4),(1.17968190133454E-6,0.166667646133106,0.219922777256081,
0.333334116906424,0.439180276291458,0.500000587679843,0.658731994343029,
0.666667058453262,0.833333529226581,0.87820409141329,1.),.UNSPECIFIED.);
#760=B_SPLINE_CURVE_WITH_KNOTS('',3,(#49690,#49691,#49692,#49693,#49694,
#49695,#49696,#49697,#49698),.UNSPECIFIED.,.F.,.F.,(4,1,1,1,1,1,4),(0.,
0.1666666666667,0.3333333333333,0.5,0.6666666666667,0.8333333333333,0.999998808810884),
 .UNSPECIFIED.);
#761=B_SPLINE_CURVE_WITH_KNOTS('',3,(#49749,#49750,#49751,#49752,#49753,
#49754,#49755,#49756,#49757,#49758,#49759,#49760,#49761,#49762,#49763,#49764,
#49765,#49766,#49767,#49768,#49769,#49770,#49771,#49772,#49773,#49774,#49775,
#49776,#49777,#49778,#49779,#49780,#49781,#49782,#49783,#49784,#49785,#49786,
#49787,#49788,#49789,#49790,#49791,#49792,#49793,#49794,#49795,#49796,#49797,
#49798,#49799,#49800,#49801,#49802,#49803,#49804,#49805,#49806,#49807,#49808,
#49809,#49810,#49811,#49812),.UNSPECIFIED.,.F.,.F.,(4,3,3,3,3,3,3,3,3,3,
3,3,3,3,3,3,3,3,3,3,3,4),(0.,0.011263028288939,0.0857588259046287,0.1428571428571,
0.172484168893865,0.244542016262902,0.2857142857143,0.33338719123398,0.406288255376173,
0.4285714285714,0.49409790740126,0.560163866020983,0.5714285714286,0.635295097422919,
0.655060558117981,0.7142857142857,0.77248275702656,0.81603079085385,0.8571428571429,
0.917309254199729,0.977475651256559,1.),.UNSPECIFIED.);
#762=B_SPLINE_CURVE_WITH_KNOTS('',3,(#49861,#49862,#49863,#49864,#49865,
#49866,#49867,#49868,#49869,#49870,#49871,#49872,#49873,#49874,#49875,#49876,
#49877,#49878,#49879,#49880,#49881,#49882,#49883,#49884,#49885,#49886,#49887,
#49888,#49889,#49890,#49891,#49892,#49893,#49894,#49895,#49896,#49897,#49898,
#49899,#49900,#49901,#49902,#49903,#49904,#49905,#49906,#49907,#49908,#49909,
#49910,#49911,#49912,#49913,#49914,#49915,#49916,#49917,#49918,#49919,#49920,
#49921,#49922,#49923,#49924),.UNSPECIFIED.,.F.,.F.,(4,3,3,3,3,3,3,3,3,3,
3,3,3,3,3,3,3,3,3,3,3,4),(0.,0.022524348752069,0.0826907458045845,0.1428571428571,
0.183969209185192,0.242166251253732,0.2857142857143,0.34493944194013,0.408805968765661,
0.4285714285714,0.494637391744036,0.505902092667695,0.5714285714286,0.644329623939086,
0.666612808947312,0.7142857142857,0.786343515622548,0.827515831048836,0.8571428571429,
0.931638703405425,0.988736971542787,1.),.UNSPECIFIED.);
#763=B_SPLINE_CURVE_WITH_KNOTS('',3,(#49925,#49926,#49927,#49928,#49929,
#49930,#49931,#49932,#49933,#49934,#49935,#49936,#49937,#49938,#49939,#49940,
#49941,#49942,#49943,#49944,#49945,#49946,#49947,#49948,#49949,#49950,#49951,
#49952,#49953,#49954,#49955,#49956,#49957,#49958,#49959,#49960,#49961,#49962,
#49963,#49964,#49965,#49966,#49967),.UNSPECIFIED.,.F.,.F.,(4,3,3,3,3,3,
3,3,3,3,3,3,3,3,4),(0.,0.0708403169625752,0.141196221398188,0.211480985837894,
0.25,0.351421886557641,0.45088459847787,0.5,0.591484098711512,0.684303235350053,
0.75,0.824311643104386,0.900296423628743,0.978409207797605,0.999992340412643),
 .UNSPECIFIED.);
#764=B_SPLINE_CURVE_WITH_KNOTS('',3,(#50011,#50012,#50013,#50014,#50015,
#50016,#50017,#50018,#50019),.UNSPECIFIED.,.F.,.F.,(4,1,1,1,1,1,4),(1.12301924736311E-6,
0.1666666666667,0.3333333333333,0.5,0.6666666666667,0.8333333333333,1.),
 .UNSPECIFIED.);
#765=B_SPLINE_CURVE_WITH_KNOTS('',3,(#50069,#50070,#50071,#50072,#50073,
#50074,#50075,#50076,#50077,#50078,#50079,#50080,#50081,#50082,#50083,#50084,
#50085,#50086,#50087,#50088,#50089,#50090),.UNSPECIFIED.,.F.,.F.,(4,2,2,
2,2,2,2,2,2,2,4),(1.17968190350786E-6,0.166667646133105,0.219922777256189,
0.333334116906424,0.439180276291488,0.500000587679843,0.658731994343154,
0.666667058453262,0.833333529226581,0.878204091413217,1.),.UNSPECIFIED.);
#766=B_SPLINE_CURVE_WITH_KNOTS('',3,(#50099,#50100,#50101,#50102,#50103,
#50104,#50105,#50106,#50107,#50108,#50109,#50110,#50111,#50112,#50113,#50114,
#50115,#50116,#50117,#50118,#50119,#50120,#50121,#50122,#50123,#50124,#50125,
#50126,#50127,#50128,#50129,#50130,#50131,#50132,#50133,#50134,#50135,#50136,
#50137,#50138,#50139,#50140,#50141,#50142,#50143,#50144,#50145,#50146,#50147,
#50148,#50149,#50150,#50151,#50152,#50153),.UNSPECIFIED.,.F.,.F.,(4,3,3,
3,3,3,3,3,3,3,3,3,3,3,3,3,3,3,4),(0.,0.0565152922712344,0.114965932003303,
0.1428571428571,0.207266907155971,0.272629548288784,0.2857142857143,0.349038397788053,
0.414377828143602,0.4285714285714,0.494613972575815,0.562439737569692,0.5714285714286,
0.646158146057277,0.7142857142857,0.807084236549117,0.8571428571429,0.955189540194312,
1.),.UNSPECIFIED.);
#767=B_SPLINE_CURVE_WITH_KNOTS('',3,(#50200,#50201,#50202,#50203,#50204,
#50205,#50206,#50207,#50208,#50209,#50210,#50211,#50212,#50213,#50214,#50215,
#50216,#50217,#50218,#50219,#50220,#50221,#50222,#50223,#50224,#50225,#50226,
#50227,#50228,#50229,#50230,#50231,#50232,#50233,#50234,#50235,#50236,#50237,
#50238,#50239,#50240,#50241,#50242),.UNSPECIFIED.,.F.,.F.,(4,3,3,3,3,3,
3,3,3,3,3,3,3,3,4),(0.,0.0708403169627012,0.141196221397882,0.211480985835855,
0.25,0.351421886559069,0.450884598479571,0.5,0.591484098710457,0.684303235349992,
0.75,0.824311643105781,0.900296423630328,0.97840920780083,0.999992340411847),
 .UNSPECIFIED.);
#768=B_SPLINE_CURVE_WITH_KNOTS('',3,(#50244,#50245,#50246,#50247,#50248,
#50249,#50250,#50251,#50252,#50253),.UNSPECIFIED.,.F.,.F.,(4,1,1,1,1,1,
1,4),(0.,0.1428571428571,0.2857142857143,0.4285714285714,0.5714285714286,
0.7142857142857,0.8571428571429,1.),.UNSPECIFIED.);
#769=B_SPLINE_CURVE_WITH_KNOTS('',3,(#50260,#50261,#50262,#50263,#50264,
#50265,#50266,#50267,#50268,#50269),.UNSPECIFIED.,.F.,.F.,(4,1,1,1,1,1,
1,4),(0.,0.1428571428571,0.2857142857143,0.4285714285714,0.5714285714286,
0.7142857142857,0.8571428571429,1.),.UNSPECIFIED.);
#770=B_SPLINE_CURVE_WITH_KNOTS('',3,(#50286,#50287,#50288,#50289,#50290,
#50291,#50292,#50293,#50294,#50295),.UNSPECIFIED.,.F.,.F.,(4,1,1,1,1,1,
1,4),(0.,0.1428571428571,0.2857142857143,0.4285714285714,0.5714285714286,
0.7142857142857,0.8571428571429,1.),.UNSPECIFIED.);
#771=B_SPLINE_CURVE_WITH_KNOTS('',3,(#50299,#50300,#50301,#50302,#50303,
#50304,#50305,#50306,#50307,#50308),.UNSPECIFIED.,.F.,.F.,(4,1,1,1,1,1,
1,4),(0.,0.1428571428571,0.2857142857143,0.4285714285714,0.5714285714286,
0.7142857142857,0.8571428571429,1.),.UNSPECIFIED.);
#772=B_SPLINE_CURVE_WITH_KNOTS('',3,(#50318,#50319,#50320,#50321,#50322,
#50323,#50324,#50325,#50326),.UNSPECIFIED.,.F.,.F.,(4,1,1,1,1,1,4),(1.1230192517404E-6,
0.1666666666667,0.3333333333333,0.5,0.6666666666667,0.8333333333333,1.),
 .UNSPECIFIED.);
#773=B_SPLINE_CURVE_WITH_KNOTS('',3,(#50406,#50407,#50408,#50409,#50410,
#50411,#50412,#50413,#50414,#50415,#50416,#50417,#50418,#50419,#50420,#50421,
#50422,#50423,#50424,#50425,#50426,#50427),.UNSPECIFIED.,.F.,.F.,(4,2,2,
2,2,2,2,2,2,2,4),(0.,0.122614489199695,0.166666475605304,0.333332951210509,
0.341573133516643,0.499999426815813,0.560641811244011,0.666665902421118,
0.779351949400641,0.833332378026322,0.999998853631626),.UNSPECIFIED.);
#774=B_SPLINE_CURVE_WITH_KNOTS('',3,(#50478,#50479,#50480,#50481,#50482,
#50483,#50484,#50485,#50486,#50487,#50488,#50489,#50490,#50491,#50492,#50493,
#50494,#50495,#50496,#50497,#50498,#50499,#50500,#50501,#50502,#50503,#50504,
#50505,#50506,#50507,#50508,#50509,#50510,#50511,#50512,#50513,#50514,#50515,
#50516,#50517,#50518,#50519,#50520,#50521,#50522,#50523,#50524,#50525,#50526,
#50527,#50528,#50529,#50530,#50531,#50532,#50533,#50534,#50535,#50536,#50537,
#50538,#50539,#50540,#50541),.UNSPECIFIED.,.F.,.F.,(4,3,3,3,3,3,3,3,3,3,
3,3,3,3,3,3,3,3,3,3,3,4),(0.,0.0112630282889006,0.0857588259025268,0.142857142855473,
0.172484168891931,0.244542016261801,0.285714285711046,0.333387191230076,
0.406288255372341,0.428571428566519,0.49409790739575,0.560163866013515,
0.571428571422092,0.635295097422519,0.655060558110842,0.714285714277565,
0.772482757008491,0.816030790845477,0.857142857133138,0.917309254189421,
0.977475651245705,0.999999999988612),.UNSPECIFIED.);
#775=B_SPLINE_CURVE_WITH_KNOTS('',3,(#50551,#50552,#50553,#50554,#50555,
#50556,#50557,#50558,#50559,#50560,#50561,#50562,#50563,#50564,#50565,#50566,
#50567,#50568,#50569,#50570,#50571,#50572,#50573,#50574,#50575,#50576,#50577,
#50578,#50579,#50580,#50581,#50582,#50583,#50584,#50585,#50586,#50587,#50588,
#50589,#50590,#50591,#50592,#50593,#50594,#50595,#50596,#50597,#50598,#50599,
#50600,#50601,#50602,#50603,#50604,#50605),.UNSPECIFIED.,.F.,.F.,(4,3,3,
3,3,3,3,3,3,3,3,3,3,3,3,3,3,3,4),(0.,0.0565152922717072,0.114965932004273,
0.1428571428571,0.207266907154939,0.272629548286749,0.2857142857143,0.349038397790888,
0.414377828149668,0.4285714285714,0.494613972566219,0.562439737549771,0.5714285714286,
0.64615814615571,0.7142857142857,0.807084237689468,0.8571428571429,0.955189538087307,
1.),.UNSPECIFIED.);
#776=B_SPLINE_CURVE_WITH_KNOTS('',3,(#50699,#50700,#50701,#50702,#50703,
#50704,#50705,#50706,#50707,#50708,#50709,#50710,#50711,#50712,#50713,#50714,
#50715,#50716,#50717,#50718,#50719,#50720,#50721,#50722,#50723,#50724,#50725,
#50726,#50727,#50728,#50729,#50730,#50731,#50732,#50733,#50734,#50735,#50736,
#50737,#50738,#50739,#50740,#50741,#50742,#50743,#50744,#50745,#50746,#50747,
#50748,#50749,#50750,#50751,#50752,#50753,#50754,#50755,#50756,#50757,#50758,
#50759,#50760,#50761,#50762),.UNSPECIFIED.,.F.,.F.,(4,3,3,3,3,3,3,3,3,3,
3,3,3,3,3,3,3,3,3,3,3,4),(0.,0.011263028289029,0.0857588259024072,0.1428571428571,
0.172484168893897,0.244542016269632,0.2857142857143,0.333387191233873,0.406288255371836,
0.4285714285714,0.494097907401377,0.560163866020033,0.5714285714286,0.63529509742806,
0.655060558118314,0.7142857142857,0.772482757018248,0.816030790854834,0.8571428571429,
0.917309254199805,0.97747565125671,0.999999999999998),.UNSPECIFIED.);
#777=B_SPLINE_CURVE_WITH_KNOTS('',3,(#50807,#50808,#50809,#50810,#50811,
#50812,#50813,#50814,#50815),.UNSPECIFIED.,.F.,.F.,(4,1,1,1,1,1,4),(0.,
0.1666666666667,0.3333333333333,0.5,0.6666666666667,0.8333333333333,0.999998808810887),
 .UNSPECIFIED.);
#778=B_SPLINE_CURVE_WITH_KNOTS('',3,(#51594,#51595,#51596,#51597),
 .UNSPECIFIED.,.F.,.F.,(4,4),(3.08084590110894,3.12989709501739),
 .UNSPECIFIED.);
#779=B_SPLINE_CURVE_WITH_KNOTS('',3,(#51606,#51607,#51608,#51609),
 .UNSPECIFIED.,.F.,.F.,(4,4),(3.03179470720155,3.08084590110894),
 .UNSPECIFIED.);
#780=B_SPLINE_CURVE_WITH_KNOTS('',3,(#51611,#51612,#51613,#51614,#51615,
#51616,#51617,#51618),.UNSPECIFIED.,.F.,.F.,(4,2,2,4),(-0.281543316074503,
-0.256347073285161,-0.128173536642581,-0.0492557161192092),
 .UNSPECIFIED.);
#781=B_SPLINE_CURVE_WITH_KNOTS('',3,(#51620,#51621,#51622,#51623,#51624,
#51625,#51626,#51627),.UNSPECIFIED.,.F.,.F.,(4,2,2,4),(-3.44463382971284,
-3.36571600918869,-3.23754247254589,-3.21234622975666),.UNSPECIFIED.);
#782=B_SPLINE_CURVE_WITH_KNOTS('',3,(#51629,#51630,#51631,#51632,#51633,
#51634,#51635),.UNSPECIFIED.,.F.,.F.,(4,3,4),(-0.0490511939078948,0.,0.0490511939079084),
 .UNSPECIFIED.);
#783=B_SPLINE_CURVE_WITH_KNOTS('',3,(#51637,#51638,#51639,#51640,#51641,
#51642,#51643,#51644),.UNSPECIFIED.,.F.,.F.,(4,2,2,4),(-0.281543316073918,
-0.256347073285632,-0.128173536642816,-0.0492557161186468),
 .UNSPECIFIED.);
#784=B_SPLINE_CURVE_WITH_KNOTS('',3,(#51646,#51647,#51648,#51649,#51650,
#51651,#51652,#51653),.UNSPECIFIED.,.F.,.F.,(4,2,2,4),(-3.44463382971226,
-3.36571600918894,-3.23754247254636,-3.21234622975697),.UNSPECIFIED.);
#785=B_SPLINE_CURVE_WITH_KNOTS('',3,(#51655,#51656,#51657,#51658,#51659,
#51660,#51661),.UNSPECIFIED.,.F.,.F.,(4,3,4),(-0.0490511939073931,0.,0.0490511939084528),
 .UNSPECIFIED.);
#786=B_SPLINE_CURVE_WITH_KNOTS('',3,(#51663,#51664,#51665,#51666,#51667,
#51668,#51669,#51670),.UNSPECIFIED.,.F.,.F.,(4,2,2,4),(-0.281543316074568,
-0.256347073286048,-0.128173536643024,-0.0492557161192777),
 .UNSPECIFIED.);
#787=B_SPLINE_CURVE_WITH_KNOTS('',3,(#51672,#51673,#51674,#51675,#51676,
#51677,#51678,#51679),.UNSPECIFIED.,.F.,.F.,(4,2,2,4),(-3.44463382971165,
-3.36571600918866,-3.23754247254584,-3.21234622975546),.UNSPECIFIED.);
#788=B_SPLINE_CURVE_WITH_KNOTS('',3,(#51681,#51682,#51683,#51684,#51685,
#51686,#51687),.UNSPECIFIED.,.F.,.F.,(4,3,4),(-0.0490511939080049,0.,0.0490511939079151),
 .UNSPECIFIED.);
#789=B_SPLINE_CURVE_WITH_KNOTS('',3,(#51689,#51690,#51691,#51692,#51693,
#51694,#51695,#51696),.UNSPECIFIED.,.F.,.F.,(4,2,2,4),(-0.281543316075136,
-0.25634707328559,-0.128173536642795,-0.049255716119827),.UNSPECIFIED.);
#790=B_SPLINE_CURVE_WITH_KNOTS('',3,(#51697,#51698,#51699,#51700,#51701,
#51702,#51703,#51704),.UNSPECIFIED.,.F.,.F.,(4,2,2,4),(-3.44463382971222,
-3.36571600918842,-3.23754247254539,-3.21234622975693),.UNSPECIFIED.);
#791=B_SPLINE_CURVE_WITH_KNOTS('',3,(#51727,#51728,#51729,#51730,#51731,
#51732,#51733,#51734,#51735,#51736),.UNSPECIFIED.,.F.,.F.,(4,2,2,2,4),(-1.23367624376484,
-1.07962569003998,-0.925575136315127,-0.771400514278829,-0.617225892242532),
 .UNSPECIFIED.);
#792=B_SPLINE_CURVE_WITH_KNOTS('',3,(#51737,#51738,#51739,#51740,#51741,
#51742,#51743,#51744,#51745,#51746),.UNSPECIFIED.,.F.,.F.,(4,2,2,2,4),(-1.85012659645245,
-1.69593736206289,-1.54174812767333,-1.38771218571909,-1.23367624376484),
 .UNSPECIFIED.);
#793=B_SPLINE_CURVE_WITH_KNOTS('',3,(#51752,#51753,#51754,#51755,#51756,
#51757,#51758,#51759,#51760,#51761),.UNSPECIFIED.,.F.,.F.,(4,2,2,2,4),(2.30953959739069,
2.51054404549657,2.71154849360245,2.89942800416522,3.08730751472799),
 .UNSPECIFIED.);
#794=B_SPLINE_CURVE_WITH_KNOTS('',3,(#51767,#51768,#51769,#51770,#51771,
#51772,#51773,#51774,#51775,#51776,#51777,#51778,#51779,#51780,#51781,#51782,
#51783,#51784),.UNSPECIFIED.,.F.,.F.,(4,2,2,2,2,2,2,2,4),(0.368633646558617,
0.466000906670528,0.563368166782438,0.648915734055293,0.734463301328148,
0.820010868601003,0.905558435873858,1.00292569598577,1.10029295609768),
 .UNSPECIFIED.);
#795=B_SPLINE_CURVE_WITH_KNOTS('',3,(#51790,#51791,#51792,#51793,#51794,
#51795,#51796,#51797,#51798,#51799),.UNSPECIFIED.,.F.,.F.,(4,2,2,2,4),(-1.77635683940028E-15,
0.181238959345487,0.362477918690977,0.570076776395974,0.777675634100972),
 .UNSPECIFIED.);
#796=B_SPLINE_CURVE_WITH_KNOTS('',3,(#51805,#51806,#51807,#51808,#51809,
#51810,#51811,#51812,#51813,#51814),.UNSPECIFIED.,.F.,.F.,(4,2,2,2,4),(0.617225892242314,
0.771400514278674,0.925575136315034,1.07962569003995,1.23367624376487),
 .UNSPECIFIED.);
#797=B_SPLINE_CURVE_WITH_KNOTS('',3,(#51817,#51818,#51819,#51820,#51821,
#51822,#51823,#51824,#51825,#51826),.UNSPECIFIED.,.F.,.F.,(4,2,2,2,4),(1.23367624376487,
1.38771218571906,1.54174812767325,1.69593736206276,1.85012659645227),
 .UNSPECIFIED.);
#798=B_SPLINE_CURVE_WITH_KNOTS('',3,(#51832,#51833,#51834,#51835,#51836,
#51837,#51838,#51839,#51840,#51841,#51842,#51843,#51844,#51845,#51846,#51847,
#51848,#51849,#51850),.UNSPECIFIED.,.F.,.F.,(4,2,2,2,3,2,2,2,4),(-0.366794796562496,
-0.268922616838031,-0.171050437113567,-0.0855252185567822,2.33146835171283E-15,
0.0855252185567869,0.171050437113571,0.268922616838036,0.366794796562501),
 .UNSPECIFIED.);
#799=B_SPLINE_CURVE_WITH_KNOTS('',3,(#51854,#51855,#51856,#51857,#51858,
#51859,#51860,#51861,#51862,#51863,#51864,#51865,#51866,#51867,#51868,#51869,
#51870,#51871,#51872),.UNSPECIFIED.,.F.,.F.,(4,2,2,2,3,2,2,2,4),(-0.365829654769541,
-0.268462394657629,-0.171095134545717,-0.0855475672728611,-5.21804821573824E-15,
0.0882774493987044,0.176554898797414,0.271203483898993,0.365852069000572),
 .UNSPECIFIED.);
#800=B_SPLINE_CURVE_WITH_KNOTS('',3,(#51876,#51877,#51878,#51879,#51880,
#51881,#51882,#51883,#51884,#51885,#51886,#51887,#51888,#51889,#51890,#51891,
#51892,#51893),.UNSPECIFIED.,.F.,.F.,(4,2,2,2,2,2,2,2,4),(-1.10334360967883,
-1.00547142995437,-0.907599250229903,-0.822074031673119,-0.736548813116335,
-0.651023594559552,-0.565498376002768,-0.467626196278304,-0.369754016553839),
 .UNSPECIFIED.);
#801=B_SPLINE_CURVE_WITH_KNOTS('',3,(#51900,#51901,#51902,#51903,#51904,
#51905,#51906,#51907,#51908,#51909),.UNSPECIFIED.,.F.,.F.,(4,2,2,2,4),(0.,
0.181230618131972,0.362461236263944,0.571238472910728,0.780015709557511),
 .UNSPECIFIED.);
#802=B_SPLINE_CURVE_WITH_KNOTS('',3,(#51912,#51913,#51914,#51915,#51916,
#51917,#51918,#51919,#51920,#51921),.UNSPECIFIED.,.F.,.F.,(4,2,2,2,4),(-2.32129720255586,
-2.11369834485087,-1.90609948714587,-1.72486052780038,-1.54362156845489),
 .UNSPECIFIED.);
#803=B_SPLINE_CURVE_WITH_KNOTS('',3,(#51939,#51940,#51941,#51942,#51943,
#51944,#51945,#51946,#51947,#51948),.UNSPECIFIED.,.F.,.F.,(4,2,2,2,4),(-1.85012659645253,
-1.69593736206296,-1.54174812767339,-1.38771218571914,-1.23367624376489),
 .UNSPECIFIED.);
#804=B_SPLINE_CURVE_WITH_KNOTS('',3,(#51952,#51953,#51954,#51955,#51956,
#51957,#51958,#51959,#51960,#51961),.UNSPECIFIED.,.F.,.F.,(4,2,2,2,4),(-1.23367624376489,
-1.07962569004007,-0.925575136315257,-0.771400514279,-0.617225892242743),
 .UNSPECIFIED.);
#805=B_SPLINE_CURVE_WITH_KNOTS('',3,(#51971,#51972,#51973,#51974,#51975,
#51976,#51977,#51978,#51979,#51980),.UNSPECIFIED.,.F.,.F.,(4,2,2,2,4),(1.54359366303678,
1.73147317359955,1.91935268416232,2.1203571322682,2.32136158037408),
 .UNSPECIFIED.);
#806=B_SPLINE_CURVE_WITH_KNOTS('',3,(#51989,#51990,#51991,#51992,#51993,
#51994,#51995,#51996,#51997,#51998),.UNSPECIFIED.,.F.,.F.,(4,2,2,2,4),(1.23367624376487,
1.38771218571901,1.54174812767315,1.69593736206261,1.85012659645207),
 .UNSPECIFIED.);
#807=B_SPLINE_CURVE_WITH_KNOTS('',3,(#51999,#52000,#52001,#52002,#52003,
#52004,#52005,#52006,#52007,#52008),.UNSPECIFIED.,.F.,.F.,(4,2,2,2,4),(0.617225892242314,
0.771400514278675,0.925575136315035,1.07962569003995,1.23367624376487),
 .UNSPECIFIED.);
#808=B_SPLINE_CURVE_WITH_KNOTS('',3,(#52138,#52139,#52140,#52141,#52142,
#52143,#52144,#52145,#52146,#52147),.UNSPECIFIED.,.F.,.F.,(4,2,2,2,4),(1.54763785217733,
1.73581526281001,1.92399267344269,2.12587396957551,2.32775526570834),
 .UNSPECIFIED.);
#809=B_SPLINE_CURVE_WITH_KNOTS('',3,(#52454,#52455,#52456,#52457,#52458,
#52459,#52460,#52461,#52462,#52463),.UNSPECIFIED.,.F.,.F.,(4,2,2,2,4),(0.767622142619809,
0.976399379266592,1.18517661591337,1.36640723404535,1.54763785217732),
 .UNSPECIFIED.);
#810=B_SPLINE_CURVE_WITH_KNOTS('',3,(#52478,#52479,#52480,#52481,#52482,
#52483,#52484,#52485,#52486,#52487),.UNSPECIFIED.,.F.,.F.,(4,2,2,2,4),(2.31525999479713,
2.52403723144391,2.73281446809069,2.91404508622267,3.09527570435464),
 .UNSPECIFIED.);
#811=B_SPLINE_CURVE_WITH_KNOTS('',3,(#52630,#52631,#52632,#52633,#52634,
#52635,#52636,#52637,#52638,#52639,#52640,#52641,#52642,#52643,#52644,#52645,
#52646,#52647),.UNSPECIFIED.,.F.,.F.,(4,2,2,2,2,2,2,2,4),(-1.24400278846932,
-1.08850242875974,-0.933002069050166,-0.777501731642414,-0.622001394234663,
-0.46650105682691,-0.311000719419158,-0.155500359709579,0.),
 .UNSPECIFIED.);
#812=B_SPLINE_CURVE_WITH_KNOTS('',3,(#52653,#52654,#52655,#52656,#52657,
#52658,#52659,#52660,#52661,#52662,#52663,#52664,#52665,#52666,#52667,#52668,
#52669,#52670),.UNSPECIFIED.,.F.,.F.,(4,2,2,2,2,2,2,2,4),(0.,0.155500359709579,
0.311000719419159,0.46650105682691,0.622001394234662,0.777501731642413,
0.933002069050164,1.08850242875974,1.24400278846933),.UNSPECIFIED.);
#813=B_SPLINE_CURVE_WITH_KNOTS('',3,(#52679,#52680,#52681,#52682,#52683,
#52684,#52685,#52686,#52687,#52688,#52689,#52690,#52691,#52692,#52693,#52694,
#52695,#52696),.UNSPECIFIED.,.F.,.F.,(4,2,2,2,2,2,2,2,4),(-1.24400278846934,
-1.08850242875976,-0.933002069050176,-0.777501731642423,-0.622001394234669,
-0.466501056826915,-0.311000719419162,-0.155500359709581,0.),
 .UNSPECIFIED.);
#814=B_SPLINE_CURVE_WITH_KNOTS('',3,(#52702,#52703,#52704,#52705,#52706,
#52707,#52708,#52709,#52710,#52711,#52712,#52713,#52714,#52715,#52716,#52717,
#52718,#52719),.UNSPECIFIED.,.F.,.F.,(4,2,2,2,2,2,2,2,4),(0.,0.155500359709582,
0.311000719419163,0.466501056826916,0.622001394234669,0.777501731642423,
0.933002069050176,1.08850242875976,1.24400278846934),.UNSPECIFIED.);
#815=B_SPLINE_CURVE_WITH_KNOTS('',3,(#52734,#52735,#52736,#52737,#52738,
#52739,#52740,#52741,#52742,#52743,#52744,#52745,#52746,#52747,#52748,#52749,
#52750,#52751),.UNSPECIFIED.,.F.,.F.,(4,2,2,2,2,2,2,2,4),(-1.24400278846932,
-1.08850242875974,-0.933002069050164,-0.777501731642413,-0.622001394234661,
-0.46650105682691,-0.311000719419158,-0.155500359709579,0.),
 .UNSPECIFIED.);
#816=B_SPLINE_CURVE_WITH_KNOTS('',3,(#52755,#52756,#52757,#52758,#52759,
#52760,#52761,#52762,#52763,#52764,#52765,#52766,#52767,#52768,#52769,#52770,
#52771,#52772),.UNSPECIFIED.,.F.,.F.,(4,2,2,2,2,2,2,2,4),(0.,0.15550035970958,
0.311000719419159,0.466501056826911,0.622001394234662,0.777501731642413,
0.933002069050165,1.08850242875974,1.24400278846932),.UNSPECIFIED.);
#817=B_SPLINE_CURVE_WITH_KNOTS('',3,(#53461,#53462,#53463,#53464,#53465,
#53466,#53467,#53468,#53469,#53470),.UNSPECIFIED.,.F.,.F.,(4,2,2,2,4),(0.,
0.0127647979976817,0.0210777909778716,0.0238357493132096,0.025921076707915),
 .UNSPECIFIED.);
#818=B_SPLINE_CURVE_WITH_KNOTS('',3,(#53489,#53490,#53491,#53492,#53493,
#53494,#53495,#53496,#53497,#53498),.UNSPECIFIED.,.F.,.F.,(4,2,2,2,4),(0.,
0.00150625431059664,0.00349900031797075,0.00979302012528766,0.0186876936860384),
 .UNSPECIFIED.);
#819=B_SPLINE_CURVE_WITH_KNOTS('',3,(#55896,#55897,#55898,#55899,#55900,
#55901,#55902,#55903,#55904,#55905),.UNSPECIFIED.,.F.,.F.,(4,2,2,2,4),(0.910129823137503,
1.1376283823127,1.36512694148791,1.59269329388146,1.82025964627501),
 .UNSPECIFIED.);
#820=B_SPLINE_CURVE_WITH_KNOTS('',3,(#55909,#55910,#55911,#55912,#55913,
#55914,#55915,#55916,#55917,#55918),.UNSPECIFIED.,.F.,.F.,(4,2,2,2,4),(1.82025964627501,
2.04782599866856,2.27539235106211,2.50289091023731,2.73038946941251),
 .UNSPECIFIED.);
#821=B_SPLINE_CURVE_WITH_KNOTS('',3,(#55923,#55924,#55925,#55926,#55927,
#55928,#55929,#55930,#55931,#55932,#55933,#55934,#55935,#55936,#55937,#55938,
#55939,#55940),.UNSPECIFIED.,.F.,.F.,(4,2,2,2,2,2,2,2,4),(0.,0.22893459915159,
0.45786919830318,0.68657220048275,0.91527520266232,1.14397820484189,1.37268120702146,
1.60161580617305,1.83055040532464),.UNSPECIFIED.);
#822=B_SPLINE_CURVE_WITH_KNOTS('',3,(#55959,#55960,#55961,#55962,#55963,
#55964,#55965,#55966,#55967,#55968,#55969,#55970,#55971,#55972,#55973,#55974,
#55975,#55976),.UNSPECIFIED.,.F.,.F.,(4,2,2,2,2,2,2,2,4),(-3.6611008106493,
-3.4321662114977,-3.20323161234611,-2.97452861016654,-2.74582560798697,
-2.5171226058074,-2.28841960362783,-2.05948500447624,-1.83055040532465),
 .UNSPECIFIED.);
#823=B_SPLINE_CURVE_WITH_KNOTS('',3,(#56047,#56048,#56049,#56050,#56051,
#56052,#56053,#56054,#56055,#56056),.UNSPECIFIED.,.F.,.F.,(4,2,2,2,4),(2.73038946941251,
2.95788802858771,3.18538658776291,3.41295294015646,3.64051929255001),
 .UNSPECIFIED.);
#824=B_SPLINE_CURVE_WITH_KNOTS('',3,(#56068,#56069,#56070,#56071,#56072,
#56073,#56074,#56075,#56076,#56077),.UNSPECIFIED.,.F.,.F.,(4,2,2,2,4),(0.,
0.22756635239355,0.4551327047871,0.682631263962301,0.910129823137503),
 .UNSPECIFIED.);
#825=B_SPLINE_CURVE_WITH_KNOTS('',3,(#56114,#56115,#56116,#56117,#56118,
#56119,#56120,#56121,#56122,#56123),.UNSPECIFIED.,.F.,.F.,(4,2,2,2,4),(0.910129823137503,
1.1376283823127,1.36512694148791,1.59269329388146,1.82025964627501),
 .UNSPECIFIED.);
#826=B_SPLINE_CURVE_WITH_KNOTS('',3,(#56127,#56128,#56129,#56130,#56131,
#56132,#56133,#56134,#56135,#56136),.UNSPECIFIED.,.F.,.F.,(4,2,2,2,4),(1.82025964627501,
2.04782599866856,2.27539235106211,2.50289091023731,2.73038946941251),
 .UNSPECIFIED.);
#827=B_SPLINE_CURVE_WITH_KNOTS('',3,(#56154,#56155,#56156,#56157,#56158,
#56159,#56160,#56161,#56162,#56163,#56164,#56165,#56166,#56167,#56168,#56169,
#56170,#56171),.UNSPECIFIED.,.F.,.F.,(4,2,2,2,2,2,2,2,4),(-1.84177286144596,
-1.6112902776922,-1.38080769393844,-1.15084706233071,-0.920886430722982,
-0.690925799115252,-0.460965167507522,-0.230482583753761,0.),
 .UNSPECIFIED.);
#828=B_SPLINE_CURVE_WITH_KNOTS('',3,(#56174,#56175,#56176,#56177,#56178,
#56179,#56180,#56181,#56182,#56183,#56184,#56185,#56186,#56187,#56188,#56189,
#56190,#56191),.UNSPECIFIED.,.F.,.F.,(4,2,2,2,2,2,2,2,4),(-3.68354572289192,
-3.45306313913815,-3.22258055538439,-2.99261992377667,-2.76265929216894,
-2.53269866056121,-2.30273802895348,-2.07225544519972,-1.84177286144596),
 .UNSPECIFIED.);
#829=B_SPLINE_CURVE_WITH_KNOTS('',3,(#56285,#56286,#56287,#56288,#56289,
#56290,#56291,#56292,#56293,#56294),.UNSPECIFIED.,.F.,.F.,(4,2,2,2,4),(2.73038946941251,
2.95788802858771,3.18538658776291,3.41295294015646,3.64051929255001),
 .UNSPECIFIED.);
#830=B_SPLINE_CURVE_WITH_KNOTS('',3,(#56306,#56307,#56308,#56309,#56310,
#56311,#56312,#56313,#56314,#56315),.UNSPECIFIED.,.F.,.F.,(4,2,2,2,4),(0.,
0.22756635239355,0.4551327047871,0.682631263962301,0.910129823137503),
 .UNSPECIFIED.);
#831=B_SPLINE_CURVE_WITH_KNOTS('',3,(#59743,#59744,#59745,#59746,#59747,
#59748,#59749,#59750),.UNSPECIFIED.,.F.,.F.,(4,2,2,4),(-6.50854151614474,
-6.00862181551197,-5.43826767053468,-4.86791352555738),.UNSPECIFIED.);
#832=B_SPLINE_CURVE_WITH_KNOTS('',3,(#59752,#59753,#59754,#59755,#59756,
#59757,#59758,#59759,#59760,#59761,#59762,#59763,#59764,#59765,#59766,#59767,
#59768,#59769,#59770,#59771,#59772,#59773,#59774,#59775,#59776,#59777),
 .UNSPECIFIED.,.F.,.F.,(4,2,2,2,2,2,2,2,2,2,2,2,4),(6.50854151613977,6.57897596048927,
7.14933010546656,7.72311029238147,8.29689047929639,8.8706706662113,9.44445085312622,
10.0182310400411,10.592011226956,11.165791413871,11.7395716007859,12.3099257457632,
12.3803601901077),.UNSPECIFIED.);
#833=B_SPLINE_CURVE_WITH_KNOTS('',3,(#59778,#59779,#59780,#59781,#59782,
#59783,#59784,#59785,#59786,#59787,#59788,#59789,#59790,#59791,#59792,#59793,
#59794,#59795,#59796,#59797,#59798,#59799,#59800,#59801,#59802,#59803,#59804,
#59805,#59806,#59807,#59808,#59809,#59810,#59811,#59812,#59813,#59814,#59815,
#59816,#59817,#59818),.UNSPECIFIED.,.F.,.F.,(4,2,2,2,2,2,2,2,3,2,2,2,2,
2,2,2,2,2,2,4),(-4.86791352555738,-4.23909906011465,-3.61028459467191,-2.98147012922918,
-2.35265566378644,-1.76449174783983,-1.17632783189322,-0.588163915946611,
0.,0.588163915946613,1.17632783189323,1.76449174783983,2.35265566378645,
2.98147012922918,3.61028459467192,4.23909906011465,4.86791352555738,5.43826767053468,
6.00862181551197,6.50854151613977),.UNSPECIFIED.);
#834=B_SPLINE_CURVE_WITH_KNOTS('',3,(#59904,#59905,#59906,#59907),
 .UNSPECIFIED.,.F.,.F.,(4,4),(0.0184096978210032,0.021955582065653),
 .UNSPECIFIED.);
#835=B_SPLINE_CURVE_WITH_KNOTS('',3,(#59908,#59909,#59910,#59911),
 .UNSPECIFIED.,.F.,.F.,(4,4),(0.0186156132125293,0.0221618161533776),
 .UNSPECIFIED.);
#836=B_SPLINE_CURVE_WITH_KNOTS('',3,(#59922,#59923,#59924,#59925,#59926,
#59927,#59928,#59929,#59930,#59931,#59932,#59933,#59934,#59935,#59936,#59937,
#59938,#59939,#59940,#59941,#59942,#59943,#59944,#59945,#59946,#59947,#59948,
#59949,#59950,#59951,#59952,#59953,#59954,#59955),.UNSPECIFIED.,.T.,.F.,
(4,2,2,2,2,2,2,2,2,2,2,2,2,2,2,2,4),(0.,0.103814244533191,0.207628489066383,
0.311436347509041,0.415244205951698,0.519052064394355,0.622859922837012,
0.726674167370203,0.830488411903395,0.934302656436586,1.03811690096978,
1.14192475941243,1.24573261785509,1.34954047629775,1.45334833474041,1.5571625792736,
1.66097682380679),.UNSPECIFIED.);
#837=B_SPLINE_CURVE_WITH_KNOTS('',3,(#59957,#59958,#59959,#59960,#59961,
#59962,#59963,#59964,#59965,#59966,#59967,#59968,#59969,#59970,#59971,#59972,
#59973,#59974,#59975,#59976,#59977,#59978,#59979,#59980,#59981,#59982,#59983,
#59984,#59985,#59986,#59987,#59988,#59989,#59990),.UNSPECIFIED.,.T.,.F.,
(4,2,2,2,2,2,2,2,2,2,2,2,2,2,2,2,4),(0.,0.103814244533193,0.207628489066386,
0.311436347509045,0.415244205951704,0.519052064394364,0.622859922837024,
0.726674167370216,0.830488411903409,0.934302656436602,1.0381169009698,1.14192475941245,
1.24573261785511,1.34954047629777,1.45334833474043,1.55716257927362,1.66097682380682),
 .UNSPECIFIED.);
#838=B_SPLINE_CURVE_WITH_KNOTS('',3,(#60087,#60088,#60089,#60090,#60091,
#60092,#60093,#60094,#60095,#60096,#60097,#60098,#60099,#60100,#60101,#60102,
#60103,#60104,#60105,#60106,#60107,#60108,#60109,#60110,#60111,#60112,#60113,
#60114,#60115,#60116,#60117,#60118,#60119,#60120),.UNSPECIFIED.,.T.,.F.,
(4,2,2,2,2,2,2,2,2,2,2,2,2,2,2,2,4),(0.,0.126366208363918,0.252732416727836,
0.37909836467664,0.505464312625444,0.631830260574249,0.758196208523054,
0.884562416886971,1.01092862525089,1.13729483361481,1.26366104197873,1.39002698992753,
1.51639293787633,1.64275888582514,1.76912483377394,1.89549104213786,2.02185725050178),
 .UNSPECIFIED.);
#839=B_SPLINE_CURVE_WITH_KNOTS('',3,(#60225,#60226,#60227,#60228,#60229,
#60230,#60231,#60232,#60233,#60234,#60235,#60236,#60237,#60238,#60239,#60240,
#60241,#60242,#60243,#60244,#60245,#60246,#60247,#60248,#60249,#60250,#60251,
#60252,#60253,#60254,#60255,#60256,#60257,#60258),.UNSPECIFIED.,.T.,.F.,
(4,2,2,2,2,2,2,2,2,2,2,2,2,2,2,2,4),(0.,0.126366208363919,0.252732416727838,
0.379098364676642,0.505464312625446,0.631830260574251,0.758196208523055,
0.884562416886973,1.01092862525089,1.13729483361481,1.26366104197873,1.39002698992753,
1.51639293787634,1.64275888582514,1.76912483377395,1.89549104213787,2.02185725050179),
 .UNSPECIFIED.);
#840=B_SPLINE_CURVE_WITH_KNOTS('',3,(#60280,#60281,#60282,#60283,#60284,
#60285,#60286,#60287,#60288,#60289,#60290,#60291,#60292,#60293,#60294,#60295,
#60296,#60297,#60298,#60299,#60300,#60301,#60302,#60303,#60304,#60305,#60306,
#60307,#60308,#60309,#60310,#60311,#60312,#60313),.UNSPECIFIED.,.T.,.F.,
(4,2,2,2,2,2,2,2,2,2,2,2,2,2,2,2,4),(0.,0.126366208363919,0.252732416727837,
0.379098364676641,0.505464312625445,0.63183026057425,0.758196208523054,
0.884562416886973,1.01092862525089,1.13729483361481,1.26366104197873,1.39002698992753,
1.51639293787634,1.64275888582514,1.76912483377395,1.89549104213786,2.02185725050178),
 .UNSPECIFIED.);
#841=B_SPLINE_CURVE_WITH_KNOTS('',3,(#60331,#60332,#60333,#60334,#60335,
#60336,#60337,#60338,#60339,#60340,#60341,#60342,#60343,#60344,#60345,#60346,
#60347,#60348,#60349,#60350,#60351,#60352,#60353,#60354,#60355,#60356,#60357,
#60358,#60359,#60360,#60361,#60362,#60363,#60364),.UNSPECIFIED.,.T.,.F.,
(4,2,2,2,2,2,2,2,2,2,2,2,2,2,2,2,4),(0.,0.126366208363918,0.252732416727836,
0.37909836467664,0.505464312625445,0.631830260574249,0.758196208523054,
0.884562416886972,1.01092862525089,1.13729483361481,1.26366104197873,1.39002698992753,
1.51639293787633,1.64275888582514,1.76912483377394,1.89549104213786,2.02185725050178),
 .UNSPECIFIED.);
#842=B_SPLINE_CURVE_WITH_KNOTS('',3,(#60377,#60378,#60379,#60380),
 .UNSPECIFIED.,.F.,.F.,(4,4),(0.0184096978210031,0.0219555820656529),
 .UNSPECIFIED.);
#843=B_SPLINE_CURVE_WITH_KNOTS('',3,(#60382,#60383,#60384,#60385),
 .UNSPECIFIED.,.F.,.F.,(4,4),(0.0186156132125292,0.0221618161533775),
 .UNSPECIFIED.);
#844=B_SPLINE_CURVE_WITH_KNOTS('',3,(#61360,#61361,#61362,#61363,#61364,
#61365,#61366,#61367,#61368,#61369,#61370,#61371,#61372,#61373,#61374,#61375,
#61376,#61377,#61378,#61379,#61380,#61381,#61382,#61383,#61384,#61385,#61386,
#61387,#61388,#61389,#61390,#61391,#61392,#61393),.UNSPECIFIED.,.T.,.F.,
(4,2,2,2,2,2,2,2,2,2,2,2,2,2,2,2,4),(-2.05511901424686,-1.92665918665082,
-1.79819935905478,-1.66976930986996,-1.54133926068514,-1.41290921150033,
-1.28447916231551,-1.15601933471947,-1.02755950712343,-0.899099679527391,
-0.770639851931354,-0.642209802746534,-0.513779753561715,-0.385349704376896,
-0.256919655192076,-0.128459827596038,0.),.UNSPECIFIED.);
#845=B_SPLINE_CURVE_WITH_KNOTS('',3,(#61395,#61396,#61397,#61398,#61399,
#61400,#61401,#61402,#61403,#61404,#61405,#61406,#61407,#61408,#61409,#61410,
#61411,#61412,#61413,#61414,#61415,#61416,#61417,#61418,#61419,#61420,#61421,
#61422,#61423,#61424,#61425,#61426,#61427,#61428),.UNSPECIFIED.,.T.,.F.,
(4,2,2,2,2,2,2,2,2,2,2,2,2,2,2,2,4),(-2.05511901424684,-1.9266591866508,
-1.79819935905477,-1.66976930986995,-1.54133926068513,-1.41290921150031,
-1.2844791623155,-1.15601933471946,-1.02755950712342,-0.899099679527382,
-0.770639851931344,-0.642209802746527,-0.513779753561709,-0.385349704376891,
-0.256919655192072,-0.128459827596036,0.),.UNSPECIFIED.);
#846=B_SPLINE_CURVE_WITH_KNOTS('',3,(#61431,#61432,#61433,#61434,#61435,
#61436,#61437,#61438,#61439,#61440,#61441,#61442,#61443,#61444,#61445,#61446,
#61447,#61448,#61449,#61450,#61451,#61452,#61453,#61454,#61455,#61456,#61457,
#61458,#61459,#61460,#61461,#61462,#61463,#61464),.UNSPECIFIED.,.T.,.F.,
(4,2,2,2,2,2,2,2,2,2,2,2,2,2,2,2,4),(-2.57601194234862,-2.41500757713331,
-2.254003211918,-2.09300608433973,-1.93200895676147,-1.7710118291832,-1.61001470160494,
-1.44901033638962,-1.28800597117431,-1.127001605959,-0.965997240743687,
-0.805000113165422,-0.644002985587156,-0.483005858008892,-0.322008730430627,
-0.161004365215313,0.),.UNSPECIFIED.);
#847=B_SPLINE_CURVE_WITH_KNOTS('',3,(#61467,#61468,#61469,#61470,#61471,
#61472,#61473,#61474,#61475,#61476,#61477,#61478,#61479,#61480,#61481,#61482,
#61483,#61484,#61485,#61486,#61487,#61488,#61489,#61490,#61491,#61492,#61493,
#61494,#61495,#61496,#61497,#61498,#61499,#61500),.UNSPECIFIED.,.T.,.F.,
(4,2,2,2,2,2,2,2,2,2,2,2,2,2,2,2,4),(0.,0.160753606357945,0.321507212715889,
0.4822596093528,0.643012005989711,0.803764402626621,0.964516799263531,1.12527040562148,
1.28602401197942,1.44677761833737,1.60753122469531,1.76828362133222,1.92903601796913,
2.08978841460604,2.25054081124296,2.4112944176009,2.57204802395885),
 .UNSPECIFIED.);
#848=B_SPLINE_CURVE_WITH_KNOTS('',3,(#61503,#61504,#61505,#61506,#61507,
#61508,#61509,#61510,#61511,#61512,#61513,#61514,#61515,#61516,#61517,#61518,
#61519,#61520,#61521,#61522,#61523,#61524,#61525,#61526,#61527,#61528,#61529,
#61530,#61531,#61532,#61533,#61534,#61535,#61536),.UNSPECIFIED.,.T.,.F.,
(4,2,2,2,2,2,2,2,2,2,2,2,2,2,2,2,4),(-2.57601194234859,-2.41500757713328,
-2.25400321191797,-2.09300608433971,-1.93200895676145,-1.77101182918318,
-1.61001470160492,-1.44901033638961,-1.2880059711743,-1.12700160595899,
-0.965997240743677,-0.805000113165413,-0.644002985587149,-0.483005858008886,
-0.322008730430623,-0.161004365215312,0.),.UNSPECIFIED.);
#849=B_SPLINE_CURVE_WITH_KNOTS('',3,(#61539,#61540,#61541,#61542,#61543,
#61544,#61545,#61546,#61547,#61548,#61549,#61550,#61551,#61552,#61553,#61554,
#61555,#61556,#61557,#61558,#61559,#61560,#61561,#61562,#61563,#61564,#61565,
#61566,#61567,#61568,#61569,#61570,#61571,#61572),.UNSPECIFIED.,.T.,.F.,
(4,2,2,2,2,2,2,2,2,2,2,2,2,2,2,2,4),(0.,0.160753606357943,0.321507212715886,
0.482259609352795,0.643012005989704,0.803764402626612,0.964516799263521,
1.12527040562146,1.28602401197941,1.44677761833735,1.60753122469529,1.7682836213322,
1.92903601796911,2.08978841460602,2.25054081124293,2.41129441760087,2.57204802395882),
 .UNSPECIFIED.);
#850=B_SPLINE_CURVE_WITH_KNOTS('',3,(#61577,#61578,#61579,#61580,#61581,
#61582,#61583,#61584,#61585,#61586,#61587,#61588,#61589,#61590,#61591,#61592,
#61593,#61594),.UNSPECIFIED.,.F.,.F.,(4,2,2,2,2,2,2,2,4),(0.,0.127857366097431,
0.255714732194861,0.383570615681227,0.511426499167593,0.639282382653959,
0.767138266140325,0.894995632237756,1.02285299833519),.UNSPECIFIED.);
#851=B_SPLINE_CURVE_WITH_KNOTS('',3,(#61595,#61596,#61597,#61598,#61599,
#61600,#61601,#61602,#61603,#61604,#61605,#61606,#61607,#61608,#61609,#61610,
#61611,#61612),.UNSPECIFIED.,.F.,.F.,(4,2,2,2,2,2,2,2,4),(1.02285299833519,
1.15071036443262,1.27856773053005,1.40642361401641,1.53427949750278,1.66213538098915,
1.78999126447551,1.91784863057294,2.04570599667037),.UNSPECIFIED.);
#852=B_SPLINE_CURVE_WITH_KNOTS('',3,(#61617,#61618,#61619,#61620,#61621,
#61622,#61623,#61624,#61625,#61626,#61627,#61628,#61629,#61630,#61631,#61632,
#61633,#61634),.UNSPECIFIED.,.F.,.F.,(4,2,2,2,2,2,2,2,4),(0.,0.12785736609743,
0.255714732194861,0.383570615681225,0.511426499167589,0.639282382653953,
0.767138266140317,0.894995632237748,1.02285299833518),.UNSPECIFIED.);
#853=B_SPLINE_CURVE_WITH_KNOTS('',3,(#61635,#61636,#61637,#61638,#61639,
#61640,#61641,#61642,#61643,#61644,#61645,#61646,#61647,#61648,#61649,#61650,
#61651,#61652),.UNSPECIFIED.,.F.,.F.,(4,2,2,2,2,2,2,2,4),(1.02285299833518,
1.15071036443261,1.27856773053004,1.4064236140164,1.53427949750277,1.66213538098913,
1.7899912644755,1.91784863057293,2.04570599667036),.UNSPECIFIED.);
#854=(
BOUNDED_SURFACE()
B_SPLINE_SURFACE(3,3,((#49084,#49085,#49086,#49087,#49088,#49089,#49090,
#49091,#49092),(#49093,#49094,#49095,#49096,#49097,#49098,#49099,#49100,
#49101),(#49102,#49103,#49104,#49105,#49106,#49107,#49108,#49109,#49110),
(#49111,#49112,#49113,#49114,#49115,#49116,#49117,#49118,#49119)),
 .UNSPECIFIED.,.F.,.F.,.F.)
B_SPLINE_SURFACE_WITH_KNOTS((4,4),(4,1,1,1,1,1,4),(0.,1.),(0.1657185475802,
0.2191677809649,0.2917200555518,0.3628106421009,0.4321191894168,0.5006571708278,
0.5134509073716),.UNSPECIFIED.)
GEOMETRIC_REPRESENTATION_ITEM()
RATIONAL_B_SPLINE_SURFACE(((1.212997002425,1.212997002425,1.212997002425,
1.212997002425,1.212997002425,1.212997002425,1.212997002425,1.212997002425,
1.212997002425),(0.9290009991916,0.9290009991916,0.9290009991916,0.9290009991916,
0.9290009991916,0.9290009991916,0.9290009991916,0.9290009991916,0.9290009991916),
(0.9290009991916,0.9290009991916,0.9290009991916,0.9290009991916,0.9290009991916,
0.9290009991916,0.9290009991916,0.9290009991916,0.9290009991916),(1.212997002425,
1.212997002425,1.212997002425,1.212997002425,1.212997002425,1.212997002425,
1.212997002425,1.212997002425,1.212997002425)))
REPRESENTATION_ITEM('')
SURFACE()
);
#855=(
BOUNDED_SURFACE()
B_SPLINE_SURFACE(3,3,((#49426,#49427,#49428,#49429,#49430,#49431,#49432,
#49433,#49434,#49435,#49436),(#49437,#49438,#49439,#49440,#49441,#49442,
#49443,#49444,#49445,#49446,#49447),(#49448,#49449,#49450,#49451,#49452,
#49453,#49454,#49455,#49456,#49457,#49458),(#49459,#49460,#49461,#49462,
#49463,#49464,#49465,#49466,#49467,#49468,#49469)),.UNSPECIFIED.,.F.,.F.,
 .F.)
B_SPLINE_SURFACE_WITH_KNOTS((4,4),(4,1,1,1,1,1,1,1,4),(0.,1.),(0.4912064856134,
0.5104451093027,0.5824328871872,0.6465099292207,0.7028608084679,0.7531387245364,
0.7991472729598,0.8414732732765,0.8528970245468),.UNSPECIFIED.)
GEOMETRIC_REPRESENTATION_ITEM()
RATIONAL_B_SPLINE_SURFACE(((1.212994991089,1.212994991089,1.212994991089,
1.212994991089,1.212994991089,1.212994991089,1.212994991089,1.212994991089,
1.212994991089,1.212994991089,1.212994991089),(0.9290016696369,0.9290016696369,
0.9290016696369,0.9290016696369,0.9290016696369,0.9290016696369,0.9290016696369,
0.9290016696369,0.9290016696369,0.9290016696369,0.9290016696369),(0.9290016696369,
0.9290016696369,0.9290016696369,0.9290016696369,0.9290016696369,0.9290016696369,
0.9290016696369,0.9290016696369,0.9290016696369,0.9290016696369,0.9290016696369),
(1.212994991089,1.212994991089,1.212994991089,1.212994991089,1.212994991089,
1.212994991089,1.212994991089,1.212994991089,1.212994991089,1.212994991089,
1.212994991089)))
REPRESENTATION_ITEM('')
SURFACE()
);
#856=(
BOUNDED_SURFACE()
B_SPLINE_SURFACE(3,3,((#49586,#49587,#49588,#49589,#49590,#49591,#49592,
#49593,#49594),(#49595,#49596,#49597,#49598,#49599,#49600,#49601,#49602,
#49603),(#49604,#49605,#49606,#49607,#49608,#49609,#49610,#49611,#49612),
(#49613,#49614,#49615,#49616,#49617,#49618,#49619,#49620,#49621)),
 .UNSPECIFIED.,.F.,.F.,.F.)
B_SPLINE_SURFACE_WITH_KNOTS((4,4),(4,1,1,1,1,1,4),(0.,1.),(0.4865185456842,
0.4989653295554,0.5676881330315,0.6372726174693,0.7085358956321,0.7811839361635,
0.8342456994508),.UNSPECIFIED.)
GEOMETRIC_REPRESENTATION_ITEM()
RATIONAL_B_SPLINE_SURFACE(((1.212997004616,1.212997004616,1.212997004616,
1.212997004616,1.212997004616,1.212997004616,1.212997004616,1.212997004616,
1.212997004616),(0.9290009984612,0.9290009984612,0.9290009984612,0.9290009984612,
0.9290009984612,0.9290009984612,0.9290009984612,0.9290009984612,0.9290009984612),
(0.9290009984612,0.9290009984612,0.9290009984612,0.9290009984612,0.9290009984612,
0.9290009984612,0.9290009984612,0.9290009984612,0.9290009984612),(1.212997004616,
1.212997004616,1.212997004616,1.212997004616,1.212997004616,1.212997004616,
1.212997004616,1.212997004616,1.212997004616)))
REPRESENTATION_ITEM('')
SURFACE()
);
#857=(
BOUNDED_SURFACE()
B_SPLINE_SURFACE(3,3,((#49652,#49653,#49654,#49655,#49656,#49657,#49658,
#49659,#49660),(#49661,#49662,#49663,#49664,#49665,#49666,#49667,#49668,
#49669),(#49670,#49671,#49672,#49673,#49674,#49675,#49676,#49677,#49678),
(#49679,#49680,#49681,#49682,#49683,#49684,#49685,#49686,#49687)),
 .UNSPECIFIED.,.F.,.F.,.F.)
B_SPLINE_SURFACE_WITH_KNOTS((4,4),(4,1,1,1,1,1,4),(0.,1.),(0.1657200365356,
0.218898549315,0.2912491980129,0.3619657900993,0.4315535161345,0.500650977664,
0.5134507157886),.UNSPECIFIED.)
GEOMETRIC_REPRESENTATION_ITEM()
RATIONAL_B_SPLINE_SURFACE(((1.212996916314,1.212996916314,1.212996916314,
1.212996916314,1.212996916314,1.212996916314,1.212996916314,1.212996916314,
1.212996916314),(0.9290010278954,0.9290010278954,0.9290010278954,0.9290010278954,
0.9290010278954,0.9290010278954,0.9290010278954,0.9290010278954,0.9290010278954),
(0.9290010278954,0.9290010278954,0.9290010278954,0.9290010278954,0.9290010278954,
0.9290010278954,0.9290010278954,0.9290010278954,0.9290010278954),(1.212996916314,
1.212996916314,1.212996916314,1.212996916314,1.212996916314,1.212996916314,
1.212996916314,1.212996916314,1.212996916314)))
REPRESENTATION_ITEM('')
SURFACE()
);
#858=(
BOUNDED_SURFACE()
B_SPLINE_SURFACE(3,3,((#49705,#49706,#49707,#49708,#49709,#49710,#49711,
#49712,#49713,#49714,#49715),(#49716,#49717,#49718,#49719,#49720,#49721,
#49722,#49723,#49724,#49725,#49726),(#49727,#49728,#49729,#49730,#49731,
#49732,#49733,#49734,#49735,#49736,#49737),(#49738,#49739,#49740,#49741,
#49742,#49743,#49744,#49745,#49746,#49747,#49748)),.UNSPECIFIED.,.F.,.F.,
 .F.)
B_SPLINE_SURFACE_WITH_KNOTS((4,4),(4,1,1,1,1,1,1,1,4),(0.,1.),(0.1471313081811,
0.1585267267235,0.2008527270402,0.2468612754635,0.297139191532,0.3534900707792,
0.4175671128126,0.4895548906971,0.5087566656269),.UNSPECIFIED.)
GEOMETRIC_REPRESENTATION_ITEM()
RATIONAL_B_SPLINE_SURFACE(((1.212994990549,1.212994990549,1.212994990549,
1.212994990549,1.212994990549,1.212994990549,1.212994990549,1.212994990549,
1.212994990549,1.212994990549,1.212994990549),(0.9290016698171,0.9290016698171,
0.9290016698171,0.9290016698171,0.9290016698171,0.9290016698171,0.9290016698171,
0.9290016698171,0.9290016698171,0.9290016698171,0.9290016698171),(0.9290016698171,
0.9290016698171,0.9290016698171,0.9290016698171,0.9290016698171,0.9290016698171,
0.9290016698171,0.9290016698171,0.9290016698171,0.9290016698171,0.9290016698171),
(1.212994990549,1.212994990549,1.212994990549,1.212994990549,1.212994990549,
1.212994990549,1.212994990549,1.212994990549,1.212994990549,1.212994990549,
1.212994990549)))
REPRESENTATION_ITEM('')
SURFACE()
);
#859=(
BOUNDED_SURFACE()
B_SPLINE_SURFACE(3,3,((#49816,#49817,#49818,#49819,#49820,#49821,#49822,
#49823,#49824,#49825,#49826),(#49827,#49828,#49829,#49830,#49831,#49832,
#49833,#49834,#49835,#49836,#49837),(#49838,#49839,#49840,#49841,#49842,
#49843,#49844,#49845,#49846,#49847,#49848),(#49849,#49850,#49851,#49852,
#49853,#49854,#49855,#49856,#49857,#49858,#49859)),.UNSPECIFIED.,.F.,.F.,
 .F.)
B_SPLINE_SURFACE_WITH_KNOTS((4,4),(4,1,1,1,1,1,1,1,4),(0.,1.),(0.4912064856134,
0.5104451093027,0.5824328871872,0.6465099292207,0.7028608084679,0.7531387245364,
0.7991472729597,0.8414732732765,0.8528970245468),.UNSPECIFIED.)
GEOMETRIC_REPRESENTATION_ITEM()
RATIONAL_B_SPLINE_SURFACE(((1.212994991089,1.212994991089,1.212994991089,
1.212994991089,1.212994991089,1.212994991089,1.212994991089,1.212994991089,
1.212994991089,1.212994991089,1.212994991089),(0.9290016696369,0.9290016696369,
0.9290016696369,0.9290016696369,0.9290016696369,0.9290016696369,0.9290016696369,
0.9290016696369,0.9290016696369,0.9290016696369,0.9290016696369),(0.9290016696369,
0.9290016696369,0.9290016696369,0.9290016696369,0.9290016696369,0.9290016696369,
0.9290016696369,0.9290016696369,0.9290016696369,0.9290016696369,0.9290016696369),
(1.212994991089,1.212994991089,1.212994991089,1.212994991089,1.212994991089,
1.212994991089,1.212994991089,1.212994991089,1.212994991089,1.212994991089,
1.212994991089)))
REPRESENTATION_ITEM('')
SURFACE()
);
#860=(
BOUNDED_SURFACE()
B_SPLINE_SURFACE(3,3,((#49975,#49976,#49977,#49978,#49979,#49980,#49981,
#49982,#49983),(#49984,#49985,#49986,#49987,#49988,#49989,#49990,#49991,
#49992),(#49993,#49994,#49995,#49996,#49997,#49998,#49999,#50000,#50001),
(#50002,#50003,#50004,#50005,#50006,#50007,#50008,#50009,#50010)),
 .UNSPECIFIED.,.F.,.F.,.F.)
B_SPLINE_SURFACE_WITH_KNOTS((4,4),(4,1,1,1,1,1,4),(0.,1.),(0.4865169701774,
0.499349022336,0.5684464838655,0.6380342099007,0.7087508019872,0.781101450685,
0.8342465447531),.UNSPECIFIED.)
GEOMETRIC_REPRESENTATION_ITEM()
RATIONAL_B_SPLINE_SURFACE(((1.21299691379,1.21299691379,1.21299691379,1.21299691379,
1.21299691379,1.21299691379,1.21299691379,1.21299691379,1.21299691379),
(0.9290010287368,0.9290010287368,0.9290010287368,0.9290010287368,0.9290010287368,
0.9290010287368,0.9290010287368,0.9290010287368,0.9290010287368),(0.9290010287368,
0.9290010287368,0.9290010287368,0.9290010287368,0.9290010287368,0.9290010287368,
0.9290010287368,0.9290010287368,0.9290010287368),(1.21299691379,1.21299691379,
1.21299691379,1.21299691379,1.21299691379,1.21299691379,1.21299691379,1.21299691379,
1.21299691379)))
REPRESENTATION_ITEM('')
SURFACE()
);
#861=(
BOUNDED_SURFACE()
B_SPLINE_SURFACE(3,3,((#50032,#50033,#50034,#50035,#50036,#50037,#50038,
#50039,#50040),(#50041,#50042,#50043,#50044,#50045,#50046,#50047,#50048,
#50049),(#50050,#50051,#50052,#50053,#50054,#50055,#50056,#50057,#50058),
(#50059,#50060,#50061,#50062,#50063,#50064,#50065,#50066,#50067)),
 .UNSPECIFIED.,.F.,.F.,.F.)
B_SPLINE_SURFACE_WITH_KNOTS((4,4),(4,1,1,1,1,1,4),(0.,1.),(0.4865185456842,
0.4989653295554,0.5676881330316,0.6372726174694,0.7085358956322,0.7811839361635,
0.8342456994508),.UNSPECIFIED.)
GEOMETRIC_REPRESENTATION_ITEM()
RATIONAL_B_SPLINE_SURFACE(((1.212997004616,1.212997004616,1.212997004616,
1.212997004616,1.212997004616,1.212997004616,1.212997004616,1.212997004616,
1.212997004616),(0.9290009984612,0.9290009984612,0.9290009984612,0.9290009984612,
0.9290009984612,0.9290009984612,0.9290009984612,0.9290009984612,0.9290009984612),
(0.9290009984612,0.9290009984612,0.9290009984612,0.9290009984612,0.9290009984612,
0.9290009984612,0.9290009984612,0.9290009984612,0.9290009984612),(1.212997004616,
1.212997004616,1.212997004616,1.212997004616,1.212997004616,1.212997004616,
1.212997004616,1.212997004616,1.212997004616)))
REPRESENTATION_ITEM('')
SURFACE()
);
#862=(
BOUNDED_SURFACE()
B_SPLINE_SURFACE(3,3,((#50155,#50156,#50157,#50158,#50159,#50160,#50161,
#50162,#50163,#50164,#50165),(#50166,#50167,#50168,#50169,#50170,#50171,
#50172,#50173,#50174,#50175,#50176),(#50177,#50178,#50179,#50180,#50181,
#50182,#50183,#50184,#50185,#50186,#50187),(#50188,#50189,#50190,#50191,
#50192,#50193,#50194,#50195,#50196,#50197,#50198)),.UNSPECIFIED.,.F.,.F.,
 .F.)
B_SPLINE_SURFACE_WITH_KNOTS((4,4),(4,1,1,1,1,1,1,1,4),(0.,1.),(0.4912064856134,
0.5104451093027,0.5824328871873,0.6465099292207,0.7028608084679,0.7531387245365,
0.7991472729598,0.8414732732765,0.8528970245468),.UNSPECIFIED.)
GEOMETRIC_REPRESENTATION_ITEM()
RATIONAL_B_SPLINE_SURFACE(((1.212994991089,1.212994991089,1.212994991089,
1.212994991089,1.212994991089,1.212994991089,1.212994991089,1.212994991089,
1.212994991089,1.212994991089,1.212994991089),(0.9290016696369,0.9290016696369,
0.9290016696369,0.9290016696369,0.9290016696369,0.9290016696369,0.9290016696369,
0.9290016696369,0.9290016696369,0.9290016696369,0.9290016696369),(0.9290016696369,
0.9290016696369,0.9290016696369,0.9290016696369,0.9290016696369,0.9290016696369,
0.9290016696369,0.9290016696369,0.9290016696369,0.9290016696369,0.9290016696369),
(1.212994991089,1.212994991089,1.212994991089,1.212994991089,1.212994991089,
1.212994991089,1.212994991089,1.212994991089,1.212994991089,1.212994991089,
1.212994991089)))
REPRESENTATION_ITEM('')
SURFACE()
);
#863=(
BOUNDED_SURFACE()
B_SPLINE_SURFACE(3,3,((#50328,#50329,#50330,#50331,#50332,#50333,#50334,
#50335,#50336),(#50337,#50338,#50339,#50340,#50341,#50342,#50343,#50344,
#50345),(#50346,#50347,#50348,#50349,#50350,#50351,#50352,#50353,#50354),
(#50355,#50356,#50357,#50358,#50359,#50360,#50361,#50362,#50363)),
 .UNSPECIFIED.,.F.,.F.,.F.)
B_SPLINE_SURFACE_WITH_KNOTS((4,4),(4,1,1,1,1,1,4),(0.,1.),(0.4865169701774,
0.499349022336,0.5684464838655,0.6380342099007,0.7087508019872,0.781101450685,
0.8342465447531),.UNSPECIFIED.)
GEOMETRIC_REPRESENTATION_ITEM()
RATIONAL_B_SPLINE_SURFACE(((1.21299691379,1.21299691379,1.21299691379,1.21299691379,
1.21299691379,1.21299691379,1.21299691379,1.21299691379,1.21299691379),
(0.9290010287368,0.9290010287368,0.9290010287368,0.9290010287368,0.9290010287368,
0.9290010287368,0.9290010287368,0.9290010287368,0.9290010287368),(0.9290010287368,
0.9290010287368,0.9290010287368,0.9290010287368,0.9290010287368,0.9290010287368,
0.9290010287368,0.9290010287368,0.9290010287368),(1.21299691379,1.21299691379,
1.21299691379,1.21299691379,1.21299691379,1.21299691379,1.21299691379,1.21299691379,
1.21299691379)))
REPRESENTATION_ITEM('')
SURFACE()
);
#864=(
BOUNDED_SURFACE()
B_SPLINE_SURFACE(3,3,((#50368,#50369,#50370,#50371,#50372,#50373,#50374,
#50375,#50376),(#50377,#50378,#50379,#50380,#50381,#50382,#50383,#50384,
#50385),(#50386,#50387,#50388,#50389,#50390,#50391,#50392,#50393,#50394),
(#50395,#50396,#50397,#50398,#50399,#50400,#50401,#50402,#50403)),
 .UNSPECIFIED.,.F.,.F.,.F.)
B_SPLINE_SURFACE_WITH_KNOTS((4,4),(4,1,1,1,1,1,4),(0.,1.),(0.1657185475802,
0.2191677809649,0.2917200555518,0.3628106421009,0.4321191894168,0.5006571708278,
0.5134509073716),.UNSPECIFIED.)
GEOMETRIC_REPRESENTATION_ITEM()
RATIONAL_B_SPLINE_SURFACE(((1.212997002425,1.212997002425,1.212997002425,
1.212997002425,1.212997002425,1.212997002425,1.212997002425,1.212997002425,
1.212997002425),(0.9290009991916,0.9290009991916,0.9290009991916,0.9290009991916,
0.9290009991916,0.9290009991916,0.9290009991916,0.9290009991916,0.9290009991916),
(0.9290009991916,0.9290009991916,0.9290009991916,0.9290009991916,0.9290009991916,
0.9290009991916,0.9290009991916,0.9290009991916,0.9290009991916),(1.212997002425,
1.212997002425,1.212997002425,1.212997002425,1.212997002425,1.212997002425,
1.212997002425,1.212997002425,1.212997002425)))
REPRESENTATION_ITEM('')
SURFACE()
);
#865=(
BOUNDED_SURFACE()
B_SPLINE_SURFACE(3,3,((#50434,#50435,#50436,#50437,#50438,#50439,#50440,
#50441,#50442,#50443,#50444),(#50445,#50446,#50447,#50448,#50449,#50450,
#50451,#50452,#50453,#50454,#50455),(#50456,#50457,#50458,#50459,#50460,
#50461,#50462,#50463,#50464,#50465,#50466),(#50467,#50468,#50469,#50470,
#50471,#50472,#50473,#50474,#50475,#50476,#50477)),.UNSPECIFIED.,.F.,.F.,
 .F.)
B_SPLINE_SURFACE_WITH_KNOTS((4,4),(4,1,1,1,1,1,1,1,4),(0.,1.),(0.1471313081811,
0.1585267267235,0.2008527270402,0.2468612754635,0.2971391915321,0.3534900707793,
0.4175671128127,0.4895548906973,0.5087566656269),.UNSPECIFIED.)
GEOMETRIC_REPRESENTATION_ITEM()
RATIONAL_B_SPLINE_SURFACE(((1.212994990549,1.212994990549,1.212994990549,
1.212994990549,1.212994990549,1.212994990549,1.212994990549,1.212994990549,
1.212994990549,1.212994990549,1.212994990549),(0.9290016698171,0.9290016698171,
0.9290016698171,0.9290016698171,0.9290016698171,0.9290016698171,0.9290016698171,
0.9290016698171,0.9290016698171,0.9290016698171,0.9290016698171),(0.9290016698171,
0.9290016698171,0.9290016698171,0.9290016698171,0.9290016698171,0.9290016698171,
0.9290016698171,0.9290016698171,0.9290016698171,0.9290016698171,0.9290016698171),
(1.212994990549,1.212994990549,1.212994990549,1.212994990549,1.212994990549,
1.212994990549,1.212994990549,1.212994990549,1.212994990549,1.212994990549,
1.212994990549)))
REPRESENTATION_ITEM('')
SURFACE()
);
#866=(
BOUNDED_SURFACE()
B_SPLINE_SURFACE(3,3,((#50606,#50607,#50608,#50609,#50610,#50611,#50612,
#50613,#50614,#50615,#50616),(#50617,#50618,#50619,#50620,#50621,#50622,
#50623,#50624,#50625,#50626,#50627),(#50628,#50629,#50630,#50631,#50632,
#50633,#50634,#50635,#50636,#50637,#50638),(#50639,#50640,#50641,#50642,
#50643,#50644,#50645,#50646,#50647,#50648,#50649)),.UNSPECIFIED.,.F.,.F.,
 .F.)
B_SPLINE_SURFACE_WITH_KNOTS((4,4),(4,1,1,1,1,1,1,1,4),(0.,1.),(0.4912070765429,
0.5104451093027,0.5824328871872,0.6465099292207,0.7028608084679,0.7531387245365,
0.7991472729598,0.8414732732765,0.8528428231596),.UNSPECIFIED.)
GEOMETRIC_REPRESENTATION_ITEM()
RATIONAL_B_SPLINE_SURFACE(((1.212994990461,1.212994990461,1.212994990461,
1.212994990461,1.212994990461,1.212994990461,1.212994990461,1.212994990461,
1.212994990461,1.212994990461,1.212994990461),(0.9290016698463,0.9290016698463,
0.9290016698463,0.9290016698463,0.9290016698463,0.9290016698463,0.9290016698463,
0.9290016698463,0.9290016698463,0.9290016698463,0.9290016698463),(0.9290016698463,
0.9290016698463,0.9290016698463,0.9290016698463,0.9290016698463,0.9290016698463,
0.9290016698463,0.9290016698463,0.9290016698463,0.9290016698463,0.9290016698463),
(1.212994990461,1.212994990461,1.212994990461,1.212994990461,1.212994990461,
1.212994990461,1.212994990461,1.212994990461,1.212994990461,1.212994990461,
1.212994990461)))
REPRESENTATION_ITEM('')
SURFACE()
);
#867=(
BOUNDED_SURFACE()
B_SPLINE_SURFACE(3,3,((#50653,#50654,#50655,#50656,#50657,#50658,#50659,
#50660,#50661,#50662,#50663),(#50664,#50665,#50666,#50667,#50668,#50669,
#50670,#50671,#50672,#50673,#50674),(#50675,#50676,#50677,#50678,#50679,
#50680,#50681,#50682,#50683,#50684,#50685),(#50686,#50687,#50688,#50689,
#50690,#50691,#50692,#50693,#50694,#50695,#50696)),.UNSPECIFIED.,.F.,.F.,
 .F.)
B_SPLINE_SURFACE_WITH_KNOTS((4,4),(4,1,1,1,1,1,1,1,4),(0.,1.),(0.1471313081811,
0.1585267267235,0.2008527270402,0.2468612754635,0.2971391915321,0.3534900707793,
0.4175671128127,0.4895548906972,0.5087566656269),.UNSPECIFIED.)
GEOMETRIC_REPRESENTATION_ITEM()
RATIONAL_B_SPLINE_SURFACE(((1.212994990549,1.212994990549,1.212994990549,
1.212994990549,1.212994990549,1.212994990549,1.212994990549,1.212994990549,
1.212994990549,1.212994990549,1.212994990549),(0.9290016698171,0.9290016698171,
0.9290016698171,0.9290016698171,0.9290016698171,0.9290016698171,0.9290016698171,
0.9290016698171,0.9290016698171,0.9290016698171,0.9290016698171),(0.9290016698171,
0.9290016698171,0.9290016698171,0.9290016698171,0.9290016698171,0.9290016698171,
0.9290016698171,0.9290016698171,0.9290016698171,0.9290016698171,0.9290016698171),
(1.212994990549,1.212994990549,1.212994990549,1.212994990549,1.212994990549,
1.212994990549,1.212994990549,1.212994990549,1.212994990549,1.212994990549,
1.212994990549)))
REPRESENTATION_ITEM('')
SURFACE()
);
#868=(
BOUNDED_SURFACE()
B_SPLINE_SURFACE(3,3,((#50771,#50772,#50773,#50774,#50775,#50776,#50777,
#50778,#50779),(#50780,#50781,#50782,#50783,#50784,#50785,#50786,#50787,
#50788),(#50789,#50790,#50791,#50792,#50793,#50794,#50795,#50796,#50797),
(#50798,#50799,#50800,#50801,#50802,#50803,#50804,#50805,#50806)),
 .UNSPECIFIED.,.F.,.F.,.F.)
B_SPLINE_SURFACE_WITH_KNOTS((4,4),(4,1,1,1,1,1,4),(0.,1.),(0.1657200395971,
0.218898549315,0.2912491980128,0.3619657900993,0.4315535161345,0.500650977664,
0.5134507157828),.UNSPECIFIED.)
GEOMETRIC_REPRESENTATION_ITEM()
RATIONAL_B_SPLINE_SURFACE(((1.212996916314,1.212996916314,1.212996916314,
1.212996916314,1.212996916314,1.212996916314,1.212996916314,1.212996916314,
1.212996916314),(0.9290010278954,0.9290010278954,0.9290010278954,0.9290010278954,
0.9290010278954,0.9290010278954,0.9290010278954,0.9290010278954,0.9290010278954),
(0.9290010278954,0.9290010278954,0.9290010278954,0.9290010278954,0.9290010278954,
0.9290010278954,0.9290010278954,0.9290010278954,0.9290010278954),(1.212996916314,
1.212996916314,1.212996916314,1.212996916314,1.212996916314,1.212996916314,
1.212996916314,1.212996916314,1.212996916314)))
REPRESENTATION_ITEM('')
SURFACE()
);
#869=(
BOUNDED_SURFACE()
B_SPLINE_SURFACE(3,3,((#50824,#50825,#50826,#50827,#50828,#50829,#50830,
#50831,#50832,#50833,#50834),(#50835,#50836,#50837,#50838,#50839,#50840,
#50841,#50842,#50843,#50844,#50845),(#50846,#50847,#50848,#50849,#50850,
#50851,#50852,#50853,#50854,#50855,#50856),(#50857,#50858,#50859,#50860,
#50861,#50862,#50863,#50864,#50865,#50866,#50867)),.UNSPECIFIED.,.F.,.F.,
 .F.)
B_SPLINE_SURFACE_WITH_KNOTS((4,4),(4,1,1,1,1,1,1,1,4),(0.,1.),(0.1471313081811,
0.1585267267235,0.2008527270402,0.2468612754635,0.297139191532,0.3534900707792,
0.4175671128127,0.4895548906972,0.5087566656269),.UNSPECIFIED.)
GEOMETRIC_REPRESENTATION_ITEM()
RATIONAL_B_SPLINE_SURFACE(((1.212994990549,1.212994990549,1.212994990549,
1.212994990549,1.212994990549,1.212994990549,1.212994990549,1.212994990549,
1.212994990549,1.212994990549,1.212994990549),(0.9290016698171,0.9290016698171,
0.9290016698171,0.9290016698171,0.9290016698171,0.9290016698171,0.9290016698171,
0.9290016698171,0.9290016698171,0.9290016698171,0.9290016698171),(0.9290016698171,
0.9290016698171,0.9290016698171,0.9290016698171,0.9290016698171,0.9290016698171,
0.9290016698171,0.9290016698171,0.9290016698171,0.9290016698171,0.9290016698171),
(1.212994990549,1.212994990549,1.212994990549,1.212994990549,1.212994990549,
1.212994990549,1.212994990549,1.212994990549,1.212994990549,1.212994990549,
1.212994990549)))
REPRESENTATION_ITEM('')
SURFACE()
);
#870=(
BOUNDED_SURFACE()
B_SPLINE_SURFACE(2,2,((#51565,#51566,#51567,#51568,#51569,#51570,#51571,
#51572,#51573),(#51574,#51575,#51576,#51577,#51578,#51579,#51580,#51581,
#51582),(#51583,#51584,#51585,#51586,#51587,#51588,#51589,#51590,#51591)),
 .UNSPECIFIED.,.F.,.T.,.F.)
B_SPLINE_SURFACE_WITH_KNOTS((3,3),(3,2,2,2,3),(-1.48658674941058,-0.838836123214499),
(-3.14159265358979,-1.5707963267949,0.,1.5707963267949,3.14159265358979),
 .UNSPECIFIED.)
GEOMETRIC_REPRESENTATION_ITEM()
RATIONAL_B_SPLINE_SURFACE(((1.,0.707106781186548,1.,0.707106781186548,1.,
0.707106781186548,1.,0.707106781186548,1.),(0.948009249396791,0.67034376887604,
0.948009249396791,0.67034376887604,0.948009249396791,0.67034376887604,0.948009249396791,
0.67034376887604,0.948009249396791),(1.,0.707106781186548,1.,0.707106781186548,
1.,0.707106781186548,1.,0.707106781186548,1.)))
REPRESENTATION_ITEM('')
SURFACE()
);
#871=(
BOUNDED_SURFACE()
B_SPLINE_SURFACE(2,2,((#52773,#52774,#52775,#52776,#52777,#52778,#52779,
#52780,#52781),(#52782,#52783,#52784,#52785,#52786,#52787,#52788,#52789,
#52790),(#52791,#52792,#52793,#52794,#52795,#52796,#52797,#52798,#52799)),
 .UNSPECIFIED.,.F.,.T.,.F.)
B_SPLINE_SURFACE_WITH_KNOTS((3,3),(3,2,2,2,3),(-1.57079634483717,-0.955666854650568),
(-3.14159265358979,-1.5707963267949,0.,1.5707963267949,3.14159265358979),
 .UNSPECIFIED.)
GEOMETRIC_REPRESENTATION_ITEM()
RATIONAL_B_SPLINE_SURFACE(((1.,0.707106781186548,1.,0.707106781186548,1.,
0.707106781186548,1.,0.707106781186548,1.),(0.953073640802859,0.673924834381854,
0.953073640802859,0.673924834381854,0.953073640802859,0.673924834381854,
0.953073640802859,0.673924834381854,0.953073640802859),(1.,0.707106781186548,
1.,0.707106781186548,1.,0.707106781186548,1.,0.707106781186548,1.)))
REPRESENTATION_ITEM('')
SURFACE()
);
#872=(
BOUNDED_SURFACE()
B_SPLINE_SURFACE(2,2,((#52806,#52807,#52808,#52809,#52810,#52811,#52812,
#52813,#52814),(#52815,#52816,#52817,#52818,#52819,#52820,#52821,#52822,
#52823),(#52824,#52825,#52826,#52827,#52828,#52829,#52830,#52831,#52832)),
 .UNSPECIFIED.,.F.,.T.,.F.)
B_SPLINE_SURFACE_WITH_KNOTS((3,3),(3,2,2,2,3),(-1.57079630698122,-0.955666850767325),
(-3.14159265358979,-1.5707963267949,0.,1.5707963267949,3.14159265358979),
 .UNSPECIFIED.)
GEOMETRIC_REPRESENTATION_ITEM()
RATIONAL_B_SPLINE_SURFACE(((1.,0.707106781186548,1.,0.707106781186548,1.,
0.707106781186548,1.,0.707106781186548,1.),(0.953073645945215,0.673924838018048,
0.953073645945215,0.673924838018048,0.953073645945215,0.673924838018048,
0.953073645945215,0.673924838018048,0.953073645945215),(1.,0.707106781186548,
1.,0.707106781186548,1.,0.707106781186548,1.,0.707106781186548,1.)))
REPRESENTATION_ITEM('')
SURFACE()
);
#873=(
BOUNDED_SURFACE()
B_SPLINE_SURFACE(2,2,((#52834,#52835,#52836,#52837,#52838,#52839,#52840,
#52841,#52842),(#52843,#52844,#52845,#52846,#52847,#52848,#52849,#52850,
#52851),(#52852,#52853,#52854,#52855,#52856,#52857,#52858,#52859,#52860)),
 .UNSPECIFIED.,.F.,.T.,.F.)
B_SPLINE_SURFACE_WITH_KNOTS((3,3),(3,2,2,2,3),(-1.57079632708437,-0.955666871754965),
(-3.14159265358979,-1.5707963267949,0.,1.5707963267949,3.14159265358979),
 .UNSPECIFIED.)
GEOMETRIC_REPRESENTATION_ITEM()
RATIONAL_B_SPLINE_SURFACE(((1.,0.707106781186548,1.,0.707106781186548,1.,
0.707106781186548,1.,0.707106781186548,1.),(0.953073646079135,0.673924838112744,
0.953073646079135,0.673924838112744,0.953073646079135,0.673924838112744,
0.953073646079135,0.673924838112744,0.953073646079135),(1.,0.707106781186548,
1.,0.707106781186548,1.,0.707106781186548,1.,0.707106781186548,1.)))
REPRESENTATION_ITEM('')
SURFACE()
);
#874=TOROIDAL_SURFACE('',#34169,8.96,2.54);
#875=TOROIDAL_SURFACE('',#34194,49.79,2.54);
#876=TOROIDAL_SURFACE('',#34210,49.79,2.54);
#877=TOROIDAL_SURFACE('',#34231,8.96,2.54);
#878=TOROIDAL_SURFACE('',#34239,8.96,2.54);
#879=TOROIDAL_SURFACE('',#34256,49.79,2.54);
#880=TOROIDAL_SURFACE('',#34276,49.79,2.54);
#881=TOROIDAL_SURFACE('',#34281,49.79,2.54);
#882=TOROIDAL_SURFACE('',#34296,8.96,2.54);
#883=TOROIDAL_SURFACE('',#34310,49.79,2.54);
#884=TOROIDAL_SURFACE('',#34335,49.79,2.54);
#885=TOROIDAL_SURFACE('',#34337,49.79,2.54);
#886=TOROIDAL_SURFACE('',#34344,44.71,2.54);
#887=TOROIDAL_SURFACE('',#34349,38.29,2.54);
#888=TOROIDAL_SURFACE('',#34393,6.1,0.1);
#889=TOROIDAL_SURFACE('',#34406,7.8,1.2);
#890=TOROIDAL_SURFACE('',#34421,5.1,0.1);
#891=TOROIDAL_SURFACE('',#34434,7.,1.);
#892=TOROIDAL_SURFACE('',#34449,5.1,0.1);
#893=TOROIDAL_SURFACE('',#34462,7.,1.);
#894=TOROIDAL_SURFACE('',#34477,5.4,0.4);
#895=TOROIDAL_SURFACE('',#34831,71.8820000000001,19.0499999999999);
#896=TOROIDAL_SURFACE('',#35092,1.00000000000001,0.5);
#897=TOROIDAL_SURFACE('',#35097,1.,0.499999999999994);
#898=TOROIDAL_SURFACE('',#35973,15.5,0.5);
#899=TOROIDAL_SURFACE('',#35982,15.5,0.5);
#900=TOROIDAL_SURFACE('',#36020,19.,0.500000000000029);
#901=TOROIDAL_SURFACE('',#36030,19.,0.499999999999998);
#902=TOROIDAL_SURFACE('',#36067,15.5,0.5);
#903=TOROIDAL_SURFACE('',#36074,15.5,0.5);
#904=TOROIDAL_SURFACE('',#36098,19.,0.500000000000029);
#905=TOROIDAL_SURFACE('',#36108,19.,0.499999999999998);
#906=TOROIDAL_SURFACE('',#36149,28.,2.);
#907=TOROIDAL_SURFACE('',#36158,32.,2.);
#908=TOROIDAL_SURFACE('',#36745,28.,2.);
#909=TOROIDAL_SURFACE('',#36754,32.,2.);
#910=TOROIDAL_SURFACE('',#38057,56.233130266379,1.78815999999988);
#911=SHAPE_REPRESENTATION_RELATIONSHIP('SRR','None',#61969,#936);
#912=SHAPE_REPRESENTATION_RELATIONSHIP('SRR','None',#61970,#937);
#913=SHAPE_REPRESENTATION_RELATIONSHIP('SRR','None',#61971,#938);
#914=SHAPE_REPRESENTATION_RELATIONSHIP('SRR','None',#61972,#939);
#915=SHAPE_REPRESENTATION_RELATIONSHIP('SRR','None',#61973,#940);
#916=SHAPE_REPRESENTATION_RELATIONSHIP('SRR','None',#61974,#941);
#917=SHAPE_REPRESENTATION_RELATIONSHIP('SRR','None',#61975,#942);
#918=SHAPE_REPRESENTATION_RELATIONSHIP('SRR','None',#61976,#943);
#919=SHAPE_REPRESENTATION_RELATIONSHIP('SRR','None',#61977,#944);
#920=SHAPE_REPRESENTATION_RELATIONSHIP('SRR','None',#61978,#945);
#921=SHAPE_REPRESENTATION_RELATIONSHIP('SRR','None',#61979,#946);
#922=SHAPE_REPRESENTATION_RELATIONSHIP('SRR','None',#61981,#947);
#923=SHAPE_REPRESENTATION_RELATIONSHIP('SRR','None',#61982,#948);
#924=SHAPE_REPRESENTATION_RELATIONSHIP('SRR','None',#61983,#949);
#925=SHAPE_REPRESENTATION_RELATIONSHIP('SRR','None',#61984,#950);
#926=SHAPE_REPRESENTATION_RELATIONSHIP('SRR','None',#61985,#951);
#927=SHAPE_REPRESENTATION_RELATIONSHIP('SRR','None',#61986,#952);
#928=SHAPE_REPRESENTATION_RELATIONSHIP('SRR','None',#61988,#953);
#929=SHAPE_REPRESENTATION_RELATIONSHIP('SRR','None',#61989,#954);
#930=SHAPE_REPRESENTATION_RELATIONSHIP('SRR','None',#61990,#955);
#931=SHAPE_REPRESENTATION_RELATIONSHIP('SRR','None',#61991,#956);
#932=SHAPE_REPRESENTATION_RELATIONSHIP('SRR','None',#61993,#957);
#933=SHAPE_REPRESENTATION_RELATIONSHIP('SRR','None',#61994,#958);
#934=SHAPE_REPRESENTATION_RELATIONSHIP('SRR','None',#61996,#959);
#935=SHAPE_REPRESENTATION_RELATIONSHIP('SRR','None',#61997,#960);
#936=ADVANCED_BREP_SHAPE_REPRESENTATION('',(#1000),#61782);
#937=ADVANCED_BREP_SHAPE_REPRESENTATION('',(#1001),#61783);
#938=ADVANCED_BREP_SHAPE_REPRESENTATION('',(#1002),#61784);
#939=ADVANCED_BREP_SHAPE_REPRESENTATION('',(#1003),#61785);
#940=ADVANCED_BREP_SHAPE_REPRESENTATION('',(#1004),#61786);
#941=ADVANCED_BREP_SHAPE_REPRESENTATION('',(#1005),#61787);
#942=ADVANCED_BREP_SHAPE_REPRESENTATION('',(#1006),#61788);
#943=ADVANCED_BREP_SHAPE_REPRESENTATION('',(#1007),#61789);
#944=ADVANCED_BREP_SHAPE_REPRESENTATION('',(#1008),#61790);
#945=ADVANCED_BREP_SHAPE_REPRESENTATION('',(#1009),#61791);
#946=ADVANCED_BREP_SHAPE_REPRESENTATION('',(#1010,#1011,#1012,#1013,#1014,
#1015,#1016,#1017,#1018,#1019,#1020,#1021,#1022,#1023,#1024),#61792);
#947=ADVANCED_BREP_SHAPE_REPRESENTATION('',(#1025),#61794);
#948=ADVANCED_BREP_SHAPE_REPRESENTATION('',(#1026),#61795);
#949=ADVANCED_BREP_SHAPE_REPRESENTATION('',(#1027),#61796);
#950=ADVANCED_BREP_SHAPE_REPRESENTATION('',(#1028),#61797);
#951=ADVANCED_BREP_SHAPE_REPRESENTATION('',(#1029),#61798);
#952=ADVANCED_BREP_SHAPE_REPRESENTATION('',(#1030),#61799);
#953=ADVANCED_BREP_SHAPE_REPRESENTATION('',(#1031),#61801);
#954=ADVANCED_BREP_SHAPE_REPRESENTATION('',(#1032),#61802);
#955=ADVANCED_BREP_SHAPE_REPRESENTATION('',(#1033),#61803);
#956=ADVANCED_BREP_SHAPE_REPRESENTATION('',(#1034),#61804);
#957=ADVANCED_BREP_SHAPE_REPRESENTATION('',(#1035),#61806);
#958=ADVANCED_BREP_SHAPE_REPRESENTATION('',(#1036),#61807);
#959=ADVANCED_BREP_SHAPE_REPRESENTATION('',(#21),#61809);
#960=ADVANCED_BREP_SHAPE_REPRESENTATION('',(#1037),#61810);
#961=STYLED_ITEM('',(#62149),#1000);
#962=STYLED_ITEM('',(#62156),#1001);
#963=STYLED_ITEM('',(#62163),#1002);
#964=STYLED_ITEM('',(#62163),#1003);
#965=STYLED_ITEM('',(#62163),#1004);
#966=STYLED_ITEM('',(#62163),#1005);
#967=STYLED_ITEM('',(#62142),#1006);
#968=STYLED_ITEM('',(#62149),#1007);
#969=STYLED_ITEM('',(#62142),#1008);
#970=STYLED_ITEM('',(#62142),#1009);
#971=STYLED_ITEM('',(#62135),#1010);
#972=STYLED_ITEM('',(#62135),#1011);
#973=STYLED_ITEM('',(#62135),#1012);
#974=STYLED_ITEM('',(#62135),#1013);
#975=STYLED_ITEM('',(#62135),#1014);
#976=STYLED_ITEM('',(#62135),#1015);
#977=STYLED_ITEM('',(#62135),#1016);
#978=STYLED_ITEM('',(#62135),#1017);
#979=STYLED_ITEM('',(#62135),#1018);
#980=STYLED_ITEM('',(#62135),#1019);
#981=STYLED_ITEM('',(#62135),#1020);
#982=STYLED_ITEM('',(#62135),#1021);
#983=STYLED_ITEM('',(#62135),#1022);
#984=STYLED_ITEM('',(#62135),#1023);
#985=STYLED_ITEM('',(#62135),#1024);
#986=STYLED_ITEM('',(#62135),#1025);
#987=STYLED_ITEM('',(#62142),#1026);
#988=STYLED_ITEM('',(#62142),#1027);
#989=STYLED_ITEM('',(#62170),#1028);
#990=STYLED_ITEM('',(#62142),#1029);
#991=STYLED_ITEM('',(#62135),#1030);
#992=STYLED_ITEM('',(#62156),#1031);
#993=STYLED_ITEM('',(#62156),#1032);
#994=STYLED_ITEM('',(#62156),#1033);
#995=STYLED_ITEM('',(#62163),#1034);
#996=STYLED_ITEM('',(#62149),#1035);
#997=STYLED_ITEM('',(#62149),#1036);
#998=STYLED_ITEM('',(#62170),#21);
#999=STYLED_ITEM('',(#62156),#1037);
#1000=MANIFOLD_SOLID_BREP('Body1',#33791);
#1001=MANIFOLD_SOLID_BREP('Body1',#33792);
#1002=MANIFOLD_SOLID_BREP('Body1',#33793);
#1003=MANIFOLD_SOLID_BREP('Body1',#33794);
#1004=MANIFOLD_SOLID_BREP('Body1',#33795);
#1005=MANIFOLD_SOLID_BREP('Body1',#33796);
#1006=MANIFOLD_SOLID_BREP('Body1',#33797);
#1007=MANIFOLD_SOLID_BREP('Body1',#33798);
#1008=MANIFOLD_SOLID_BREP('Body1',#33799);
#1009=MANIFOLD_SOLID_BREP('Body1',#33800);
#1010=MANIFOLD_SOLID_BREP('Body1',#33801);
#1011=MANIFOLD_SOLID_BREP('Body2',#33802);
#1012=MANIFOLD_SOLID_BREP('Body3',#33803);
#1013=MANIFOLD_SOLID_BREP('Body4',#33804);
#1014=MANIFOLD_SOLID_BREP('Body5',#33805);
#1015=MANIFOLD_SOLID_BREP('Body6',#33806);
#1016=MANIFOLD_SOLID_BREP('Body7',#33807);
#1017=MANIFOLD_SOLID_BREP('Body8',#33808);
#1018=MANIFOLD_SOLID_BREP('Body9',#33809);
#1019=MANIFOLD_SOLID_BREP('Body10',#33810);
#1020=MANIFOLD_SOLID_BREP('Body11',#33811);
#1021=MANIFOLD_SOLID_BREP('Body12',#33812);
#1022=MANIFOLD_SOLID_BREP('Body13',#33813);
#1023=MANIFOLD_SOLID_BREP('Body14',#33814);
#1024=MANIFOLD_SOLID_BREP('Body15',#33815);
#1025=MANIFOLD_SOLID_BREP('Body1',#33816);
#1026=MANIFOLD_SOLID_BREP('Body1',#33817);
#1027=MANIFOLD_SOLID_BREP('Body1',#33818);
#1028=MANIFOLD_SOLID_BREP('Body1',#33819);
#1029=MANIFOLD_SOLID_BREP('Body1',#33820);
#1030=MANIFOLD_SOLID_BREP('Body1',#33821);
#1031=MANIFOLD_SOLID_BREP('Body1',#33822);
#1032=MANIFOLD_SOLID_BREP('Body1',#33823);
#1033=MANIFOLD_SOLID_BREP('Body1',#33824);
#1034=MANIFOLD_SOLID_BREP('Body1',#33825);
#1035=MANIFOLD_SOLID_BREP('Body1',#33826);
#1036=MANIFOLD_SOLID_BREP('Body1',#33827);
#1037=MANIFOLD_SOLID_BREP('Body1',#33839);
#1038=CYLINDRICAL_SURFACE('',#34129,20.);
#1039=CYLINDRICAL_SURFACE('',#34132,5.);
#1040=CYLINDRICAL_SURFACE('',#34137,5.);
#1041=CYLINDRICAL_SURFACE('',#34141,75.);
#1042=CYLINDRICAL_SURFACE('',#34143,75.);
#1043=CYLINDRICAL_SURFACE('',#34145,5.);
#1044=CYLINDRICAL_SURFACE('',#34150,75.);
#1045=CYLINDRICAL_SURFACE('',#34167,11.5);
#1046=CYLINDRICAL_SURFACE('',#34173,2.54);
#1047=CYLINDRICAL_SURFACE('',#34190,5.75);
#1048=CYLINDRICAL_SURFACE('',#34191,5.75);
#1049=CYLINDRICAL_SURFACE('',#34192,5.75);
#1050=CYLINDRICAL_SURFACE('',#34193,5.75);
#1051=CYLINDRICAL_SURFACE('',#34199,47.25);
#1052=CYLINDRICAL_SURFACE('',#34221,2.54);
#1053=CYLINDRICAL_SURFACE('',#34224,2.54);
#1054=CYLINDRICAL_SURFACE('',#34229,2.54);
#1055=CYLINDRICAL_SURFACE('',#34234,11.5);
#1056=CYLINDRICAL_SURFACE('',#34236,2.54);
#1057=CYLINDRICAL_SURFACE('',#34242,11.5);
#1058=CYLINDRICAL_SURFACE('',#34245,2.54);
#1059=CYLINDRICAL_SURFACE('',#34251,2.54);
#1060=CYLINDRICAL_SURFACE('',#34255,2.54);
#1061=CYLINDRICAL_SURFACE('',#34259,2.54);
#1062=CYLINDRICAL_SURFACE('',#34264,2.54);
#1063=CYLINDRICAL_SURFACE('',#34266,2.54);
#1064=CYLINDRICAL_SURFACE('',#34271,2.54);
#1065=CYLINDRICAL_SURFACE('',#34275,2.54);
#1066=CYLINDRICAL_SURFACE('',#34280,2.54);
#1067=CYLINDRICAL_SURFACE('',#34285,2.54);
#1068=CYLINDRICAL_SURFACE('',#34287,2.54);
#1069=CYLINDRICAL_SURFACE('',#34291,2.54);
#1070=CYLINDRICAL_SURFACE('',#34294,11.5);
#1071=CYLINDRICAL_SURFACE('',#34299,2.54);
#1072=CYLINDRICAL_SURFACE('',#34302,2.54);
#1073=CYLINDRICAL_SURFACE('',#34307,2.54);
#1074=CYLINDRICAL_SURFACE('',#34313,2.54);
#1075=CYLINDRICAL_SURFACE('',#34318,2.54);
#1076=CYLINDRICAL_SURFACE('',#34319,2.54);
#1077=CYLINDRICAL_SURFACE('',#34325,2.54);
#1078=CYLINDRICAL_SURFACE('',#34327,2.54);
#1079=CYLINDRICAL_SURFACE('',#34330,2.54);
#1080=CYLINDRICAL_SURFACE('',#34338,2.54);
#1081=CYLINDRICAL_SURFACE('',#34341,2.54);
#1082=CYLINDRICAL_SURFACE('',#34353,35.75);
#1083=CYLINDRICAL_SURFACE('',#34357,27.315);
#1084=CYLINDRICAL_SURFACE('',#34361,23.435);
#1085=CYLINDRICAL_SURFACE('',#34365,15.);
#1086=CYLINDRICAL_SURFACE('',#34369,23.435);
#1087=CYLINDRICAL_SURFACE('',#34373,27.315);
#1088=CYLINDRICAL_SURFACE('',#34377,35.75);
#1089=CYLINDRICAL_SURFACE('',#34384,11.5);
#1090=CYLINDRICAL_SURFACE('',#34386,11.5);
#1091=CYLINDRICAL_SURFACE('',#34388,11.5);
#1092=CYLINDRICAL_SURFACE('',#34390,11.5);
#1093=CYLINDRICAL_SURFACE('',#34398,6.);
#1094=CYLINDRICAL_SURFACE('',#34412,9.);
#1095=CYLINDRICAL_SURFACE('',#34426,5.);
#1096=CYLINDRICAL_SURFACE('',#34440,8.);
#1097=CYLINDRICAL_SURFACE('',#34454,5.);
#1098=CYLINDRICAL_SURFACE('',#34468,8.);
#1099=CYLINDRICAL_SURFACE('',#34482,5.);
#1100=CYLINDRICAL_SURFACE('',#34511,7.3);
#1101=CYLINDRICAL_SURFACE('',#34529,4.);
#1102=CYLINDRICAL_SURFACE('',#34532,4.);
#1103=CYLINDRICAL_SURFACE('',#34535,4.);
#1104=CYLINDRICAL_SURFACE('',#34538,4.);
#1105=CYLINDRICAL_SURFACE('',#34541,4.);
#1106=CYLINDRICAL_SURFACE('',#34544,4.);
#1107=CYLINDRICAL_SURFACE('',#34576,4.08939999999975);
#1108=CYLINDRICAL_SURFACE('',#34577,84.4550000000046);
#1109=CYLINDRICAL_SURFACE('',#34582,2.286);
#1110=CYLINDRICAL_SURFACE('',#34583,2.286);
#1111=CYLINDRICAL_SURFACE('',#34584,4.82600000000001);
#1112=CYLINDRICAL_SURFACE('',#34587,4.08939999999991);
#1113=CYLINDRICAL_SURFACE('',#34590,84.455000000012);
#1114=CYLINDRICAL_SURFACE('',#34615,4.08939999999986);
#1115=CYLINDRICAL_SURFACE('',#34617,4.08939999999985);
#1116=CYLINDRICAL_SURFACE('',#34647,4.82600000000001);
#1117=CYLINDRICAL_SURFACE('',#34648,4.826);
#1118=CYLINDRICAL_SURFACE('',#34652,4.82599999999999);
#1119=CYLINDRICAL_SURFACE('',#34656,4.82600000000005);
#1120=CYLINDRICAL_SURFACE('',#34660,4.82600000000005);
#1121=CYLINDRICAL_SURFACE('',#34672,3.04799999999982);
#1122=CYLINDRICAL_SURFACE('',#34675,3.04799999999992);
#1123=CYLINDRICAL_SURFACE('',#34678,3.048);
#1124=CYLINDRICAL_SURFACE('',#34681,3.04800000000001);
#1125=CYLINDRICAL_SURFACE('',#34699,4.08940000000001);
#1126=CYLINDRICAL_SURFACE('',#34714,4.0894);
#1127=CYLINDRICAL_SURFACE('',#34751,4.826);
#1128=CYLINDRICAL_SURFACE('',#34757,4.826);
#1129=CYLINDRICAL_SURFACE('',#34781,11.1759999999998);
#1130=CYLINDRICAL_SURFACE('',#34811,4.12749999999997);
#1131=CYLINDRICAL_SURFACE('',#34817,4.12750000000001);
#1132=CYLINDRICAL_SURFACE('',#34823,4.12749999999996);
#1133=CYLINDRICAL_SURFACE('',#34836,90.9319999999999);
#1134=CYLINDRICAL_SURFACE('',#34840,82.931);
#1135=CYLINDRICAL_SURFACE('',#34855,5.08000000000016);
#1136=CYLINDRICAL_SURFACE('',#34858,5.08000000000021);
#1137=CYLINDRICAL_SURFACE('',#34866,5.08);
#1138=CYLINDRICAL_SURFACE('',#34869,5.08000000000001);
#1139=CYLINDRICAL_SURFACE('',#34874,3.90270999999991);
#1140=CYLINDRICAL_SURFACE('',#34881,3.90270999999999);
#1141=CYLINDRICAL_SURFACE('',#34888,3.90271000000012);
#1142=CYLINDRICAL_SURFACE('',#34895,3.90271);
#1143=CYLINDRICAL_SURFACE('',#34908,57.15);
#1144=CYLINDRICAL_SURFACE('',#34912,52.451);
#1145=CYLINDRICAL_SURFACE('',#34916,13.081);
#1146=CYLINDRICAL_SURFACE('',#34920,12.446);
#1147=CYLINDRICAL_SURFACE('',#34924,8.76299999999995);
#1148=CYLINDRICAL_SURFACE('',#34925,2.794);
#1149=CYLINDRICAL_SURFACE('',#34928,8.76299999999997);
#1150=CYLINDRICAL_SURFACE('',#34932,2.794);
#1151=CYLINDRICAL_SURFACE('',#34937,2.79400000000002);
#1152=CYLINDRICAL_SURFACE('',#34941,8.76300000000001);
#1153=CYLINDRICAL_SURFACE('',#34942,8.763);
#1154=CYLINDRICAL_SURFACE('',#34946,2.79399999999998);
#1155=CYLINDRICAL_SURFACE('',#34950,2.76860000000046);
#1156=CYLINDRICAL_SURFACE('',#34958,2.7686);
#1157=CYLINDRICAL_SURFACE('',#34960,2.76860000000001);
#1158=CYLINDRICAL_SURFACE('',#34961,2.76860000000061);
#1159=CYLINDRICAL_SURFACE('',#34965,4.73709999999997);
#1160=CYLINDRICAL_SURFACE('',#34968,2.18439999999999);
#1161=CYLINDRICAL_SURFACE('',#34989,2.18440000000006);
#1162=CYLINDRICAL_SURFACE('',#34990,4.73710000000002);
#1163=CYLINDRICAL_SURFACE('',#35041,0.5);
#1164=CYLINDRICAL_SURFACE('',#35049,0.5);
#1165=CYLINDRICAL_SURFACE('',#35054,0.5);
#1166=CYLINDRICAL_SURFACE('',#35065,0.5);
#1167=CYLINDRICAL_SURFACE('',#35109,0.5);
#1168=CYLINDRICAL_SURFACE('',#35110,0.5);
#1169=CYLINDRICAL_SURFACE('',#35116,0.5);
#1170=CYLINDRICAL_SURFACE('',#35117,0.5);
#1171=CYLINDRICAL_SURFACE('',#35122,0.5);
#1172=CYLINDRICAL_SURFACE('',#35124,0.5);
#1173=CYLINDRICAL_SURFACE('',#35125,0.5);
#1174=CYLINDRICAL_SURFACE('',#35126,0.5);
#1175=CYLINDRICAL_SURFACE('',#35127,0.5);
#1176=CYLINDRICAL_SURFACE('',#35128,0.5);
#1177=CYLINDRICAL_SURFACE('',#35129,0.5);
#1178=CYLINDRICAL_SURFACE('',#35130,0.5);
#1179=CYLINDRICAL_SURFACE('',#35131,0.5);
#1180=CYLINDRICAL_SURFACE('',#35132,0.5);
#1181=CYLINDRICAL_SURFACE('',#35133,0.5);
#1182=CYLINDRICAL_SURFACE('',#35134,0.5);
#1183=CYLINDRICAL_SURFACE('',#35135,0.5);
#1184=CYLINDRICAL_SURFACE('',#35136,0.5);
#1185=CYLINDRICAL_SURFACE('',#35137,0.5);
#1186=CYLINDRICAL_SURFACE('',#35138,0.5);
#1187=CYLINDRICAL_SURFACE('',#35154,5.188);
#1188=CYLINDRICAL_SURFACE('',#35159,5.188);
#1189=CYLINDRICAL_SURFACE('',#35164,5.188);
#1190=CYLINDRICAL_SURFACE('',#35169,5.188);
#1191=CYLINDRICAL_SURFACE('',#35193,2.);
#1192=CYLINDRICAL_SURFACE('',#35197,2.);
#1193=CYLINDRICAL_SURFACE('',#35201,4.);
#1194=CYLINDRICAL_SURFACE('',#35205,4.);
#1195=CYLINDRICAL_SURFACE('',#35209,2.);
#1196=CYLINDRICAL_SURFACE('',#35213,2.);
#1197=CYLINDRICAL_SURFACE('',#35217,4.);
#1198=CYLINDRICAL_SURFACE('',#35221,4.);
#1199=CYLINDRICAL_SURFACE('',#35227,2.);
#1200=CYLINDRICAL_SURFACE('',#35231,2.);
#1201=CYLINDRICAL_SURFACE('',#35235,4.);
#1202=CYLINDRICAL_SURFACE('',#35239,4.);
#1203=CYLINDRICAL_SURFACE('',#35243,2.);
#1204=CYLINDRICAL_SURFACE('',#35247,2.);
#1205=CYLINDRICAL_SURFACE('',#35251,4.);
#1206=CYLINDRICAL_SURFACE('',#35255,4.);
#1207=CYLINDRICAL_SURFACE('',#35261,2.);
#1208=CYLINDRICAL_SURFACE('',#35265,2.);
#1209=CYLINDRICAL_SURFACE('',#35269,4.);
#1210=CYLINDRICAL_SURFACE('',#35273,4.);
#1211=CYLINDRICAL_SURFACE('',#35277,2.);
#1212=CYLINDRICAL_SURFACE('',#35281,2.);
#1213=CYLINDRICAL_SURFACE('',#35285,4.);
#1214=CYLINDRICAL_SURFACE('',#35289,4.);
#1215=CYLINDRICAL_SURFACE('',#35295,2.);
#1216=CYLINDRICAL_SURFACE('',#35299,2.);
#1217=CYLINDRICAL_SURFACE('',#35303,4.);
#1218=CYLINDRICAL_SURFACE('',#35307,4.);
#1219=CYLINDRICAL_SURFACE('',#35311,2.);
#1220=CYLINDRICAL_SURFACE('',#35315,2.);
#1221=CYLINDRICAL_SURFACE('',#35319,4.);
#1222=CYLINDRICAL_SURFACE('',#35323,4.);
#1223=CYLINDRICAL_SURFACE('',#35338,2.);
#1224=CYLINDRICAL_SURFACE('',#35341,2.);
#1225=CYLINDRICAL_SURFACE('',#35343,4.);
#1226=CYLINDRICAL_SURFACE('',#35345,4.);
#1227=CYLINDRICAL_SURFACE('',#35354,4.);
#1228=CYLINDRICAL_SURFACE('',#35355,2.);
#1229=CYLINDRICAL_SURFACE('',#35357,2.);
#1230=CYLINDRICAL_SURFACE('',#35360,4.);
#1231=CYLINDRICAL_SURFACE('',#35372,2.);
#1232=CYLINDRICAL_SURFACE('',#35375,2.);
#1233=CYLINDRICAL_SURFACE('',#35377,4.);
#1234=CYLINDRICAL_SURFACE('',#35380,4.);
#1235=CYLINDRICAL_SURFACE('',#35389,4.);
#1236=CYLINDRICAL_SURFACE('',#35390,2.);
#1237=CYLINDRICAL_SURFACE('',#35392,2.);
#1238=CYLINDRICAL_SURFACE('',#35394,4.);
#1239=CYLINDRICAL_SURFACE('',#35406,2.);
#1240=CYLINDRICAL_SURFACE('',#35409,2.);
#1241=CYLINDRICAL_SURFACE('',#35412,4.);
#1242=CYLINDRICAL_SURFACE('',#35415,4.);
#1243=CYLINDRICAL_SURFACE('',#35424,2.);
#1244=CYLINDRICAL_SURFACE('',#35426,2.);
#1245=CYLINDRICAL_SURFACE('',#35427,4.);
#1246=CYLINDRICAL_SURFACE('',#35429,4.);
#1247=CYLINDRICAL_SURFACE('',#35440,2.);
#1248=CYLINDRICAL_SURFACE('',#35443,2.);
#1249=CYLINDRICAL_SURFACE('',#35446,4.);
#1250=CYLINDRICAL_SURFACE('',#35449,4.);
#1251=CYLINDRICAL_SURFACE('',#35458,2.);
#1252=CYLINDRICAL_SURFACE('',#35460,2.);
#1253=CYLINDRICAL_SURFACE('',#35461,4.);
#1254=CYLINDRICAL_SURFACE('',#35463,4.);
#1255=CYLINDRICAL_SURFACE('',#35465,2.);
#1256=CYLINDRICAL_SURFACE('',#35469,2.);
#1257=CYLINDRICAL_SURFACE('',#35473,4.);
#1258=CYLINDRICAL_SURFACE('',#35477,4.);
#1259=CYLINDRICAL_SURFACE('',#35481,2.);
#1260=CYLINDRICAL_SURFACE('',#35485,2.);
#1261=CYLINDRICAL_SURFACE('',#35489,4.);
#1262=CYLINDRICAL_SURFACE('',#35493,4.);
#1263=CYLINDRICAL_SURFACE('',#35499,2.);
#1264=CYLINDRICAL_SURFACE('',#35503,2.);
#1265=CYLINDRICAL_SURFACE('',#35507,4.);
#1266=CYLINDRICAL_SURFACE('',#35511,4.);
#1267=CYLINDRICAL_SURFACE('',#35515,2.);
#1268=CYLINDRICAL_SURFACE('',#35519,2.);
#1269=CYLINDRICAL_SURFACE('',#35523,4.);
#1270=CYLINDRICAL_SURFACE('',#35527,4.);
#1271=CYLINDRICAL_SURFACE('',#35533,2.);
#1272=CYLINDRICAL_SURFACE('',#35537,2.);
#1273=CYLINDRICAL_SURFACE('',#35541,4.);
#1274=CYLINDRICAL_SURFACE('',#35545,4.);
#1275=CYLINDRICAL_SURFACE('',#35549,2.);
#1276=CYLINDRICAL_SURFACE('',#35553,2.);
#1277=CYLINDRICAL_SURFACE('',#35557,4.);
#1278=CYLINDRICAL_SURFACE('',#35561,4.);
#1279=CYLINDRICAL_SURFACE('',#35566,4.);
#1280=CYLINDRICAL_SURFACE('',#35570,4.);
#1281=CYLINDRICAL_SURFACE('',#35574,4.);
#1282=CYLINDRICAL_SURFACE('',#35578,4.);
#1283=CYLINDRICAL_SURFACE('',#35582,24.0000000000018);
#1284=CYLINDRICAL_SURFACE('',#35586,24.0000000000018);
#1285=CYLINDRICAL_SURFACE('',#35590,24.0000000000018);
#1286=CYLINDRICAL_SURFACE('',#35594,24.0000000000018);
#1287=CYLINDRICAL_SURFACE('',#35600,4.);
#1288=CYLINDRICAL_SURFACE('',#35604,4.);
#1289=CYLINDRICAL_SURFACE('',#35608,4.);
#1290=CYLINDRICAL_SURFACE('',#35612,4.);
#1291=CYLINDRICAL_SURFACE('',#35616,24.0000000000018);
#1292=CYLINDRICAL_SURFACE('',#35620,24.0000000000018);
#1293=CYLINDRICAL_SURFACE('',#35624,24.0000000000018);
#1294=CYLINDRICAL_SURFACE('',#35628,24.0000000000018);
#1295=CYLINDRICAL_SURFACE('',#35634,4.);
#1296=CYLINDRICAL_SURFACE('',#35638,4.);
#1297=CYLINDRICAL_SURFACE('',#35642,4.);
#1298=CYLINDRICAL_SURFACE('',#35646,4.);
#1299=CYLINDRICAL_SURFACE('',#35650,24.0000000000018);
#1300=CYLINDRICAL_SURFACE('',#35654,24.0000000000018);
#1301=CYLINDRICAL_SURFACE('',#35658,24.0000000000018);
#1302=CYLINDRICAL_SURFACE('',#35662,24.0000000000018);
#1303=CYLINDRICAL_SURFACE('',#35668,4.);
#1304=CYLINDRICAL_SURFACE('',#35672,4.);
#1305=CYLINDRICAL_SURFACE('',#35676,4.);
#1306=CYLINDRICAL_SURFACE('',#35680,4.);
#1307=CYLINDRICAL_SURFACE('',#35684,24.0000000000018);
#1308=CYLINDRICAL_SURFACE('',#35688,24.0000000000018);
#1309=CYLINDRICAL_SURFACE('',#35692,24.0000000000018);
#1310=CYLINDRICAL_SURFACE('',#35696,24.0000000000018);
#1311=CYLINDRICAL_SURFACE('',#35704,5.053);
#1312=CYLINDRICAL_SURFACE('',#35707,5.053);
#1313=CYLINDRICAL_SURFACE('',#35710,5.053);
#1314=CYLINDRICAL_SURFACE('',#35713,5.053);
#1315=CYLINDRICAL_SURFACE('',#35716,5.053);
#1316=CYLINDRICAL_SURFACE('',#35719,5.053);
#1317=CYLINDRICAL_SURFACE('',#35722,5.053);
#1318=CYLINDRICAL_SURFACE('',#35725,5.053);
#1319=CYLINDRICAL_SURFACE('',#35728,5.053);
#1320=CYLINDRICAL_SURFACE('',#35731,5.053);
#1321=CYLINDRICAL_SURFACE('',#35734,5.053);
#1322=CYLINDRICAL_SURFACE('',#35737,5.053);
#1323=CYLINDRICAL_SURFACE('',#35740,5.053);
#1324=CYLINDRICAL_SURFACE('',#35743,5.053);
#1325=CYLINDRICAL_SURFACE('',#35746,5.053);
#1326=CYLINDRICAL_SURFACE('',#35749,5.053);
#1327=CYLINDRICAL_SURFACE('',#35774,4.188);
#1328=CYLINDRICAL_SURFACE('',#35777,4.188);
#1329=CYLINDRICAL_SURFACE('',#35780,4.188);
#1330=CYLINDRICAL_SURFACE('',#35783,4.188);
#1331=CYLINDRICAL_SURFACE('',#35786,4.188);
#1332=CYLINDRICAL_SURFACE('',#35789,4.188);
#1333=CYLINDRICAL_SURFACE('',#35790,5.188);
#1334=CYLINDRICAL_SURFACE('',#35793,5.188);
#1335=CYLINDRICAL_SURFACE('',#35796,5.188);
#1336=CYLINDRICAL_SURFACE('',#35799,5.188);
#1337=CYLINDRICAL_SURFACE('',#35802,5.188);
#1338=CYLINDRICAL_SURFACE('',#35805,5.188);
#1339=CYLINDRICAL_SURFACE('',#35808,5.188);
#1340=CYLINDRICAL_SURFACE('',#35811,5.188);
#1341=CYLINDRICAL_SURFACE('',#35814,20.);
#1342=CYLINDRICAL_SURFACE('',#35817,20.);
#1343=CYLINDRICAL_SURFACE('',#35835,4.188);
#1344=CYLINDRICAL_SURFACE('',#35838,4.188);
#1345=CYLINDRICAL_SURFACE('',#35841,4.188);
#1346=CYLINDRICAL_SURFACE('',#35844,4.188);
#1347=CYLINDRICAL_SURFACE('',#35847,4.188);
#1348=CYLINDRICAL_SURFACE('',#35850,4.188);
#1349=CYLINDRICAL_SURFACE('',#35851,5.188);
#1350=CYLINDRICAL_SURFACE('',#35854,5.188);
#1351=CYLINDRICAL_SURFACE('',#35857,5.188);
#1352=CYLINDRICAL_SURFACE('',#35860,5.188);
#1353=CYLINDRICAL_SURFACE('',#35863,5.188);
#1354=CYLINDRICAL_SURFACE('',#35866,5.188);
#1355=CYLINDRICAL_SURFACE('',#35869,5.188);
#1356=CYLINDRICAL_SURFACE('',#35872,5.188);
#1357=CYLINDRICAL_SURFACE('',#35875,20.);
#1358=CYLINDRICAL_SURFACE('',#35878,20.);
#1359=CYLINDRICAL_SURFACE('',#35885,5.5);
#1360=CYLINDRICAL_SURFACE('',#35888,5.5);
#1361=CYLINDRICAL_SURFACE('',#35891,5.5);
#1362=CYLINDRICAL_SURFACE('',#35894,5.5);
#1363=CYLINDRICAL_SURFACE('',#35897,5.5);
#1364=CYLINDRICAL_SURFACE('',#35900,5.5);
#1365=CYLINDRICAL_SURFACE('',#35914,31.);
#1366=CYLINDRICAL_SURFACE('',#35923,7.);
#1367=CYLINDRICAL_SURFACE('',#35926,7.);
#1368=CYLINDRICAL_SURFACE('',#35929,7.);
#1369=CYLINDRICAL_SURFACE('',#35932,7.);
#1370=CYLINDRICAL_SURFACE('',#35963,20.);
#1371=CYLINDRICAL_SURFACE('',#35966,5.99999999999999);
#1372=CYLINDRICAL_SURFACE('',#35970,6.00000000000001);
#1373=CYLINDRICAL_SURFACE('',#35980,15.);
#1374=CYLINDRICAL_SURFACE('',#35989,15.);
#1375=CYLINDRICAL_SURFACE('',#35995,18.5);
#1376=CYLINDRICAL_SURFACE('',#36001,18.5);
#1377=CYLINDRICAL_SURFACE('',#36007,6.);
#1378=CYLINDRICAL_SURFACE('',#36011,6.);
#1379=CYLINDRICAL_SURFACE('',#36014,20.);
#1380=CYLINDRICAL_SURFACE('',#36033,20.);
#1381=CYLINDRICAL_SURFACE('',#36040,12.5);
#1382=CYLINDRICAL_SURFACE('',#36047,15.);
#1383=CYLINDRICAL_SURFACE('',#36052,5.99999999999999);
#1384=CYLINDRICAL_SURFACE('',#36055,6.00000000000001);
#1385=CYLINDRICAL_SURFACE('',#36064,18.5);
#1386=CYLINDRICAL_SURFACE('',#36071,15.);
#1387=CYLINDRICAL_SURFACE('',#36082,18.5);
#1388=CYLINDRICAL_SURFACE('',#36088,6.);
#1389=CYLINDRICAL_SURFACE('',#36092,6.);
#1390=CYLINDRICAL_SURFACE('',#36095,20.);
#1391=CYLINDRICAL_SURFACE('',#36117,20.);
#1392=CYLINDRICAL_SURFACE('',#36119,30.);
#1393=CYLINDRICAL_SURFACE('',#36123,18.5);
#1394=CYLINDRICAL_SURFACE('',#36126,33.);
#1395=CYLINDRICAL_SURFACE('',#36154,30.);
#1396=CYLINDRICAL_SURFACE('',#36356,15.);
#1397=CYLINDRICAL_SURFACE('',#36359,59.00430282);
#1398=CYLINDRICAL_SURFACE('',#36361,28.3018268963564);
#1399=CYLINDRICAL_SURFACE('',#36363,28.3018268963564);
#1400=CYLINDRICAL_SURFACE('',#36365,59.00430282);
#1401=CYLINDRICAL_SURFACE('',#36367,28.3018268963564);
#1402=CYLINDRICAL_SURFACE('',#36369,28.3018268963564);
#1403=CYLINDRICAL_SURFACE('',#36371,59.00430282);
#1404=CYLINDRICAL_SURFACE('',#36373,28.3018268963564);
#1405=CYLINDRICAL_SURFACE('',#36375,28.3018268963564);
#1406=CYLINDRICAL_SURFACE('',#36377,59.00430282);
#1407=CYLINDRICAL_SURFACE('',#36379,28.3018268963564);
#1408=CYLINDRICAL_SURFACE('',#36381,28.3018268963564);
#1409=CYLINDRICAL_SURFACE('',#36383,59.00430282);
#1410=CYLINDRICAL_SURFACE('',#36385,28.3018268963564);
#1411=CYLINDRICAL_SURFACE('',#36387,28.3018268963564);
#1412=CYLINDRICAL_SURFACE('',#36389,59.00430282);
#1413=CYLINDRICAL_SURFACE('',#36391,28.3018268963564);
#1414=CYLINDRICAL_SURFACE('',#36393,28.3018268963564);
#1415=CYLINDRICAL_SURFACE('',#36395,59.00430282);
#1416=CYLINDRICAL_SURFACE('',#36397,28.3018268963564);
#1417=CYLINDRICAL_SURFACE('',#36399,28.3018268963564);
#1418=CYLINDRICAL_SURFACE('',#36401,59.00430282);
#1419=CYLINDRICAL_SURFACE('',#36403,28.3018268963564);
#1420=CYLINDRICAL_SURFACE('',#36405,28.3018268963564);
#1421=CYLINDRICAL_SURFACE('',#36407,59.00430282);
#1422=CYLINDRICAL_SURFACE('',#36409,28.3018268963564);
#1423=CYLINDRICAL_SURFACE('',#36411,28.3018268963564);
#1424=CYLINDRICAL_SURFACE('',#36413,59.00430282);
#1425=CYLINDRICAL_SURFACE('',#36415,28.3018268963564);
#1426=CYLINDRICAL_SURFACE('',#36417,28.3018268963564);
#1427=CYLINDRICAL_SURFACE('',#36419,59.00430282);
#1428=CYLINDRICAL_SURFACE('',#36421,28.3018268963564);
#1429=CYLINDRICAL_SURFACE('',#36423,28.3018268963564);
#1430=CYLINDRICAL_SURFACE('',#36425,59.00430282);
#1431=CYLINDRICAL_SURFACE('',#36427,28.3018268963564);
#1432=CYLINDRICAL_SURFACE('',#36429,28.3018268963564);
#1433=CYLINDRICAL_SURFACE('',#36431,59.00430282);
#1434=CYLINDRICAL_SURFACE('',#36433,28.3018268963564);
#1435=CYLINDRICAL_SURFACE('',#36435,28.3018268963564);
#1436=CYLINDRICAL_SURFACE('',#36437,59.00430282);
#1437=CYLINDRICAL_SURFACE('',#36439,28.3018268963564);
#1438=CYLINDRICAL_SURFACE('',#36441,28.3018268963564);
#1439=CYLINDRICAL_SURFACE('',#36443,59.00430282);
#1440=CYLINDRICAL_SURFACE('',#36445,28.3018268963564);
#1441=CYLINDRICAL_SURFACE('',#36447,28.3018268963564);
#1442=CYLINDRICAL_SURFACE('',#36449,59.00430282);
#1443=CYLINDRICAL_SURFACE('',#36451,28.3018268963564);
#1444=CYLINDRICAL_SURFACE('',#36453,28.3018268963564);
#1445=CYLINDRICAL_SURFACE('',#36455,59.00430282);
#1446=CYLINDRICAL_SURFACE('',#36457,28.3018268963564);
#1447=CYLINDRICAL_SURFACE('',#36459,28.3018268963564);
#1448=CYLINDRICAL_SURFACE('',#36461,59.00430282);
#1449=CYLINDRICAL_SURFACE('',#36463,28.3018268963564);
#1450=CYLINDRICAL_SURFACE('',#36465,28.3018268963564);
#1451=CYLINDRICAL_SURFACE('',#36467,59.00430282);
#1452=CYLINDRICAL_SURFACE('',#36469,28.3018268963564);
#1453=CYLINDRICAL_SURFACE('',#36471,28.3018268963564);
#1454=CYLINDRICAL_SURFACE('',#36473,59.00430282);
#1455=CYLINDRICAL_SURFACE('',#36475,28.3018268963564);
#1456=CYLINDRICAL_SURFACE('',#36477,28.3018268963564);
#1457=CYLINDRICAL_SURFACE('',#36479,59.00430282);
#1458=CYLINDRICAL_SURFACE('',#36481,28.3018268963564);
#1459=CYLINDRICAL_SURFACE('',#36483,28.3018268963564);
#1460=CYLINDRICAL_SURFACE('',#36485,59.00430282);
#1461=CYLINDRICAL_SURFACE('',#36487,28.3018268963564);
#1462=CYLINDRICAL_SURFACE('',#36489,28.3018268963564);
#1463=CYLINDRICAL_SURFACE('',#36491,59.00430282);
#1464=CYLINDRICAL_SURFACE('',#36493,28.3018268963564);
#1465=CYLINDRICAL_SURFACE('',#36495,28.3018268963564);
#1466=CYLINDRICAL_SURFACE('',#36497,59.00430282);
#1467=CYLINDRICAL_SURFACE('',#36499,28.3018268963564);
#1468=CYLINDRICAL_SURFACE('',#36501,28.3018268963564);
#1469=CYLINDRICAL_SURFACE('',#36503,59.00430282);
#1470=CYLINDRICAL_SURFACE('',#36505,28.3018268963564);
#1471=CYLINDRICAL_SURFACE('',#36507,28.3018268963564);
#1472=CYLINDRICAL_SURFACE('',#36509,59.00430282);
#1473=CYLINDRICAL_SURFACE('',#36511,28.3018268963564);
#1474=CYLINDRICAL_SURFACE('',#36513,28.3018268963564);
#1475=CYLINDRICAL_SURFACE('',#36515,59.00430282);
#1476=CYLINDRICAL_SURFACE('',#36517,28.3018268963564);
#1477=CYLINDRICAL_SURFACE('',#36519,28.3018268963564);
#1478=CYLINDRICAL_SURFACE('',#36521,59.00430282);
#1479=CYLINDRICAL_SURFACE('',#36523,28.3018268963564);
#1480=CYLINDRICAL_SURFACE('',#36525,28.3018268963564);
#1481=CYLINDRICAL_SURFACE('',#36527,59.00430282);
#1482=CYLINDRICAL_SURFACE('',#36529,28.3018268963564);
#1483=CYLINDRICAL_SURFACE('',#36531,28.3018268963564);
#1484=CYLINDRICAL_SURFACE('',#36533,59.00430282);
#1485=CYLINDRICAL_SURFACE('',#36535,28.3018268963564);
#1486=CYLINDRICAL_SURFACE('',#36537,28.3018268963564);
#1487=CYLINDRICAL_SURFACE('',#36539,59.00430282);
#1488=CYLINDRICAL_SURFACE('',#36541,28.3018268963564);
#1489=CYLINDRICAL_SURFACE('',#36543,28.3018268963564);
#1490=CYLINDRICAL_SURFACE('',#36545,59.00430282);
#1491=CYLINDRICAL_SURFACE('',#36547,28.3018268963564);
#1492=CYLINDRICAL_SURFACE('',#36549,28.3018268963564);
#1493=CYLINDRICAL_SURFACE('',#36551,59.00430282);
#1494=CYLINDRICAL_SURFACE('',#36553,28.3018268963564);
#1495=CYLINDRICAL_SURFACE('',#36555,28.3018268963564);
#1496=CYLINDRICAL_SURFACE('',#36557,59.00430282);
#1497=CYLINDRICAL_SURFACE('',#36559,28.3018268963564);
#1498=CYLINDRICAL_SURFACE('',#36561,28.3018268963564);
#1499=CYLINDRICAL_SURFACE('',#36563,59.00430282);
#1500=CYLINDRICAL_SURFACE('',#36565,28.3018268963564);
#1501=CYLINDRICAL_SURFACE('',#36567,28.3018268963564);
#1502=CYLINDRICAL_SURFACE('',#36569,59.00430282);
#1503=CYLINDRICAL_SURFACE('',#36571,28.3018268963564);
#1504=CYLINDRICAL_SURFACE('',#36573,28.3018268963564);
#1505=CYLINDRICAL_SURFACE('',#36575,59.00430282);
#1506=CYLINDRICAL_SURFACE('',#36577,28.3018268963564);
#1507=CYLINDRICAL_SURFACE('',#36579,28.3018268963564);
#1508=CYLINDRICAL_SURFACE('',#36581,59.00430282);
#1509=CYLINDRICAL_SURFACE('',#36583,28.3018268963564);
#1510=CYLINDRICAL_SURFACE('',#36585,28.3018268963564);
#1511=CYLINDRICAL_SURFACE('',#36587,59.00430282);
#1512=CYLINDRICAL_SURFACE('',#36589,28.3018268963564);
#1513=CYLINDRICAL_SURFACE('',#36591,28.3018268963564);
#1514=CYLINDRICAL_SURFACE('',#36593,59.00430282);
#1515=CYLINDRICAL_SURFACE('',#36595,28.3018268963564);
#1516=CYLINDRICAL_SURFACE('',#36597,28.3018268963564);
#1517=CYLINDRICAL_SURFACE('',#36599,59.00430282);
#1518=CYLINDRICAL_SURFACE('',#36601,28.3018268963564);
#1519=CYLINDRICAL_SURFACE('',#36603,28.3018268963564);
#1520=CYLINDRICAL_SURFACE('',#36605,59.00430282);
#1521=CYLINDRICAL_SURFACE('',#36607,28.3018268963564);
#1522=CYLINDRICAL_SURFACE('',#36609,28.3018268963564);
#1523=CYLINDRICAL_SURFACE('',#36611,59.00430282);
#1524=CYLINDRICAL_SURFACE('',#36613,28.3018268963564);
#1525=CYLINDRICAL_SURFACE('',#36615,28.3018268963564);
#1526=CYLINDRICAL_SURFACE('',#36617,59.00430282);
#1527=CYLINDRICAL_SURFACE('',#36619,28.3018268963564);
#1528=CYLINDRICAL_SURFACE('',#36621,28.3018268963564);
#1529=CYLINDRICAL_SURFACE('',#36623,59.00430282);
#1530=CYLINDRICAL_SURFACE('',#36625,28.3018268963564);
#1531=CYLINDRICAL_SURFACE('',#36627,28.3018268963564);
#1532=CYLINDRICAL_SURFACE('',#36629,59.00430282);
#1533=CYLINDRICAL_SURFACE('',#36631,28.3018268963564);
#1534=CYLINDRICAL_SURFACE('',#36633,28.3018268963564);
#1535=CYLINDRICAL_SURFACE('',#36635,59.00430282);
#1536=CYLINDRICAL_SURFACE('',#36637,28.3018268963564);
#1537=CYLINDRICAL_SURFACE('',#36639,28.3018268963564);
#1538=CYLINDRICAL_SURFACE('',#36641,64.5);
#1539=CYLINDRICAL_SURFACE('',#36643,64.5);
#1540=CYLINDRICAL_SURFACE('',#36645,64.5);
#1541=CYLINDRICAL_SURFACE('',#36647,64.5);
#1542=CYLINDRICAL_SURFACE('',#36649,64.5);
#1543=CYLINDRICAL_SURFACE('',#36651,64.5);
#1544=CYLINDRICAL_SURFACE('',#36653,64.5);
#1545=CYLINDRICAL_SURFACE('',#36655,64.5);
#1546=CYLINDRICAL_SURFACE('',#36657,64.5);
#1547=CYLINDRICAL_SURFACE('',#36659,64.5);
#1548=CYLINDRICAL_SURFACE('',#36661,64.5);
#1549=CYLINDRICAL_SURFACE('',#36663,64.5);
#1550=CYLINDRICAL_SURFACE('',#36665,64.5);
#1551=CYLINDRICAL_SURFACE('',#36667,64.5);
#1552=CYLINDRICAL_SURFACE('',#36669,64.5);
#1553=CYLINDRICAL_SURFACE('',#36671,64.5);
#1554=CYLINDRICAL_SURFACE('',#36673,64.5);
#1555=CYLINDRICAL_SURFACE('',#36675,64.5);
#1556=CYLINDRICAL_SURFACE('',#36677,64.5);
#1557=CYLINDRICAL_SURFACE('',#36679,64.5);
#1558=CYLINDRICAL_SURFACE('',#36681,64.5);
#1559=CYLINDRICAL_SURFACE('',#36683,64.5);
#1560=CYLINDRICAL_SURFACE('',#36685,64.5);
#1561=CYLINDRICAL_SURFACE('',#36687,64.5);
#1562=CYLINDRICAL_SURFACE('',#36689,64.5);
#1563=CYLINDRICAL_SURFACE('',#36691,64.5);
#1564=CYLINDRICAL_SURFACE('',#36693,64.5);
#1565=CYLINDRICAL_SURFACE('',#36695,64.5);
#1566=CYLINDRICAL_SURFACE('',#36697,64.5);
#1567=CYLINDRICAL_SURFACE('',#36699,64.5);
#1568=CYLINDRICAL_SURFACE('',#36701,64.5);
#1569=CYLINDRICAL_SURFACE('',#36703,64.5);
#1570=CYLINDRICAL_SURFACE('',#36705,64.5);
#1571=CYLINDRICAL_SURFACE('',#36707,64.5);
#1572=CYLINDRICAL_SURFACE('',#36709,64.5);
#1573=CYLINDRICAL_SURFACE('',#36711,64.5);
#1574=CYLINDRICAL_SURFACE('',#36713,64.5);
#1575=CYLINDRICAL_SURFACE('',#36715,64.5);
#1576=CYLINDRICAL_SURFACE('',#36717,64.5);
#1577=CYLINDRICAL_SURFACE('',#36719,64.5);
#1578=CYLINDRICAL_SURFACE('',#36721,64.5);
#1579=CYLINDRICAL_SURFACE('',#36723,64.5);
#1580=CYLINDRICAL_SURFACE('',#36725,64.5);
#1581=CYLINDRICAL_SURFACE('',#36727,64.5);
#1582=CYLINDRICAL_SURFACE('',#36729,64.5);
#1583=CYLINDRICAL_SURFACE('',#36731,64.5);
#1584=CYLINDRICAL_SURFACE('',#36733,64.5);
#1585=CYLINDRICAL_SURFACE('',#36735,59.00430282);
#1586=CYLINDRICAL_SURFACE('',#36737,28.3018268963564);
#1587=CYLINDRICAL_SURFACE('',#36739,28.3018268963564);
#1588=CYLINDRICAL_SURFACE('',#36741,64.5);
#1589=CYLINDRICAL_SURFACE('',#36750,30.);
#1590=CYLINDRICAL_SURFACE('',#36920,15.);
#1591=CYLINDRICAL_SURFACE('',#36923,46.875);
#1592=CYLINDRICAL_SURFACE('',#36925,27.0484525317045);
#1593=CYLINDRICAL_SURFACE('',#36927,27.0484525317045);
#1594=CYLINDRICAL_SURFACE('',#36929,46.875);
#1595=CYLINDRICAL_SURFACE('',#36931,27.0484525317045);
#1596=CYLINDRICAL_SURFACE('',#36933,27.0484525317045);
#1597=CYLINDRICAL_SURFACE('',#36935,46.875);
#1598=CYLINDRICAL_SURFACE('',#36937,27.0484525317045);
#1599=CYLINDRICAL_SURFACE('',#36939,27.0484525317045);
#1600=CYLINDRICAL_SURFACE('',#36941,46.875);
#1601=CYLINDRICAL_SURFACE('',#36943,27.0484525317045);
#1602=CYLINDRICAL_SURFACE('',#36945,27.0484525317045);
#1603=CYLINDRICAL_SURFACE('',#36947,46.875);
#1604=CYLINDRICAL_SURFACE('',#36949,27.0484525317045);
#1605=CYLINDRICAL_SURFACE('',#36951,27.0484525317045);
#1606=CYLINDRICAL_SURFACE('',#36953,46.875);
#1607=CYLINDRICAL_SURFACE('',#36955,27.0484525317045);
#1608=CYLINDRICAL_SURFACE('',#36957,27.0484525317045);
#1609=CYLINDRICAL_SURFACE('',#36959,46.875);
#1610=CYLINDRICAL_SURFACE('',#36961,27.0484525317045);
#1611=CYLINDRICAL_SURFACE('',#36963,27.0484525317045);
#1612=CYLINDRICAL_SURFACE('',#36965,46.875);
#1613=CYLINDRICAL_SURFACE('',#36967,27.0484525317045);
#1614=CYLINDRICAL_SURFACE('',#36969,27.0484525317045);
#1615=CYLINDRICAL_SURFACE('',#36971,46.875);
#1616=CYLINDRICAL_SURFACE('',#36973,27.0484525317045);
#1617=CYLINDRICAL_SURFACE('',#36975,27.0484525317045);
#1618=CYLINDRICAL_SURFACE('',#36977,46.875);
#1619=CYLINDRICAL_SURFACE('',#36979,27.0484525317045);
#1620=CYLINDRICAL_SURFACE('',#36981,27.0484525317045);
#1621=CYLINDRICAL_SURFACE('',#36983,46.875);
#1622=CYLINDRICAL_SURFACE('',#36985,27.0484525317045);
#1623=CYLINDRICAL_SURFACE('',#36987,27.0484525317045);
#1624=CYLINDRICAL_SURFACE('',#36989,46.875);
#1625=CYLINDRICAL_SURFACE('',#36991,27.0484525317045);
#1626=CYLINDRICAL_SURFACE('',#36993,27.0484525317045);
#1627=CYLINDRICAL_SURFACE('',#36995,46.875);
#1628=CYLINDRICAL_SURFACE('',#36997,27.0484525317045);
#1629=CYLINDRICAL_SURFACE('',#36999,27.0484525317045);
#1630=CYLINDRICAL_SURFACE('',#37001,46.875);
#1631=CYLINDRICAL_SURFACE('',#37003,27.0484525317045);
#1632=CYLINDRICAL_SURFACE('',#37005,27.0484525317045);
#1633=CYLINDRICAL_SURFACE('',#37007,46.875);
#1634=CYLINDRICAL_SURFACE('',#37009,27.0484525317045);
#1635=CYLINDRICAL_SURFACE('',#37011,27.0484525317045);
#1636=CYLINDRICAL_SURFACE('',#37013,46.875);
#1637=CYLINDRICAL_SURFACE('',#37015,27.0484525317045);
#1638=CYLINDRICAL_SURFACE('',#37017,27.0484525317045);
#1639=CYLINDRICAL_SURFACE('',#37019,46.875);
#1640=CYLINDRICAL_SURFACE('',#37021,27.0484525317045);
#1641=CYLINDRICAL_SURFACE('',#37023,27.0484525317045);
#1642=CYLINDRICAL_SURFACE('',#37025,46.875);
#1643=CYLINDRICAL_SURFACE('',#37027,27.0484525317045);
#1644=CYLINDRICAL_SURFACE('',#37029,27.0484525317045);
#1645=CYLINDRICAL_SURFACE('',#37031,46.875);
#1646=CYLINDRICAL_SURFACE('',#37033,27.0484525317045);
#1647=CYLINDRICAL_SURFACE('',#37035,27.0484525317045);
#1648=CYLINDRICAL_SURFACE('',#37037,46.875);
#1649=CYLINDRICAL_SURFACE('',#37039,27.0484525317045);
#1650=CYLINDRICAL_SURFACE('',#37041,27.0484525317045);
#1651=CYLINDRICAL_SURFACE('',#37043,46.875);
#1652=CYLINDRICAL_SURFACE('',#37045,27.0484525317045);
#1653=CYLINDRICAL_SURFACE('',#37047,27.0484525317045);
#1654=CYLINDRICAL_SURFACE('',#37049,46.875);
#1655=CYLINDRICAL_SURFACE('',#37051,27.0484525317045);
#1656=CYLINDRICAL_SURFACE('',#37053,27.0484525317045);
#1657=CYLINDRICAL_SURFACE('',#37055,46.875);
#1658=CYLINDRICAL_SURFACE('',#37057,27.0484525317045);
#1659=CYLINDRICAL_SURFACE('',#37059,27.0484525317045);
#1660=CYLINDRICAL_SURFACE('',#37061,46.875);
#1661=CYLINDRICAL_SURFACE('',#37063,27.0484525317045);
#1662=CYLINDRICAL_SURFACE('',#37065,27.0484525317045);
#1663=CYLINDRICAL_SURFACE('',#37067,46.875);
#1664=CYLINDRICAL_SURFACE('',#37069,27.0484525317045);
#1665=CYLINDRICAL_SURFACE('',#37071,27.0484525317045);
#1666=CYLINDRICAL_SURFACE('',#37073,46.875);
#1667=CYLINDRICAL_SURFACE('',#37075,27.0484525317045);
#1668=CYLINDRICAL_SURFACE('',#37077,27.0484525317045);
#1669=CYLINDRICAL_SURFACE('',#37079,46.875);
#1670=CYLINDRICAL_SURFACE('',#37081,27.0484525317045);
#1671=CYLINDRICAL_SURFACE('',#37083,27.0484525317045);
#1672=CYLINDRICAL_SURFACE('',#37085,46.875);
#1673=CYLINDRICAL_SURFACE('',#37087,27.0484525317045);
#1674=CYLINDRICAL_SURFACE('',#37089,27.0484525317045);
#1675=CYLINDRICAL_SURFACE('',#37091,46.875);
#1676=CYLINDRICAL_SURFACE('',#37093,27.0484525317045);
#1677=CYLINDRICAL_SURFACE('',#37095,27.0484525317045);
#1678=CYLINDRICAL_SURFACE('',#37097,46.875);
#1679=CYLINDRICAL_SURFACE('',#37099,27.0484525317045);
#1680=CYLINDRICAL_SURFACE('',#37101,27.0484525317045);
#1681=CYLINDRICAL_SURFACE('',#37103,46.875);
#1682=CYLINDRICAL_SURFACE('',#37105,27.0484525317045);
#1683=CYLINDRICAL_SURFACE('',#37107,27.0484525317045);
#1684=CYLINDRICAL_SURFACE('',#37109,46.875);
#1685=CYLINDRICAL_SURFACE('',#37111,27.0484525317045);
#1686=CYLINDRICAL_SURFACE('',#37113,27.0484525317045);
#1687=CYLINDRICAL_SURFACE('',#37115,46.875);
#1688=CYLINDRICAL_SURFACE('',#37117,27.0484525317045);
#1689=CYLINDRICAL_SURFACE('',#37119,27.0484525317045);
#1690=CYLINDRICAL_SURFACE('',#37121,46.875);
#1691=CYLINDRICAL_SURFACE('',#37123,27.0484525317045);
#1692=CYLINDRICAL_SURFACE('',#37125,27.0484525317045);
#1693=CYLINDRICAL_SURFACE('',#37127,46.875);
#1694=CYLINDRICAL_SURFACE('',#37129,27.0484525317045);
#1695=CYLINDRICAL_SURFACE('',#37131,27.0484525317045);
#1696=CYLINDRICAL_SURFACE('',#37133,46.875);
#1697=CYLINDRICAL_SURFACE('',#37135,27.0484525317045);
#1698=CYLINDRICAL_SURFACE('',#37137,27.0484525317045);
#1699=CYLINDRICAL_SURFACE('',#37139,46.875);
#1700=CYLINDRICAL_SURFACE('',#37141,27.0484525317045);
#1701=CYLINDRICAL_SURFACE('',#37143,27.0484525317045);
#1702=CYLINDRICAL_SURFACE('',#37145,46.875);
#1703=CYLINDRICAL_SURFACE('',#37147,27.0484525317045);
#1704=CYLINDRICAL_SURFACE('',#37149,27.0484525317045);
#1705=CYLINDRICAL_SURFACE('',#37151,46.875);
#1706=CYLINDRICAL_SURFACE('',#37153,27.0484525317045);
#1707=CYLINDRICAL_SURFACE('',#37155,27.0484525317045);
#1708=CYLINDRICAL_SURFACE('',#37157,52.37069718);
#1709=CYLINDRICAL_SURFACE('',#37159,52.37069718);
#1710=CYLINDRICAL_SURFACE('',#37161,52.37069718);
#1711=CYLINDRICAL_SURFACE('',#37163,52.37069718);
#1712=CYLINDRICAL_SURFACE('',#37165,52.37069718);
#1713=CYLINDRICAL_SURFACE('',#37167,52.37069718);
#1714=CYLINDRICAL_SURFACE('',#37169,52.37069718);
#1715=CYLINDRICAL_SURFACE('',#37171,52.37069718);
#1716=CYLINDRICAL_SURFACE('',#37173,52.37069718);
#1717=CYLINDRICAL_SURFACE('',#37175,52.37069718);
#1718=CYLINDRICAL_SURFACE('',#37177,52.37069718);
#1719=CYLINDRICAL_SURFACE('',#37179,52.37069718);
#1720=CYLINDRICAL_SURFACE('',#37181,52.37069718);
#1721=CYLINDRICAL_SURFACE('',#37183,52.37069718);
#1722=CYLINDRICAL_SURFACE('',#37185,52.37069718);
#1723=CYLINDRICAL_SURFACE('',#37187,52.37069718);
#1724=CYLINDRICAL_SURFACE('',#37189,52.37069718);
#1725=CYLINDRICAL_SURFACE('',#37191,52.37069718);
#1726=CYLINDRICAL_SURFACE('',#37193,52.37069718);
#1727=CYLINDRICAL_SURFACE('',#37195,52.37069718);
#1728=CYLINDRICAL_SURFACE('',#37197,52.37069718);
#1729=CYLINDRICAL_SURFACE('',#37199,52.37069718);
#1730=CYLINDRICAL_SURFACE('',#37201,52.37069718);
#1731=CYLINDRICAL_SURFACE('',#37203,52.37069718);
#1732=CYLINDRICAL_SURFACE('',#37205,52.37069718);
#1733=CYLINDRICAL_SURFACE('',#37207,52.37069718);
#1734=CYLINDRICAL_SURFACE('',#37209,52.37069718);
#1735=CYLINDRICAL_SURFACE('',#37211,52.37069718);
#1736=CYLINDRICAL_SURFACE('',#37213,52.37069718);
#1737=CYLINDRICAL_SURFACE('',#37215,52.37069718);
#1738=CYLINDRICAL_SURFACE('',#37217,52.37069718);
#1739=CYLINDRICAL_SURFACE('',#37219,52.37069718);
#1740=CYLINDRICAL_SURFACE('',#37221,52.37069718);
#1741=CYLINDRICAL_SURFACE('',#37223,52.37069718);
#1742=CYLINDRICAL_SURFACE('',#37225,52.37069718);
#1743=CYLINDRICAL_SURFACE('',#37227,52.37069718);
#1744=CYLINDRICAL_SURFACE('',#37229,52.37069718);
#1745=CYLINDRICAL_SURFACE('',#37231,52.37069718);
#1746=CYLINDRICAL_SURFACE('',#37233,52.37069718);
#1747=CYLINDRICAL_SURFACE('',#37235,46.875);
#1748=CYLINDRICAL_SURFACE('',#37237,27.0484525317045);
#1749=CYLINDRICAL_SURFACE('',#37239,27.0484525317045);
#1750=CYLINDRICAL_SURFACE('',#37241,52.37069718);
#1751=CYLINDRICAL_SURFACE('',#37256,3.22047616000001);
#1752=CYLINDRICAL_SURFACE('',#37257,3.9116);
#1753=CYLINDRICAL_SURFACE('',#37264,4.19099999999999);
#1754=CYLINDRICAL_SURFACE('',#37273,3.22047616000001);
#1755=CYLINDRICAL_SURFACE('',#37274,3.91160000000001);
#1756=CYLINDRICAL_SURFACE('',#37281,4.19099999999999);
#1757=CYLINDRICAL_SURFACE('',#37287,2.74750784000002);
#1758=CYLINDRICAL_SURFACE('',#37291,3.3527999999999);
#1759=CYLINDRICAL_SURFACE('',#37296,3.6322);
#1760=CYLINDRICAL_SURFACE('',#37299,3.9116);
#1761=CYLINDRICAL_SURFACE('',#37304,4.191);
#1762=CYLINDRICAL_SURFACE('',#37312,3.22047616000001);
#1763=CYLINDRICAL_SURFACE('',#37316,3.91160000000001);
#1764=CYLINDRICAL_SURFACE('',#37321,4.19099999999999);
#1765=CYLINDRICAL_SURFACE('',#37329,3.22047616000001);
#1766=CYLINDRICAL_SURFACE('',#37354,4.70822528);
#1767=CYLINDRICAL_SURFACE('',#37364,4.70822528000001);
#1768=CYLINDRICAL_SURFACE('',#37372,4.70822528000003);
#1769=CYLINDRICAL_SURFACE('',#37377,4.70822527999992);
#1770=CYLINDRICAL_SURFACE('',#37385,28.8698432);
#1771=CYLINDRICAL_SURFACE('',#37392,28.8519616);
#1772=CYLINDRICAL_SURFACE('',#37408,4.70822528000001);
#1773=CYLINDRICAL_SURFACE('',#37412,4.70822528);
#1774=CYLINDRICAL_SURFACE('',#37416,4.70822528000001);
#1775=CYLINDRICAL_SURFACE('',#37420,4.70822528000002);
#1776=CYLINDRICAL_SURFACE('',#37432,22.5);
#1777=CYLINDRICAL_SURFACE('',#37519,2.74750784);
#1778=CYLINDRICAL_SURFACE('',#37527,2.74750784000001);
#1779=CYLINDRICAL_SURFACE('',#37535,2.74750784);
#1780=CYLINDRICAL_SURFACE('',#37544,3.2204761600001);
#1781=CYLINDRICAL_SURFACE('',#37552,3.22047616000001);
#1782=CYLINDRICAL_SURFACE('',#37560,3.22047616000007);
#1783=CYLINDRICAL_SURFACE('',#37568,3.22047616000001);
#1784=CYLINDRICAL_SURFACE('',#37592,46.9481408);
#1785=CYLINDRICAL_SURFACE('',#37614,30.1930816);
#1786=CYLINDRICAL_SURFACE('',#37617,67.056);
#1787=CYLINDRICAL_SURFACE('',#37620,46.9481408);
#1788=CYLINDRICAL_SURFACE('',#37630,67.0291776);
#1789=CYLINDRICAL_SURFACE('',#37633,2.74750783999999);
#1790=CYLINDRICAL_SURFACE('',#37647,13.4268464);
#1791=CYLINDRICAL_SURFACE('',#37649,2.74750784);
#1792=CYLINDRICAL_SURFACE('',#37673,3.3528);
#1793=CYLINDRICAL_SURFACE('',#37703,3.35280000000001);
#1794=CYLINDRICAL_SURFACE('',#37714,3.3528);
#1795=CYLINDRICAL_SURFACE('',#37718,2.74750783999998);
#1796=CYLINDRICAL_SURFACE('',#37719,2.74750784000003);
#1797=CYLINDRICAL_SURFACE('',#37723,3.3528);
#1798=CYLINDRICAL_SURFACE('',#37724,37.9894592000001);
#1799=CYLINDRICAL_SURFACE('',#37732,37.9894592000001);
#1800=CYLINDRICAL_SURFACE('',#37738,46.9481408);
#1801=CYLINDRICAL_SURFACE('',#37739,37.9894592000001);
#1802=CYLINDRICAL_SURFACE('',#37744,46.9481408);
#1803=CYLINDRICAL_SURFACE('',#37789,2.74750784);
#1804=CYLINDRICAL_SURFACE('',#37792,2.74750784000001);
#1805=CYLINDRICAL_SURFACE('',#37795,21.82583392);
#1806=CYLINDRICAL_SURFACE('',#37797,3.63219999999997);
#1807=CYLINDRICAL_SURFACE('',#37800,3.63219999999997);
#1808=CYLINDRICAL_SURFACE('',#37803,3.63219999999999);
#1809=CYLINDRICAL_SURFACE('',#37806,3.63219999999999);
#1810=CYLINDRICAL_SURFACE('',#37817,2.14579200000041);
#1811=CYLINDRICAL_SURFACE('',#37820,55.4329599999993);
#1812=CYLINDRICAL_SURFACE('',#37823,2.14579200000012);
#1813=CYLINDRICAL_SURFACE('',#37827,2.14579200000009);
#1814=CYLINDRICAL_SURFACE('',#37830,45.0616320000007);
#1815=CYLINDRICAL_SURFACE('',#37833,2.145792);
#1816=CYLINDRICAL_SURFACE('',#37838,2.14579200000016);
#1817=CYLINDRICAL_SURFACE('',#37841,55.4329600000005);
#1818=CYLINDRICAL_SURFACE('',#37844,2.14579199999963);
#1819=CYLINDRICAL_SURFACE('',#37848,2.14579199999972);
#1820=CYLINDRICAL_SURFACE('',#37851,45.0616320000002);
#1821=CYLINDRICAL_SURFACE('',#37854,2.14579199999999);
#1822=CYLINDRICAL_SURFACE('',#37859,2.14579199999966);
#1823=CYLINDRICAL_SURFACE('',#37862,55.432960000003);
#1824=CYLINDRICAL_SURFACE('',#37865,2.14579200000016);
#1825=CYLINDRICAL_SURFACE('',#37869,2.14579199999998);
#1826=CYLINDRICAL_SURFACE('',#37872,45.0616319999968);
#1827=CYLINDRICAL_SURFACE('',#37875,2.14579199999998);
#1828=CYLINDRICAL_SURFACE('',#37879,3.63219999999999);
#1829=CYLINDRICAL_SURFACE('',#37881,3.63220000000001);
#1830=CYLINDRICAL_SURFACE('',#37883,3.63220000000001);
#1831=CYLINDRICAL_SURFACE('',#37885,40.2514816000001);
#1832=CYLINDRICAL_SURFACE('',#37891,40.251481599999);
#1833=CYLINDRICAL_SURFACE('',#37897,40.2514815999998);
#1834=CYLINDRICAL_SURFACE('',#37942,8.94079999999995);
#1835=CYLINDRICAL_SURFACE('',#37946,8.9408000000001);
#1836=CYLINDRICAL_SURFACE('',#37949,8.94079999999996);
#1837=CYLINDRICAL_SURFACE('',#37952,8.94080000000006);
#1838=CYLINDRICAL_SURFACE('',#37955,40.2514815999993);
#1839=CYLINDRICAL_SURFACE('',#37959,2.14579200000032);
#1840=CYLINDRICAL_SURFACE('',#37963,2.14579199999841);
#1841=CYLINDRICAL_SURFACE('',#37966,45.0616320000031);
#1842=CYLINDRICAL_SURFACE('',#37969,2.14579199999958);
#1843=CYLINDRICAL_SURFACE('',#37973,2.1457920000008);
#1844=CYLINDRICAL_SURFACE('',#37976,55.4329600000096);
#1845=CYLINDRICAL_SURFACE('',#37981,2.14579199999998);
#1846=CYLINDRICAL_SURFACE('',#37984,45.0616319999932);
#1847=CYLINDRICAL_SURFACE('',#37987,2.14579199999989);
#1848=CYLINDRICAL_SURFACE('',#37991,2.14579199999978);
#1849=CYLINDRICAL_SURFACE('',#37994,55.4329600000042);
#1850=CYLINDRICAL_SURFACE('',#37997,2.14579200000232);
#1851=CYLINDRICAL_SURFACE('',#38001,55.4329599999945);
#1852=CYLINDRICAL_SURFACE('',#38004,2.14579199999928);
#1853=CYLINDRICAL_SURFACE('',#38008,2.14579200000044);
#1854=CYLINDRICAL_SURFACE('',#38011,45.0616320000025);
#1855=CYLINDRICAL_SURFACE('',#38014,2.14579200000129);
#1856=CYLINDRICAL_SURFACE('',#38018,2.14579199999758);
#1857=CYLINDRICAL_SURFACE('',#38022,55.4329600000029);
#1858=CYLINDRICAL_SURFACE('',#38025,2.14579199999957);
#1859=CYLINDRICAL_SURFACE('',#38029,2.1457920000006);
#1860=CYLINDRICAL_SURFACE('',#38032,45.0616319999986);
#1861=CYLINDRICAL_SURFACE('',#38035,2.14579199999942);
#1862=CYLINDRICAL_SURFACE('',#38039,2.14579200000082);
#1863=CYLINDRICAL_SURFACE('',#38043,45.0616319999982);
#1864=CYLINDRICAL_SURFACE('',#38045,2.1457920000002);
#1865=CYLINDRICAL_SURFACE('',#38048,2.14579199999973);
#1866=CYLINDRICAL_SURFACE('',#38050,55.4329600000018);
#1867=CYLINDRICAL_SURFACE('',#38052,2.14579199999995);
#1868=CYLINDRICAL_SURFACE('',#38054,2.145792);
#1869=CYLINDRICAL_SURFACE('',#38075,5.02472959999993);
#1870=CYLINDRICAL_SURFACE('',#38088,12.);
#1871=CYLINDRICAL_SURFACE('',#38091,4.26299999999998);
#1872=CYLINDRICAL_SURFACE('',#38092,4.26299999999993);
#1873=CYLINDRICAL_SURFACE('',#38093,3.38975000000002);
#1874=CYLINDRICAL_SURFACE('',#38094,3.38974999999999);
#1875=CYLINDRICAL_SURFACE('',#38097,22.5);
#1876=CYLINDRICAL_SURFACE('',#38099,24.9999999999999);
#1877=CYLINDRICAL_SURFACE('',#38111,35.0000000000001);
#1878=FACE_BOUND('',#6114,.T.);
#1879=FACE_BOUND('',#6132,.T.);
#1880=FACE_BOUND('',#6134,.T.);
#1881=FACE_BOUND('',#6135,.T.);
#1882=FACE_BOUND('',#6136,.T.);
#1883=FACE_BOUND('',#6137,.T.);
#1884=FACE_BOUND('',#6138,.T.);
#1885=FACE_BOUND('',#6143,.T.);
#1886=FACE_BOUND('',#6145,.T.);
#1887=FACE_BOUND('',#6147,.T.);
#1888=FACE_BOUND('',#6149,.T.);
#1889=FACE_BOUND('',#6238,.T.);
#1890=FACE_BOUND('',#6242,.T.);
#1891=FACE_BOUND('',#6245,.T.);
#1892=FACE_BOUND('',#6248,.T.);
#1893=FACE_BOUND('',#6251,.T.);
#1894=FACE_BOUND('',#6254,.T.);
#1895=FACE_BOUND('',#6257,.T.);
#1896=FACE_BOUND('',#6260,.T.);
#1897=FACE_BOUND('',#6272,.T.);
#1898=FACE_BOUND('',#6277,.T.);
#1899=FACE_BOUND('',#6289,.T.);
#1900=FACE_BOUND('',#6294,.T.);
#1901=FACE_BOUND('',#6306,.T.);
#1902=FACE_BOUND('',#6311,.T.);
#1903=FACE_BOUND('',#6323,.T.);
#1904=FACE_BOUND('',#6336,.T.);
#1905=FACE_BOUND('',#6351,.T.);
#1906=FACE_BOUND('',#6357,.T.);
#1907=FACE_BOUND('',#6359,.T.);
#1908=FACE_BOUND('',#6367,.T.);
#1909=FACE_BOUND('',#6368,.T.);
#1910=FACE_BOUND('',#6369,.T.);
#1911=FACE_BOUND('',#6370,.T.);
#1912=FACE_BOUND('',#6371,.T.);
#1913=FACE_BOUND('',#6372,.T.);
#1914=FACE_BOUND('',#6373,.T.);
#1915=FACE_BOUND('',#6389,.T.);
#1916=FACE_BOUND('',#6390,.T.);
#1917=FACE_BOUND('',#6391,.T.);
#1918=FACE_BOUND('',#6392,.T.);
#1919=FACE_BOUND('',#6393,.T.);
#1920=FACE_BOUND('',#6394,.T.);
#1921=FACE_BOUND('',#6395,.T.);
#1922=FACE_BOUND('',#6399,.T.);
#1923=FACE_BOUND('',#6409,.T.);
#1924=FACE_BOUND('',#6410,.T.);
#1925=FACE_BOUND('',#6418,.T.);
#1926=FACE_BOUND('',#6419,.T.);
#1927=FACE_BOUND('',#6422,.T.);
#1928=FACE_BOUND('',#6442,.T.);
#1929=FACE_BOUND('',#6454,.T.);
#1930=FACE_BOUND('',#6456,.T.);
#1931=FACE_BOUND('',#6457,.T.);
#1932=FACE_BOUND('',#6458,.T.);
#1933=FACE_BOUND('',#6469,.T.);
#1934=FACE_BOUND('',#6472,.T.);
#1935=FACE_BOUND('',#6521,.T.);
#1936=FACE_BOUND('',#6539,.T.);
#1937=FACE_BOUND('',#6552,.T.);
#1938=FACE_BOUND('',#6564,.T.);
#1939=FACE_BOUND('',#6565,.T.);
#1940=FACE_BOUND('',#6566,.T.);
#1941=FACE_BOUND('',#6570,.T.);
#1942=FACE_BOUND('',#6577,.T.);
#1943=FACE_BOUND('',#6583,.T.);
#1944=FACE_BOUND('',#6602,.T.);
#1945=FACE_BOUND('',#6603,.T.);
#1946=FACE_BOUND('',#6604,.T.);
#1947=FACE_BOUND('',#6605,.T.);
#1948=FACE_BOUND('',#6606,.T.);
#1949=FACE_BOUND('',#6607,.T.);
#1950=FACE_BOUND('',#6608,.T.);
#1951=FACE_BOUND('',#6609,.T.);
#1952=FACE_BOUND('',#6610,.T.);
#1953=FACE_BOUND('',#6613,.T.);
#1954=FACE_BOUND('',#6616,.T.);
#1955=FACE_BOUND('',#6617,.T.);
#1956=FACE_BOUND('',#6618,.T.);
#1957=FACE_BOUND('',#6621,.T.);
#1958=FACE_BOUND('',#6624,.T.);
#1959=FACE_BOUND('',#6630,.T.);
#1960=FACE_BOUND('',#6636,.T.);
#1961=FACE_BOUND('',#6640,.T.);
#1962=FACE_BOUND('',#6647,.T.);
#1963=FACE_BOUND('',#6652,.T.);
#1964=FACE_BOUND('',#6656,.T.);
#1965=FACE_BOUND('',#6658,.T.);
#1966=FACE_BOUND('',#6660,.T.);
#1967=FACE_BOUND('',#6664,.T.);
#1968=FACE_BOUND('',#6698,.T.);
#1969=FACE_BOUND('',#6699,.T.);
#1970=FACE_BOUND('',#6700,.T.);
#1971=FACE_BOUND('',#6701,.T.);
#1972=FACE_BOUND('',#6702,.T.);
#1973=FACE_BOUND('',#6748,.T.);
#1974=FACE_BOUND('',#6749,.T.);
#1975=FACE_BOUND('',#6750,.T.);
#1976=FACE_BOUND('',#6751,.T.);
#1977=FACE_BOUND('',#6752,.T.);
#1978=FACE_BOUND('',#6801,.T.);
#1979=FACE_BOUND('',#6803,.T.);
#1980=FACE_BOUND('',#6821,.T.);
#1981=FACE_BOUND('',#6823,.T.);
#1982=FACE_BOUND('',#6841,.T.);
#1983=FACE_BOUND('',#6843,.T.);
#1984=FACE_BOUND('',#6861,.T.);
#1985=FACE_BOUND('',#6863,.T.);
#1986=FACE_BOUND('',#6865,.T.);
#1987=FACE_BOUND('',#6874,.T.);
#1988=FACE_BOUND('',#6885,.T.);
#1989=FACE_BOUND('',#6895,.T.);
#1990=FACE_BOUND('',#6905,.T.);
#1991=FACE_BOUND('',#6915,.T.);
#1992=FACE_BOUND('',#6925,.T.);
#1993=FACE_BOUND('',#6935,.T.);
#1994=FACE_BOUND('',#6961,.T.);
#1995=FACE_BOUND('',#6963,.T.);
#1996=FACE_BOUND('',#6981,.T.);
#1997=FACE_BOUND('',#6983,.T.);
#1998=FACE_BOUND('',#7001,.T.);
#1999=FACE_BOUND('',#7003,.T.);
#2000=FACE_BOUND('',#7021,.T.);
#2001=FACE_BOUND('',#7023,.T.);
#2002=FACE_BOUND('',#7041,.T.);
#2003=FACE_BOUND('',#7043,.T.);
#2004=FACE_BOUND('',#7061,.T.);
#2005=FACE_BOUND('',#7063,.T.);
#2006=FACE_BOUND('',#7081,.T.);
#2007=FACE_BOUND('',#7083,.T.);
#2008=FACE_BOUND('',#7101,.T.);
#2009=FACE_BOUND('',#7102,.T.);
#2010=FACE_BOUND('',#7103,.T.);
#2011=FACE_BOUND('',#7104,.T.);
#2012=FACE_BOUND('',#7105,.T.);
#2013=FACE_BOUND('',#7106,.T.);
#2014=FACE_BOUND('',#7107,.T.);
#2015=FACE_BOUND('',#7108,.T.);
#2016=FACE_BOUND('',#7111,.T.);
#2017=FACE_BOUND('',#7112,.T.);
#2018=FACE_BOUND('',#7113,.T.);
#2019=FACE_BOUND('',#7114,.T.);
#2020=FACE_BOUND('',#7115,.T.);
#2021=FACE_BOUND('',#7116,.T.);
#2022=FACE_BOUND('',#7117,.T.);
#2023=FACE_BOUND('',#7118,.T.);
#2024=FACE_BOUND('',#7121,.T.);
#2025=FACE_BOUND('',#7123,.T.);
#2026=FACE_BOUND('',#7124,.T.);
#2027=FACE_BOUND('',#7125,.T.);
#2028=FACE_BOUND('',#7126,.T.);
#2029=FACE_BOUND('',#7127,.T.);
#2030=FACE_BOUND('',#7128,.T.);
#2031=FACE_BOUND('',#7129,.T.);
#2032=FACE_BOUND('',#7130,.T.);
#2033=FACE_BOUND('',#7133,.T.);
#2034=FACE_BOUND('',#7134,.T.);
#2035=FACE_BOUND('',#7135,.T.);
#2036=FACE_BOUND('',#7136,.T.);
#2037=FACE_BOUND('',#7137,.T.);
#2038=FACE_BOUND('',#7138,.T.);
#2039=FACE_BOUND('',#7139,.T.);
#2040=FACE_BOUND('',#7140,.T.);
#2041=FACE_BOUND('',#7143,.T.);
#2042=FACE_BOUND('',#7145,.T.);
#2043=FACE_BOUND('',#7146,.T.);
#2044=FACE_BOUND('',#7147,.T.);
#2045=FACE_BOUND('',#7149,.T.);
#2046=FACE_BOUND('',#7150,.T.);
#2047=FACE_BOUND('',#7151,.T.);
#2048=FACE_BOUND('',#7176,.T.);
#2049=FACE_BOUND('',#7177,.T.);
#2050=FACE_BOUND('',#7178,.T.);
#2051=FACE_BOUND('',#7179,.T.);
#2052=FACE_BOUND('',#7180,.T.);
#2053=FACE_BOUND('',#7181,.T.);
#2054=FACE_BOUND('',#7182,.T.);
#2055=FACE_BOUND('',#7183,.T.);
#2056=FACE_BOUND('',#7184,.T.);
#2057=FACE_BOUND('',#7185,.T.);
#2058=FACE_BOUND('',#7188,.T.);
#2059=FACE_BOUND('',#7189,.T.);
#2060=FACE_BOUND('',#7190,.T.);
#2061=FACE_BOUND('',#7191,.T.);
#2062=FACE_BOUND('',#7192,.T.);
#2063=FACE_BOUND('',#7193,.T.);
#2064=FACE_BOUND('',#7194,.T.);
#2065=FACE_BOUND('',#7195,.T.);
#2066=FACE_BOUND('',#7196,.T.);
#2067=FACE_BOUND('',#7197,.T.);
#2068=FACE_BOUND('',#7199,.T.);
#2069=FACE_BOUND('',#7200,.T.);
#2070=FACE_BOUND('',#7201,.T.);
#2071=FACE_BOUND('',#7203,.T.);
#2072=FACE_BOUND('',#7204,.T.);
#2073=FACE_BOUND('',#7205,.T.);
#2074=FACE_BOUND('',#7230,.T.);
#2075=FACE_BOUND('',#7231,.T.);
#2076=FACE_BOUND('',#7232,.T.);
#2077=FACE_BOUND('',#7233,.T.);
#2078=FACE_BOUND('',#7234,.T.);
#2079=FACE_BOUND('',#7235,.T.);
#2080=FACE_BOUND('',#7236,.T.);
#2081=FACE_BOUND('',#7237,.T.);
#2082=FACE_BOUND('',#7238,.T.);
#2083=FACE_BOUND('',#7239,.T.);
#2084=FACE_BOUND('',#7242,.T.);
#2085=FACE_BOUND('',#7243,.T.);
#2086=FACE_BOUND('',#7244,.T.);
#2087=FACE_BOUND('',#7245,.T.);
#2088=FACE_BOUND('',#7246,.T.);
#2089=FACE_BOUND('',#7247,.T.);
#2090=FACE_BOUND('',#7248,.T.);
#2091=FACE_BOUND('',#7249,.T.);
#2092=FACE_BOUND('',#7250,.T.);
#2093=FACE_BOUND('',#7251,.T.);
#2094=FACE_BOUND('',#7263,.T.);
#2095=FACE_BOUND('',#7264,.T.);
#2096=FACE_BOUND('',#7265,.T.);
#2097=FACE_BOUND('',#7266,.T.);
#2098=FACE_BOUND('',#7267,.T.);
#2099=FACE_BOUND('',#7268,.T.);
#2100=FACE_BOUND('',#7270,.T.);
#2101=FACE_BOUND('',#7271,.T.);
#2102=FACE_BOUND('',#7272,.T.);
#2103=FACE_BOUND('',#7273,.T.);
#2104=FACE_BOUND('',#7274,.T.);
#2105=FACE_BOUND('',#7275,.T.);
#2106=FACE_BOUND('',#7299,.T.);
#2107=FACE_BOUND('',#7300,.T.);
#2108=FACE_BOUND('',#7301,.T.);
#2109=FACE_BOUND('',#7302,.T.);
#2110=FACE_BOUND('',#7303,.T.);
#2111=FACE_BOUND('',#7305,.T.);
#2112=FACE_BOUND('',#7306,.T.);
#2113=FACE_BOUND('',#7307,.T.);
#2114=FACE_BOUND('',#7308,.T.);
#2115=FACE_BOUND('',#7309,.T.);
#2116=FACE_BOUND('',#7318,.T.);
#2117=FACE_BOUND('',#7320,.T.);
#2118=FACE_BOUND('',#7323,.T.);
#2119=FACE_BOUND('',#7341,.T.);
#2120=FACE_BOUND('',#7345,.T.);
#2121=FACE_BOUND('',#7350,.T.);
#2122=FACE_BOUND('',#7355,.T.);
#2123=FACE_BOUND('',#7363,.T.);
#2124=FACE_BOUND('',#7369,.T.);
#2125=FACE_BOUND('',#7382,.T.);
#2126=FACE_BOUND('',#7386,.T.);
#2127=FACE_BOUND('',#7392,.T.);
#2128=FACE_BOUND('',#7396,.T.);
#2129=FACE_BOUND('',#7400,.T.);
#2130=FACE_BOUND('',#7402,.T.);
#2131=FACE_BOUND('',#7406,.T.);
#2132=FACE_BOUND('',#7409,.T.);
#2133=FACE_BOUND('',#7607,.T.);
#2134=FACE_BOUND('',#7611,.T.);
#2135=FACE_BOUND('',#7614,.T.);
#2136=FACE_BOUND('',#7780,.T.);
#2137=FACE_BOUND('',#7787,.T.);
#2138=FACE_BOUND('',#7789,.T.);
#2139=FACE_BOUND('',#7797,.T.);
#2140=FACE_BOUND('',#7799,.T.);
#2141=FACE_BOUND('',#7807,.T.);
#2142=FACE_BOUND('',#7810,.T.);
#2143=FACE_BOUND('',#7813,.T.);
#2144=FACE_BOUND('',#7816,.T.);
#2145=FACE_BOUND('',#7823,.T.);
#2146=FACE_BOUND('',#7826,.T.);
#2147=FACE_BOUND('',#7841,.T.);
#2148=FACE_BOUND('',#7845,.T.);
#2149=FACE_BOUND('',#7846,.T.);
#2150=FACE_BOUND('',#7847,.T.);
#2151=FACE_BOUND('',#7848,.T.);
#2152=FACE_BOUND('',#7868,.T.);
#2153=FACE_BOUND('',#7877,.T.);
#2154=FACE_BOUND('',#7928,.T.);
#2155=FACE_BOUND('',#7938,.T.);
#2156=FACE_BOUND('',#7943,.T.);
#2157=FACE_BOUND('',#7983,.T.);
#2158=FACE_BOUND('',#7985,.T.);
#2159=FACE_BOUND('',#7989,.T.);
#2160=FACE_BOUND('',#7990,.T.);
#2161=FACE_BOUND('',#7991,.T.);
#2162=FACE_BOUND('',#7992,.T.);
#2163=FACE_BOUND('',#8001,.T.);
#2164=FACE_BOUND('',#8002,.T.);
#2165=FACE_BOUND('',#8003,.T.);
#2166=FACE_BOUND('',#8004,.T.);
#2167=FACE_BOUND('',#8005,.T.);
#2168=FACE_BOUND('',#8018,.T.);
#2169=FACE_BOUND('',#8019,.T.);
#2170=FACE_BOUND('',#8020,.T.);
#2171=FACE_BOUND('',#8021,.T.);
#2172=FACE_BOUND('',#8022,.T.);
#2173=FACE_BOUND('',#8024,.T.);
#2174=FACE_BOUND('',#8027,.T.);
#2175=FACE_BOUND('',#8031,.T.);
#2176=FACE_BOUND('',#8034,.T.);
#2177=FACE_BOUND('',#8036,.T.);
#2178=FACE_BOUND('',#8037,.T.);
#2179=FACE_BOUND('',#8040,.T.);
#2180=FACE_BOUND('',#8041,.T.);
#2181=FACE_BOUND('',#8057,.T.);
#2182=FACE_BOUND('',#8063,.T.);
#2183=FACE_BOUND('',#8080,.T.);
#2184=FACE_BOUND('',#8086,.T.);
#2185=FACE_BOUND('',#8097,.T.);
#2186=FACE_BOUND('',#8098,.T.);
#2187=FACE_BOUND('',#8104,.T.);
#2188=FACE_BOUND('',#8105,.T.);
#2189=FACE_BOUND('',#8107,.T.);
#2190=FACE_BOUND('',#8109,.T.);
#2191=FACE_BOUND('',#8113,.T.);
#2192=FACE_BOUND('',#8115,.T.);
#2193=FACE_BOUND('',#8144,.T.);
#2194=FACE_BOUND('',#8146,.T.);
#2195=FACE_BOUND('',#8148,.T.);
#2196=FACE_BOUND('',#8194,.T.);
#2197=FACE_BOUND('',#8196,.T.);
#2198=FACE_BOUND('',#8198,.T.);
#2199=FACE_BOUND('',#8213,.T.);
#2200=FACE_BOUND('',#8227,.T.);
#2201=FACE_BOUND('',#8276,.T.);
#2202=FACE_BOUND('',#8277,.T.);
#2203=FACE_BOUND('',#8278,.T.);
#2204=FACE_BOUND('',#8279,.T.);
#2205=FACE_BOUND('',#8280,.T.);
#2206=FACE_BOUND('',#8281,.T.);
#2207=FACE_BOUND('',#8282,.T.);
#2208=FACE_BOUND('',#8289,.T.);
#2209=FACE_BOUND('',#8290,.T.);
#2210=FACE_BOUND('',#8291,.T.);
#2211=FACE_BOUND('',#8292,.T.);
#2212=FACE_BOUND('',#8293,.T.);
#2213=FACE_BOUND('',#8294,.T.);
#2214=FACE_BOUND('',#8295,.T.);
#2215=FACE_BOUND('',#8296,.T.);
#2216=FACE_BOUND('',#8297,.T.);
#2217=FACE_BOUND('',#8298,.T.);
#2218=FACE_BOUND('',#8299,.T.);
#2219=FACE_BOUND('',#8300,.T.);
#2220=FACE_BOUND('',#8301,.T.);
#2221=FACE_BOUND('',#8302,.T.);
#2222=FACE_BOUND('',#8303,.T.);
#2223=FACE_BOUND('',#8308,.T.);
#2224=FACE_BOUND('',#8320,.T.);
#2225=FACE_BOUND('',#8322,.T.);
#2226=FACE_BOUND('',#8323,.T.);
#2227=FACE_BOUND('',#8329,.T.);
#2228=FACE_BOUND('',#8331,.T.);
#2229=FACE_BOUND('',#8332,.T.);
#2230=FACE_BOUND('',#8334,.T.);
#2231=FACE_BOUND('',#8335,.T.);
#2232=FACE_BOUND('',#8338,.T.);
#2233=FACE_BOUND('',#8341,.T.);
#2234=FACE_BOUND('',#8342,.T.);
#2235=FACE_BOUND('',#8344,.T.);
#2236=CIRCLE('',#34122,5.);
#2237=CIRCLE('',#34123,75.);
#2238=CIRCLE('',#34124,5.);
#2239=CIRCLE('',#34125,75.);
#2240=CIRCLE('',#34126,5.);
#2241=CIRCLE('',#34127,75.);
#2242=CIRCLE('',#34128,20.);
#2243=CIRCLE('',#34130,20.);
#2244=CIRCLE('',#34133,5.);
#2245=CIRCLE('',#34138,5.);
#2246=CIRCLE('',#34142,75.);
#2247=CIRCLE('',#34144,75.);
#2248=CIRCLE('',#34146,5.);
#2249=CIRCLE('',#34151,75.);
#2250=CIRCLE('',#34155,11.5);
#2251=CIRCLE('',#34156,11.5);
#2252=CIRCLE('',#34157,11.5);
#2253=CIRCLE('',#34158,11.5);
#2254=CIRCLE('',#34159,5.75);
#2255=CIRCLE('',#34160,5.75);
#2256=CIRCLE('',#34161,5.75);
#2257=CIRCLE('',#34162,5.75);
#2258=CIRCLE('',#34163,11.5);
#2259=CIRCLE('',#34164,11.5);
#2260=CIRCLE('',#34165,11.5);
#2261=CIRCLE('',#34166,11.5);
#2262=CIRCLE('',#34168,11.5);
#2263=CIRCLE('',#34170,2.54);
#2264=CIRCLE('',#34171,8.960000684551);
#2265=CIRCLE('',#34172,2.54);
#2266=CIRCLE('',#34174,2.54);
#2267=CIRCLE('',#34176,49.78996319131);
#2268=CIRCLE('',#34177,8.960000684551);
#2269=CIRCLE('',#34178,5.75);
#2270=CIRCLE('',#34180,49.78996141255);
#2271=CIRCLE('',#34181,8.960000684551);
#2272=CIRCLE('',#34182,5.75);
#2273=CIRCLE('',#34184,49.78996319131);
#2274=CIRCLE('',#34185,5.75);
#2275=CIRCLE('',#34187,49.78996141255);
#2276=CIRCLE('',#34188,8.960000684551);
#2277=CIRCLE('',#34189,5.75);
#2278=CIRCLE('',#34195,2.539999943211);
#2279=CIRCLE('',#34196,47.25);
#2280=CIRCLE('',#34197,2.54);
#2281=CIRCLE('',#34198,2.539975517689);
#2282=CIRCLE('',#34200,47.25);
#2283=CIRCLE('',#34201,47.25);
#2284=CIRCLE('',#34202,47.25);
#2285=CIRCLE('',#34203,47.25);
#2286=CIRCLE('',#34204,47.25);
#2287=CIRCLE('',#34205,47.25);
#2288=CIRCLE('',#34206,47.25);
#2289=CIRCLE('',#34207,47.25);
#2290=CIRCLE('',#34208,47.25);
#2291=CIRCLE('',#34209,47.25);
#2292=CIRCLE('',#34211,49.79);
#2293=CIRCLE('',#34212,2.54);
#2294=CIRCLE('',#34213,2.54);
#2295=CIRCLE('',#34216,49.79);
#2296=CIRCLE('',#34218,49.79);
#2297=CIRCLE('',#34220,49.79);
#2298=CIRCLE('',#34222,2.54);
#2299=CIRCLE('',#34225,2.54);
#2300=CIRCLE('',#34227,2.539999283673);
#2301=CIRCLE('',#34228,2.54);
#2302=CIRCLE('',#34230,2.54);
#2303=CIRCLE('',#34232,11.5);
#2304=CIRCLE('',#34233,2.54);
#2305=CIRCLE('',#34237,2.54);
#2306=CIRCLE('',#34238,2.54);
#2307=CIRCLE('',#34240,11.5);
#2308=CIRCLE('',#34241,2.54);
#2309=CIRCLE('',#34244,2.540003327809);
#2310=CIRCLE('',#34246,2.54);
#2311=CIRCLE('',#34248,2.54);
#2312=CIRCLE('',#34249,2.539975498399);
#2313=CIRCLE('',#34250,2.539999989149);
#2314=CIRCLE('',#34252,2.54);
#2315=CIRCLE('',#34254,2.54);
#2316=CIRCLE('',#34257,2.54);
#2317=CIRCLE('',#34258,2.539975299827);
#2318=CIRCLE('',#34260,2.54);
#2319=CIRCLE('',#34262,2.539999283673);
#2320=CIRCLE('',#34263,2.54);
#2321=CIRCLE('',#34265,2.540003327809);
#2322=CIRCLE('',#34267,2.54);
#2323=CIRCLE('',#34269,2.54);
#2324=CIRCLE('',#34270,2.539975344705);
#2325=CIRCLE('',#34272,2.54);
#2326=CIRCLE('',#34274,2.54);
#2327=CIRCLE('',#34277,2.54);
#2328=CIRCLE('',#34279,2.54);
#2329=CIRCLE('',#34282,2.54);
#2330=CIRCLE('',#34283,2.539975498399);
#2331=CIRCLE('',#34284,2.539999989149);
#2332=CIRCLE('',#34286,2.54);
#2333=CIRCLE('',#34288,2.54);
#2334=CIRCLE('',#34290,2.540003327809);
#2335=CIRCLE('',#34292,2.54);
#2336=CIRCLE('',#34295,11.5);
#2337=CIRCLE('',#34297,2.54);
#2338=CIRCLE('',#34298,2.54);
#2339=CIRCLE('',#34300,2.54);
#2340=CIRCLE('',#34303,2.54);
#2341=CIRCLE('',#34305,2.54);
#2342=CIRCLE('',#34306,2.539999283994);
#2343=CIRCLE('',#34308,2.539975344705);
#2344=CIRCLE('',#34309,2.539999943211);
#2345=CIRCLE('',#34311,2.54);
#2346=CIRCLE('',#34312,2.539975517689);
#2347=CIRCLE('',#34314,2.54);
#2348=CIRCLE('',#34316,2.539999283673);
#2349=CIRCLE('',#34317,2.54);
#2350=CIRCLE('',#34320,2.54);
#2351=CIRCLE('',#34323,2.54);
#2352=CIRCLE('',#34324,2.54);
#2353=CIRCLE('',#34326,2.540003327809);
#2354=CIRCLE('',#34328,2.54);
#2355=CIRCLE('',#34329,2.539999283673);
#2356=CIRCLE('',#34331,2.54);
#2357=CIRCLE('',#34333,2.53997529983);
#2358=CIRCLE('',#34334,2.54);
#2359=CIRCLE('',#34336,2.54);
#2360=CIRCLE('',#34339,2.54);
#2361=CIRCLE('',#34342,2.54);
#2362=CIRCLE('',#34345,44.70999983335);
#2363=CIRCLE('',#34346,2.54);
#2364=CIRCLE('',#34348,38.28999862038);
#2365=CIRCLE('',#34350,35.75);
#2366=CIRCLE('',#34351,35.75);
#2367=CIRCLE('',#34352,2.54);
#2368=CIRCLE('',#34354,35.75);
#2369=CIRCLE('',#34356,27.315);
#2370=CIRCLE('',#34358,27.315);
#2371=CIRCLE('',#34360,23.435);
#2372=CIRCLE('',#34362,23.435);
#2373=CIRCLE('',#34364,15.);
#2374=CIRCLE('',#34366,15.);
#2375=CIRCLE('',#34368,23.435);
#2376=CIRCLE('',#34370,23.435);
#2377=CIRCLE('',#34372,27.315);
#2378=CIRCLE('',#34374,27.315);
#2379=CIRCLE('',#34376,35.75);
#2380=CIRCLE('',#34378,35.75);
#2381=CIRCLE('',#34380,11.5);
#2382=CIRCLE('',#34381,11.5);
#2383=CIRCLE('',#34382,11.5);
#2384=CIRCLE('',#34383,11.5);
#2385=CIRCLE('',#34394,6.);
#2386=CIRCLE('',#34395,6.);
#2387=CIRCLE('',#34396,0.1);
#2388=CIRCLE('',#34397,6.1);
#2389=CIRCLE('',#34399,6.);
#2390=CIRCLE('',#34400,6.);
#2391=CIRCLE('',#34402,9.);
#2392=CIRCLE('',#34404,4.9264625);
#2393=CIRCLE('',#34407,9.);
#2394=CIRCLE('',#34408,9.);
#2395=CIRCLE('',#34409,1.2);
#2396=CIRCLE('',#34410,7.8);
#2397=CIRCLE('',#34422,5.);
#2398=CIRCLE('',#34423,5.);
#2399=CIRCLE('',#34424,0.1);
#2400=CIRCLE('',#34425,5.1);
#2401=CIRCLE('',#34427,5.);
#2402=CIRCLE('',#34428,5.);
#2403=CIRCLE('',#34430,8.);
#2404=CIRCLE('',#34432,4.079825);
#2405=CIRCLE('',#34435,8.);
#2406=CIRCLE('',#34436,8.);
#2407=CIRCLE('',#34437,1.);
#2408=CIRCLE('',#34438,7.);
#2409=CIRCLE('',#34450,5.);
#2410=CIRCLE('',#34451,5.);
#2411=CIRCLE('',#34452,0.1);
#2412=CIRCLE('',#34453,5.1);
#2413=CIRCLE('',#34455,5.);
#2414=CIRCLE('',#34456,5.);
#2415=CIRCLE('',#34458,8.);
#2416=CIRCLE('',#34460,4.079825);
#2417=CIRCLE('',#34463,8.);
#2418=CIRCLE('',#34464,8.);
#2419=CIRCLE('',#34465,1.);
#2420=CIRCLE('',#34466,7.);
#2421=CIRCLE('',#34478,5.);
#2422=CIRCLE('',#34479,5.);
#2423=CIRCLE('',#34480,0.4);
#2424=CIRCLE('',#34481,5.4);
#2425=CIRCLE('',#34483,5.);
#2426=CIRCLE('',#34484,5.);
#2427=CIRCLE('',#34486,7.3);
#2428=CIRCLE('',#34488,4.079825);
#2429=CIRCLE('',#34491,8.00000000000003);
#2430=CIRCLE('',#34493,8.00000000000003);
#2431=CIRCLE('',#34495,8.00000000000003);
#2432=CIRCLE('',#34497,8.00000000000003);
#2433=CIRCLE('',#34499,8.00000000000003);
#2434=CIRCLE('',#34501,8.00000000000003);
#2435=CIRCLE('',#34506,7.3);
#2436=CIRCLE('',#34530,4.);
#2437=CIRCLE('',#34531,4.);
#2438=CIRCLE('',#34533,4.);
#2439=CIRCLE('',#34534,4.);
#2440=CIRCLE('',#34536,4.);
#2441=CIRCLE('',#34537,4.);
#2442=CIRCLE('',#34539,4.);
#2443=CIRCLE('',#34540,4.);
#2444=CIRCLE('',#34542,4.);
#2445=CIRCLE('',#34543,4.);
#2446=CIRCLE('',#34545,4.);
#2447=CIRCLE('',#34546,4.);
#2448=CIRCLE('',#34569,4.08939999999988);
#2449=CIRCLE('',#34570,4.08939999999988);
#2450=CIRCLE('',#34575,4.0893999999995);
#2451=CIRCLE('',#34578,84.4550000000159);
#2452=CIRCLE('',#34579,84.4549999999612);
#2453=CIRCLE('',#34580,84.4549999999434);
#2454=CIRCLE('',#34581,84.4550000000244);
#2455=CIRCLE('',#34588,4.08940000000003);
#2456=CIRCLE('',#34589,4.08939999999987);
#2457=CIRCLE('',#34591,84.4549999999862);
#2458=CIRCLE('',#34592,84.4550000001664);
#2459=CIRCLE('',#34593,84.4550000000658);
#2460=CIRCLE('',#34594,84.4549999999639);
#2461=CIRCLE('',#34597,5.73418625921224);
#2462=CIRCLE('',#34598,6.39225125407266);
#2463=CIRCLE('',#34599,6.39225125407329);
#2464=CIRCLE('',#34600,5.73418625920595);
#2465=CIRCLE('',#34601,6.39225125407447);
#2466=CIRCLE('',#34602,6.39225125407165);
#2467=CIRCLE('',#34603,5.73418625919979);
#2468=CIRCLE('',#34604,6.39225125407114);
#2469=CIRCLE('',#34605,6.39225125407334);
#2470=CIRCLE('',#34606,5.73418625920593);
#2471=CIRCLE('',#34607,6.3922512540724);
#2472=CIRCLE('',#34608,6.39225125407298);
#2473=CIRCLE('',#34610,6.3922512540739);
#2474=CIRCLE('',#34612,5.73418625919449);
#2475=CIRCLE('',#34614,4.08939999999995);
#2476=CIRCLE('',#34616,4.08939999999987);
#2477=CIRCLE('',#34618,4.08939999999931);
#2478=CIRCLE('',#34619,4.08939999999987);
#2479=CIRCLE('',#34621,6.39225125406976);
#2480=CIRCLE('',#34623,5.7341862591997);
#2481=CIRCLE('',#34625,6.39225125407312);
#2482=CIRCLE('',#34627,6.39225125407987);
#2483=CIRCLE('',#34629,5.73418625919762);
#2484=CIRCLE('',#34631,6.39225125407758);
#2485=CIRCLE('',#34633,6.39225125407361);
#2486=CIRCLE('',#34635,5.73418625916851);
#2487=CIRCLE('',#34637,6.39225125407298);
#2488=CIRCLE('',#34639,6.39225125407049);
#2489=CIRCLE('',#34641,5.73418625919762);
#2490=CIRCLE('',#34643,6.3922512540717);
#2491=CIRCLE('',#34649,4.82600000000001);
#2492=CIRCLE('',#34650,4.82600000000001);
#2493=CIRCLE('',#34653,4.82600000000004);
#2494=CIRCLE('',#34654,4.82599999999999);
#2495=CIRCLE('',#34657,4.82600000000005);
#2496=CIRCLE('',#34658,4.82600000000005);
#2497=CIRCLE('',#34661,4.82600000000003);
#2498=CIRCLE('',#34662,4.82599999999998);
#2499=CIRCLE('',#34666,4.0894);
#2500=CIRCLE('',#34667,4.08940000000001);
#2501=CIRCLE('',#34668,3.04799999999999);
#2502=CIRCLE('',#34669,3.04799999999999);
#2503=CIRCLE('',#34670,3.04800000000004);
#2504=CIRCLE('',#34671,3.04800000000004);
#2505=CIRCLE('',#34673,3.04799999999999);
#2506=CIRCLE('',#34676,3.04799999999999);
#2507=CIRCLE('',#34679,3.04800000000004);
#2508=CIRCLE('',#34682,3.04800000000004);
#2509=CIRCLE('',#34686,4.08940000000001);
#2510=CIRCLE('',#34687,6.47939701209842);
#2511=CIRCLE('',#34688,5.83117497592219);
#2512=CIRCLE('',#34689,6.47939701210061);
#2513=CIRCLE('',#34690,6.47939701209921);
#2514=CIRCLE('',#34691,5.83117497591494);
#2515=CIRCLE('',#34692,6.4793970120992);
#2516=CIRCLE('',#34693,6.47939701210015);
#2517=CIRCLE('',#34694,5.83117497591959);
#2518=CIRCLE('',#34695,6.47939701209921);
#2519=CIRCLE('',#34696,6.47939701209916);
#2520=CIRCLE('',#34697,5.83117497592765);
#2521=CIRCLE('',#34698,6.479397012098);
#2522=CIRCLE('',#34701,4.0894);
#2523=CIRCLE('',#34702,6.47939701209688);
#2524=CIRCLE('',#34703,5.83117497592362);
#2525=CIRCLE('',#34704,6.47939701209502);
#2526=CIRCLE('',#34705,6.47939701209653);
#2527=CIRCLE('',#34706,5.83117497590882);
#2528=CIRCLE('',#34707,6.47939701209738);
#2529=CIRCLE('',#34708,6.47939701209747);
#2530=CIRCLE('',#34709,5.83117497591427);
#2531=CIRCLE('',#34710,6.47939701209745);
#2532=CIRCLE('',#34711,6.47939701209746);
#2533=CIRCLE('',#34712,5.83117497591896);
#2534=CIRCLE('',#34713,6.47939701209731);
#2535=CIRCLE('',#34754,82.9309999999989);
#2536=CIRCLE('',#34756,82.9310000000032);
#2537=CIRCLE('',#34759,82.931);
#2538=CIRCLE('',#34761,82.9309999999999);
#2539=CIRCLE('',#34763,82.931000000047);
#2540=CIRCLE('',#34765,82.9310000000546);
#2541=CIRCLE('',#34768,11.1760000000001);
#2542=CIRCLE('',#34782,11.1760000000001);
#2543=CIRCLE('',#34787,6.39225125407378);
#2544=CIRCLE('',#34788,5.73418625920022);
#2545=CIRCLE('',#34789,6.39225125407387);
#2546=CIRCLE('',#34790,6.39225125407349);
#2547=CIRCLE('',#34791,5.73418625919864);
#2548=CIRCLE('',#34792,6.39225125407317);
#2549=CIRCLE('',#34793,6.39225125407526);
#2550=CIRCLE('',#34794,5.73418625919519);
#2551=CIRCLE('',#34795,6.39225125407178);
#2552=CIRCLE('',#34796,6.39225125407384);
#2553=CIRCLE('',#34809,90.932);
#2554=CIRCLE('',#34810,82.931);
#2555=CIRCLE('',#34812,4.12750000000046);
#2556=CIRCLE('',#34813,4.12750000000046);
#2557=CIRCLE('',#34815,0.0083587400462651);
#2558=CIRCLE('',#34816,0.0083587400462651);
#2559=CIRCLE('',#34818,4.1275);
#2560=CIRCLE('',#34819,4.1275);
#2561=CIRCLE('',#34821,0.00835874004620744);
#2562=CIRCLE('',#34822,0.00835874004620744);
#2563=CIRCLE('',#34824,4.12750000000005);
#2564=CIRCLE('',#34825,7.13809812492437);
#2565=CIRCLE('',#34827,0.00835888222172394);
#2566=CIRCLE('',#34828,0.00835888222172394);
#2567=CIRCLE('',#34829,7.13809812641026);
#2568=CIRCLE('',#34830,7.13809812562023);
#2569=CIRCLE('',#34832,90.932);
#2570=CIRCLE('',#34833,90.932);
#2571=CIRCLE('',#34834,19.0499999999999);
#2572=CIRCLE('',#34835,71.882);
#2573=CIRCLE('',#34839,12.446);
#2574=CIRCLE('',#34841,82.931);
#2575=CIRCLE('',#34842,82.931);
#2576=CIRCLE('',#34844,5.64270291970328);
#2577=CIRCLE('',#34847,5.47861854669138);
#2578=CIRCLE('',#34851,5.08000000000016);
#2579=CIRCLE('',#34852,5.08000000000016);
#2580=CIRCLE('',#34853,4.7371);
#2581=CIRCLE('',#34854,2.76860000000045);
#2582=CIRCLE('',#34856,5.08000000000016);
#2583=CIRCLE('',#34859,5.08000000000016);
#2584=CIRCLE('',#34862,5.08);
#2585=CIRCLE('',#34863,5.08);
#2586=CIRCLE('',#34864,4.73709999999994);
#2587=CIRCLE('',#34865,2.7686);
#2588=CIRCLE('',#34867,5.08);
#2589=CIRCLE('',#34870,5.08);
#2590=CIRCLE('',#34873,3.90271);
#2591=CIRCLE('',#34875,3.90271);
#2592=CIRCLE('',#34876,3.90271);
#2593=CIRCLE('',#34878,4.7625);
#2594=CIRCLE('',#34880,3.90271);
#2595=CIRCLE('',#34882,3.90271);
#2596=CIRCLE('',#34883,3.90271);
#2597=CIRCLE('',#34885,4.7625);
#2598=CIRCLE('',#34887,3.90271000000005);
#2599=CIRCLE('',#34889,3.90271000000005);
#2600=CIRCLE('',#34890,3.90271000000005);
#2601=CIRCLE('',#34892,4.7625);
#2602=CIRCLE('',#34894,3.90271);
#2603=CIRCLE('',#34896,3.90271);
#2604=CIRCLE('',#34897,3.90271);
#2605=CIRCLE('',#34899,4.7625);
#2606=CIRCLE('',#34901,82.2083254018421);
#2607=CIRCLE('',#34903,8.76300000000001);
#2608=CIRCLE('',#34904,8.76300000000001);
#2609=CIRCLE('',#34905,8.76300000000001);
#2610=CIRCLE('',#34906,8.76299999999998);
#2611=CIRCLE('',#34907,57.15);
#2612=CIRCLE('',#34909,57.15);
#2613=CIRCLE('',#34911,52.451);
#2614=CIRCLE('',#34913,52.451);
#2615=CIRCLE('',#34915,13.081);
#2616=CIRCLE('',#34917,13.081);
#2617=CIRCLE('',#34919,12.446);
#2618=CIRCLE('',#34922,8.76300000000001);
#2619=CIRCLE('',#34923,2.794);
#2620=CIRCLE('',#34926,2.794);
#2621=CIRCLE('',#34929,8.76299999999998);
#2622=CIRCLE('',#34931,2.794);
#2623=CIRCLE('',#34933,2.794);
#2624=CIRCLE('',#34936,2.79400000000001);
#2625=CIRCLE('',#34938,2.79400000000001);
#2626=CIRCLE('',#34940,8.76300000000001);
#2627=CIRCLE('',#34943,8.76300000000001);
#2628=CIRCLE('',#34945,2.794);
#2629=CIRCLE('',#34947,2.794);
#2630=CIRCLE('',#34951,2.76860000000046);
#2631=CIRCLE('',#34952,2.76860000000045);
#2632=CIRCLE('',#34955,2.7686);
#2633=CIRCLE('',#34956,2.7686);
#2634=CIRCLE('',#34957,2.18440000000005);
#2635=CIRCLE('',#34959,2.7686);
#2636=CIRCLE('',#34962,2.76860000000046);
#2637=CIRCLE('',#34964,2.1844);
#2638=CIRCLE('',#34966,4.73709999999989);
#2639=CIRCLE('',#34967,4.73709999999993);
#2640=CIRCLE('',#34969,2.1844);
#2641=CIRCLE('',#34972,4.9247349817135);
#2642=CIRCLE('',#34973,5.64270291970351);
#2643=CIRCLE('',#34974,5.47861854669129);
#2644=CIRCLE('',#34975,5.64270291970121);
#2645=CIRCLE('',#34976,4.92473498170593);
#2646=CIRCLE('',#34977,5.64270291970139);
#2647=CIRCLE('',#34978,5.47861854669133);
#2648=CIRCLE('',#34979,5.64270291970326);
#2649=CIRCLE('',#34980,4.92473498170479);
#2650=CIRCLE('',#34981,5.64270291970299);
#2651=CIRCLE('',#34982,4.92473498170593);
#2652=CIRCLE('',#34983,5.64270291970284);
#2653=CIRCLE('',#34984,5.47861854669129);
#2654=CIRCLE('',#34985,5.64270291970352);
#2655=CIRCLE('',#34987,4.73710000000003);
#2656=CIRCLE('',#34988,2.1844);
#2657=CIRCLE('',#34991,4.73710000000006);
#2658=CIRCLE('',#34993,4.92473498170677);
#2659=CIRCLE('',#34994,5.64270291970129);
#2660=CIRCLE('',#34995,5.47861854668747);
#2661=CIRCLE('',#34996,5.64270291969926);
#2662=CIRCLE('',#34997,4.9247349817059);
#2663=CIRCLE('',#34998,5.64270291970433);
#2664=CIRCLE('',#34999,5.47861854667958);
#2665=CIRCLE('',#35000,5.64270291970706);
#2666=CIRCLE('',#35001,4.92473498170641);
#2667=CIRCLE('',#35002,5.64270291970507);
#2668=CIRCLE('',#35003,5.47861854667962);
#2669=CIRCLE('',#35004,5.64270291970448);
#2670=CIRCLE('',#35005,4.9247349817059);
#2671=CIRCLE('',#35006,5.64270291970619);
#2672=CIRCLE('',#35007,5.47861854669134);
#2673=CIRCLE('',#35008,5.64270291969768);
#2674=CIRCLE('',#35042,0.5);
#2675=CIRCLE('',#35043,0.5);
#2676=CIRCLE('',#35045,6.188);
#2677=CIRCLE('',#35046,6.188);
#2678=CIRCLE('',#35047,6.188);
#2679=CIRCLE('',#35048,6.188);
#2680=CIRCLE('',#35050,0.5);
#2681=CIRCLE('',#35051,0.5);
#2682=CIRCLE('',#35053,1.00000000000015);
#2683=CIRCLE('',#35055,0.5);
#2684=CIRCLE('',#35056,0.5);
#2685=CIRCLE('',#35057,0.500000000000003);
#2686=CIRCLE('',#35058,0.499999999999992);
#2687=CIRCLE('',#35066,0.5);
#2688=CIRCLE('',#35067,0.5);
#2689=CIRCLE('',#35069,0.5);
#2690=CIRCLE('',#35070,0.499999999999998);
#2691=CIRCLE('',#35071,0.499999999999992);
#2692=CIRCLE('',#35073,0.499999999999998);
#2693=CIRCLE('',#35074,0.499999999999972);
#2694=CIRCLE('',#35075,0.499999999999996);
#2695=CIRCLE('',#35077,0.5);
#2696=CIRCLE('',#35078,0.499999999999972);
#2697=CIRCLE('',#35079,0.499999999999998);
#2698=CIRCLE('',#35081,0.499999999999972);
#2699=CIRCLE('',#35082,0.499999999999972);
#2700=CIRCLE('',#35083,0.499999999999998);
#2701=CIRCLE('',#35085,0.5);
#2702=CIRCLE('',#35086,0.499999999999998);
#2703=CIRCLE('',#35087,0.500000000000114);
#2704=CIRCLE('',#35089,0.499999999999998);
#2705=CIRCLE('',#35090,0.499999999999972);
#2706=CIRCLE('',#35091,0.499999999999972);
#2707=CIRCLE('',#35093,1.00000000000013);
#2708=CIRCLE('',#35094,0.500000000000006);
#2709=CIRCLE('',#35095,0.499999999999998);
#2710=CIRCLE('',#35096,0.5);
#2711=CIRCLE('',#35098,0.49999999999999);
#2712=CIRCLE('',#35099,0.499999999999972);
#2713=CIRCLE('',#35100,0.499999999999994);
#2714=CIRCLE('',#35102,0.5);
#2715=CIRCLE('',#35103,0.5);
#2716=CIRCLE('',#35104,0.500000000000002);
#2717=CIRCLE('',#35106,0.499999999999998);
#2718=CIRCLE('',#35107,0.5);
#2719=CIRCLE('',#35108,0.500000000000007);
#2720=CIRCLE('',#35111,0.5);
#2721=CIRCLE('',#35113,0.499999999999972);
#2722=CIRCLE('',#35114,0.499999999999998);
#2723=CIRCLE('',#35115,0.499999999999998);
#2724=CIRCLE('',#35119,0.500000000000007);
#2725=CIRCLE('',#35120,0.499999999999972);
#2726=CIRCLE('',#35121,0.500000000000003);
#2727=CIRCLE('',#35123,0.5);
#2728=CIRCLE('',#35144,6.18799999999941);
#2729=CIRCLE('',#35145,6.18799999999941);
#2730=CIRCLE('',#35146,6.18799999999941);
#2731=CIRCLE('',#35147,6.18799999999941);
#2732=CIRCLE('',#35153,5.188);
#2733=CIRCLE('',#35155,5.188);
#2734=CIRCLE('',#35156,5.188);
#2735=CIRCLE('',#35158,5.188);
#2736=CIRCLE('',#35160,5.188);
#2737=CIRCLE('',#35161,5.188);
#2738=CIRCLE('',#35163,5.188);
#2739=CIRCLE('',#35165,5.188);
#2740=CIRCLE('',#35166,5.188);
#2741=CIRCLE('',#35168,5.188);
#2742=CIRCLE('',#35170,5.188);
#2743=CIRCLE('',#35171,5.188);
#2744=CIRCLE('',#35194,2.);
#2745=CIRCLE('',#35195,2.);
#2746=CIRCLE('',#35198,2.);
#2747=CIRCLE('',#35199,2.);
#2748=CIRCLE('',#35202,4.);
#2749=CIRCLE('',#35203,4.);
#2750=CIRCLE('',#35206,4.);
#2751=CIRCLE('',#35207,4.);
#2752=CIRCLE('',#35210,2.);
#2753=CIRCLE('',#35211,2.);
#2754=CIRCLE('',#35214,2.);
#2755=CIRCLE('',#35215,2.);
#2756=CIRCLE('',#35218,4.);
#2757=CIRCLE('',#35219,4.);
#2758=CIRCLE('',#35222,4.);
#2759=CIRCLE('',#35223,4.);
#2760=CIRCLE('',#35228,2.);
#2761=CIRCLE('',#35229,2.);
#2762=CIRCLE('',#35232,2.);
#2763=CIRCLE('',#35233,2.);
#2764=CIRCLE('',#35236,4.);
#2765=CIRCLE('',#35237,4.);
#2766=CIRCLE('',#35240,4.);
#2767=CIRCLE('',#35241,4.);
#2768=CIRCLE('',#35244,2.);
#2769=CIRCLE('',#35245,2.);
#2770=CIRCLE('',#35248,2.);
#2771=CIRCLE('',#35249,2.);
#2772=CIRCLE('',#35252,4.);
#2773=CIRCLE('',#35253,4.);
#2774=CIRCLE('',#35256,4.);
#2775=CIRCLE('',#35257,4.);
#2776=CIRCLE('',#35262,2.);
#2777=CIRCLE('',#35263,2.);
#2778=CIRCLE('',#35266,2.);
#2779=CIRCLE('',#35267,2.);
#2780=CIRCLE('',#35270,4.);
#2781=CIRCLE('',#35271,4.);
#2782=CIRCLE('',#35274,4.);
#2783=CIRCLE('',#35275,4.);
#2784=CIRCLE('',#35278,2.);
#2785=CIRCLE('',#35279,2.);
#2786=CIRCLE('',#35282,2.);
#2787=CIRCLE('',#35283,2.);
#2788=CIRCLE('',#35286,4.);
#2789=CIRCLE('',#35287,4.);
#2790=CIRCLE('',#35290,4.);
#2791=CIRCLE('',#35291,4.);
#2792=CIRCLE('',#35296,2.);
#2793=CIRCLE('',#35297,2.);
#2794=CIRCLE('',#35300,2.);
#2795=CIRCLE('',#35301,2.);
#2796=CIRCLE('',#35304,4.);
#2797=CIRCLE('',#35305,4.);
#2798=CIRCLE('',#35308,4.);
#2799=CIRCLE('',#35309,4.);
#2800=CIRCLE('',#35312,2.);
#2801=CIRCLE('',#35313,2.);
#2802=CIRCLE('',#35316,2.);
#2803=CIRCLE('',#35317,2.);
#2804=CIRCLE('',#35320,4.);
#2805=CIRCLE('',#35321,4.);
#2806=CIRCLE('',#35324,4.);
#2807=CIRCLE('',#35325,4.);
#2808=CIRCLE('',#35466,2.);
#2809=CIRCLE('',#35467,2.);
#2810=CIRCLE('',#35470,2.);
#2811=CIRCLE('',#35471,2.);
#2812=CIRCLE('',#35474,4.);
#2813=CIRCLE('',#35475,4.);
#2814=CIRCLE('',#35478,4.);
#2815=CIRCLE('',#35479,4.);
#2816=CIRCLE('',#35482,2.);
#2817=CIRCLE('',#35483,2.);
#2818=CIRCLE('',#35486,2.);
#2819=CIRCLE('',#35487,2.);
#2820=CIRCLE('',#35490,4.);
#2821=CIRCLE('',#35491,4.);
#2822=CIRCLE('',#35494,4.);
#2823=CIRCLE('',#35495,4.);
#2824=CIRCLE('',#35500,2.);
#2825=CIRCLE('',#35501,2.);
#2826=CIRCLE('',#35504,2.);
#2827=CIRCLE('',#35505,2.);
#2828=CIRCLE('',#35508,4.);
#2829=CIRCLE('',#35509,4.);
#2830=CIRCLE('',#35512,4.);
#2831=CIRCLE('',#35513,4.);
#2832=CIRCLE('',#35516,2.);
#2833=CIRCLE('',#35517,2.);
#2834=CIRCLE('',#35520,2.);
#2835=CIRCLE('',#35521,2.);
#2836=CIRCLE('',#35524,4.);
#2837=CIRCLE('',#35525,4.);
#2838=CIRCLE('',#35528,4.);
#2839=CIRCLE('',#35529,4.);
#2840=CIRCLE('',#35534,2.);
#2841=CIRCLE('',#35535,2.);
#2842=CIRCLE('',#35538,2.);
#2843=CIRCLE('',#35539,2.);
#2844=CIRCLE('',#35542,4.);
#2845=CIRCLE('',#35543,4.);
#2846=CIRCLE('',#35546,4.);
#2847=CIRCLE('',#35547,4.);
#2848=CIRCLE('',#35550,2.);
#2849=CIRCLE('',#35551,2.);
#2850=CIRCLE('',#35554,2.);
#2851=CIRCLE('',#35555,2.);
#2852=CIRCLE('',#35558,4.);
#2853=CIRCLE('',#35559,4.);
#2854=CIRCLE('',#35562,4.);
#2855=CIRCLE('',#35563,4.);
#2856=CIRCLE('',#35567,4.);
#2857=CIRCLE('',#35568,4.);
#2858=CIRCLE('',#35571,4.);
#2859=CIRCLE('',#35572,4.);
#2860=CIRCLE('',#35575,4.);
#2861=CIRCLE('',#35576,4.);
#2862=CIRCLE('',#35579,4.);
#2863=CIRCLE('',#35580,4.);
#2864=CIRCLE('',#35583,24.0000000000018);
#2865=CIRCLE('',#35584,24.0000000000018);
#2866=CIRCLE('',#35587,24.0000000000018);
#2867=CIRCLE('',#35588,24.0000000000018);
#2868=CIRCLE('',#35591,24.0000000000018);
#2869=CIRCLE('',#35592,24.0000000000018);
#2870=CIRCLE('',#35595,24.0000000000018);
#2871=CIRCLE('',#35596,24.0000000000018);
#2872=CIRCLE('',#35601,4.);
#2873=CIRCLE('',#35602,4.);
#2874=CIRCLE('',#35605,4.);
#2875=CIRCLE('',#35606,4.);
#2876=CIRCLE('',#35609,4.);
#2877=CIRCLE('',#35610,4.);
#2878=CIRCLE('',#35613,4.);
#2879=CIRCLE('',#35614,4.);
#2880=CIRCLE('',#35617,24.0000000000018);
#2881=CIRCLE('',#35618,24.0000000000018);
#2882=CIRCLE('',#35621,24.0000000000018);
#2883=CIRCLE('',#35622,24.0000000000018);
#2884=CIRCLE('',#35625,24.0000000000018);
#2885=CIRCLE('',#35626,24.0000000000018);
#2886=CIRCLE('',#35629,24.0000000000018);
#2887=CIRCLE('',#35630,24.0000000000018);
#2888=CIRCLE('',#35635,4.);
#2889=CIRCLE('',#35636,4.);
#2890=CIRCLE('',#35639,4.);
#2891=CIRCLE('',#35640,4.);
#2892=CIRCLE('',#35643,4.);
#2893=CIRCLE('',#35644,4.);
#2894=CIRCLE('',#35647,4.);
#2895=CIRCLE('',#35648,4.);
#2896=CIRCLE('',#35651,24.0000000000018);
#2897=CIRCLE('',#35652,24.0000000000018);
#2898=CIRCLE('',#35655,24.0000000000018);
#2899=CIRCLE('',#35656,24.0000000000018);
#2900=CIRCLE('',#35659,24.0000000000018);
#2901=CIRCLE('',#35660,24.0000000000018);
#2902=CIRCLE('',#35663,24.0000000000018);
#2903=CIRCLE('',#35664,24.0000000000018);
#2904=CIRCLE('',#35669,4.);
#2905=CIRCLE('',#35670,4.);
#2906=CIRCLE('',#35673,4.);
#2907=CIRCLE('',#35674,4.);
#2908=CIRCLE('',#35677,4.);
#2909=CIRCLE('',#35678,4.);
#2910=CIRCLE('',#35681,4.);
#2911=CIRCLE('',#35682,4.);
#2912=CIRCLE('',#35685,24.0000000000018);
#2913=CIRCLE('',#35686,24.0000000000018);
#2914=CIRCLE('',#35689,24.0000000000018);
#2915=CIRCLE('',#35690,24.0000000000018);
#2916=CIRCLE('',#35693,24.0000000000018);
#2917=CIRCLE('',#35694,24.0000000000018);
#2918=CIRCLE('',#35697,24.0000000000018);
#2919=CIRCLE('',#35698,24.0000000000018);
#2920=CIRCLE('',#35705,5.053);
#2921=CIRCLE('',#35706,5.053);
#2922=CIRCLE('',#35708,5.053);
#2923=CIRCLE('',#35709,5.053);
#2924=CIRCLE('',#35711,5.053);
#2925=CIRCLE('',#35712,5.053);
#2926=CIRCLE('',#35714,5.053);
#2927=CIRCLE('',#35715,5.053);
#2928=CIRCLE('',#35717,5.053);
#2929=CIRCLE('',#35718,5.053);
#2930=CIRCLE('',#35720,5.053);
#2931=CIRCLE('',#35721,5.053);
#2932=CIRCLE('',#35723,5.053);
#2933=CIRCLE('',#35724,5.053);
#2934=CIRCLE('',#35726,5.053);
#2935=CIRCLE('',#35727,5.053);
#2936=CIRCLE('',#35729,5.053);
#2937=CIRCLE('',#35730,5.053);
#2938=CIRCLE('',#35732,5.053);
#2939=CIRCLE('',#35733,5.053);
#2940=CIRCLE('',#35735,5.053);
#2941=CIRCLE('',#35736,5.053);
#2942=CIRCLE('',#35738,5.053);
#2943=CIRCLE('',#35739,5.053);
#2944=CIRCLE('',#35741,5.053);
#2945=CIRCLE('',#35742,5.053);
#2946=CIRCLE('',#35744,5.053);
#2947=CIRCLE('',#35745,5.053);
#2948=CIRCLE('',#35747,5.053);
#2949=CIRCLE('',#35748,5.053);
#2950=CIRCLE('',#35750,5.053);
#2951=CIRCLE('',#35751,5.053);
#2952=CIRCLE('',#35764,4.188);
#2953=CIRCLE('',#35765,4.188);
#2954=CIRCLE('',#35766,4.188);
#2955=CIRCLE('',#35768,4.188);
#2956=CIRCLE('',#35769,4.188);
#2957=CIRCLE('',#35770,4.188);
#2958=CIRCLE('',#35773,4.188);
#2959=CIRCLE('',#35776,4.188);
#2960=CIRCLE('',#35779,4.188);
#2961=CIRCLE('',#35782,4.188);
#2962=CIRCLE('',#35785,4.188);
#2963=CIRCLE('',#35788,4.188);
#2964=CIRCLE('',#35791,5.188);
#2965=CIRCLE('',#35792,5.188);
#2966=CIRCLE('',#35794,5.188);
#2967=CIRCLE('',#35795,5.188);
#2968=CIRCLE('',#35797,5.188);
#2969=CIRCLE('',#35798,5.188);
#2970=CIRCLE('',#35800,5.188);
#2971=CIRCLE('',#35801,5.188);
#2972=CIRCLE('',#35803,5.188);
#2973=CIRCLE('',#35804,5.188);
#2974=CIRCLE('',#35806,5.188);
#2975=CIRCLE('',#35807,5.188);
#2976=CIRCLE('',#35809,5.188);
#2977=CIRCLE('',#35810,5.188);
#2978=CIRCLE('',#35812,5.188);
#2979=CIRCLE('',#35813,5.188);
#2980=CIRCLE('',#35815,20.);
#2981=CIRCLE('',#35816,20.);
#2982=CIRCLE('',#35818,20.);
#2983=CIRCLE('',#35819,20.);
#2984=CIRCLE('',#35825,4.188);
#2985=CIRCLE('',#35826,4.188);
#2986=CIRCLE('',#35827,4.188);
#2987=CIRCLE('',#35829,4.188);
#2988=CIRCLE('',#35830,4.188);
#2989=CIRCLE('',#35831,4.188);
#2990=CIRCLE('',#35834,4.188);
#2991=CIRCLE('',#35837,4.188);
#2992=CIRCLE('',#35840,4.188);
#2993=CIRCLE('',#35843,4.188);
#2994=CIRCLE('',#35846,4.188);
#2995=CIRCLE('',#35849,4.188);
#2996=CIRCLE('',#35852,5.188);
#2997=CIRCLE('',#35853,5.188);
#2998=CIRCLE('',#35855,5.188);
#2999=CIRCLE('',#35856,5.188);
#3000=CIRCLE('',#35858,5.188);
#3001=CIRCLE('',#35859,5.188);
#3002=CIRCLE('',#35861,5.188);
#3003=CIRCLE('',#35862,5.188);
#3004=CIRCLE('',#35864,5.188);
#3005=CIRCLE('',#35865,5.188);
#3006=CIRCLE('',#35867,5.188);
#3007=CIRCLE('',#35868,5.188);
#3008=CIRCLE('',#35870,5.188);
#3009=CIRCLE('',#35871,5.188);
#3010=CIRCLE('',#35873,5.188);
#3011=CIRCLE('',#35874,5.188);
#3012=CIRCLE('',#35876,20.);
#3013=CIRCLE('',#35877,20.);
#3014=CIRCLE('',#35879,20.);
#3015=CIRCLE('',#35880,20.);
#3016=CIRCLE('',#35886,5.5);
#3017=CIRCLE('',#35887,5.5);
#3018=CIRCLE('',#35889,5.5);
#3019=CIRCLE('',#35890,5.5);
#3020=CIRCLE('',#35892,5.5);
#3021=CIRCLE('',#35893,5.5);
#3022=CIRCLE('',#35895,5.5);
#3023=CIRCLE('',#35896,5.5);
#3024=CIRCLE('',#35898,5.5);
#3025=CIRCLE('',#35899,5.5);
#3026=CIRCLE('',#35901,5.5);
#3027=CIRCLE('',#35902,5.5);
#3028=CIRCLE('',#35913,31.);
#3029=CIRCLE('',#35915,31.);
#3030=CIRCLE('',#35924,7.);
#3031=CIRCLE('',#35925,7.);
#3032=CIRCLE('',#35927,7.);
#3033=CIRCLE('',#35928,7.);
#3034=CIRCLE('',#35930,7.);
#3035=CIRCLE('',#35931,7.);
#3036=CIRCLE('',#35933,7.);
#3037=CIRCLE('',#35934,7.);
#3038=CIRCLE('',#35964,20.);
#3039=CIRCLE('',#35965,20.);
#3040=CIRCLE('',#35967,5.99999999999999);
#3041=CIRCLE('',#35971,6.00000000000001);
#3042=CIRCLE('',#35974,15.);
#3043=CIRCLE('',#35975,15.);
#3044=CIRCLE('',#35976,0.5);
#3045=CIRCLE('',#35977,15.5);
#3046=CIRCLE('',#35979,18.);
#3047=CIRCLE('',#35981,15.);
#3048=CIRCLE('',#35983,15.5);
#3049=CIRCLE('',#35984,0.5);
#3050=CIRCLE('',#35985,15.);
#3051=CIRCLE('',#35986,15.);
#3052=CIRCLE('',#35988,18.);
#3053=CIRCLE('',#35990,15.);
#3054=CIRCLE('',#35991,15.);
#3055=CIRCLE('',#35993,18.5);
#3056=CIRCLE('',#35994,18.5);
#3057=CIRCLE('',#35996,18.5);
#3058=CIRCLE('',#35997,18.5);
#3059=CIRCLE('',#35999,18.5);
#3060=CIRCLE('',#36000,18.5);
#3061=CIRCLE('',#36002,18.5);
#3062=CIRCLE('',#36003,18.5);
#3063=CIRCLE('',#36005,14.);
#3064=CIRCLE('',#36008,6.);
#3065=CIRCLE('',#36012,6.);
#3066=CIRCLE('',#36015,20.);
#3067=CIRCLE('',#36016,20.);
#3068=CIRCLE('',#36018,14.);
#3069=CIRCLE('',#36021,19.);
#3070=CIRCLE('',#36022,0.500000000000029);
#3071=CIRCLE('',#36024,19.5);
#3072=CIRCLE('',#36027,19.5);
#3073=CIRCLE('',#36029,19.);
#3074=CIRCLE('',#36031,0.499999999999998);
#3075=CIRCLE('',#36034,20.);
#3076=CIRCLE('',#36035,20.);
#3077=CIRCLE('',#36037,12.5);
#3078=CIRCLE('',#36038,12.5);
#3079=CIRCLE('',#36039,12.);
#3080=CIRCLE('',#36041,12.5);
#3081=CIRCLE('',#36044,15.);
#3082=CIRCLE('',#36045,15.);
#3083=CIRCLE('',#36046,14.5);
#3084=CIRCLE('',#36048,15.);
#3085=CIRCLE('',#36049,15.);
#3086=CIRCLE('',#36053,5.99999999999999);
#3087=CIRCLE('',#36056,6.00000000000001);
#3088=CIRCLE('',#36059,18.5);
#3089=CIRCLE('',#36060,18.5);
#3090=CIRCLE('',#36061,18.);
#3091=CIRCLE('',#36063,15.5);
#3092=CIRCLE('',#36065,18.5);
#3093=CIRCLE('',#36066,18.5);
#3094=CIRCLE('',#36068,0.5);
#3095=CIRCLE('',#36069,15.);
#3096=CIRCLE('',#36070,15.);
#3097=CIRCLE('',#36072,15.);
#3098=CIRCLE('',#36073,15.);
#3099=CIRCLE('',#36075,0.5);
#3100=CIRCLE('',#36076,15.5);
#3101=CIRCLE('',#36078,18.);
#3102=CIRCLE('',#36080,18.5);
#3103=CIRCLE('',#36081,18.5);
#3104=CIRCLE('',#36083,18.5);
#3105=CIRCLE('',#36084,18.5);
#3106=CIRCLE('',#36086,14.);
#3107=CIRCLE('',#36089,6.);
#3108=CIRCLE('',#36093,6.);
#3109=CIRCLE('',#36096,20.);
#3110=CIRCLE('',#36097,20.);
#3111=CIRCLE('',#36099,19.);
#3112=CIRCLE('',#36100,0.500000000000029);
#3113=CIRCLE('',#36102,19.5);
#3114=CIRCLE('',#36105,19.5);
#3115=CIRCLE('',#36107,19.);
#3116=CIRCLE('',#36109,0.499999999999998);
#3117=CIRCLE('',#36115,30.);
#3118=CIRCLE('',#36116,20.);
#3119=CIRCLE('',#36118,20.);
#3120=CIRCLE('',#36120,30.);
#3121=CIRCLE('',#36124,18.5);
#3122=CIRCLE('',#36125,18.5);
#3123=CIRCLE('',#36127,33.);
#3124=CIRCLE('',#36128,33.);
#3125=CIRCLE('',#36150,28.);
#3126=CIRCLE('',#36151,2.);
#3127=CIRCLE('',#36152,30.);
#3128=CIRCLE('',#36153,30.);
#3129=CIRCLE('',#36155,30.);
#3130=CIRCLE('',#36157,15.);
#3131=CIRCLE('',#36159,32.);
#3132=CIRCLE('',#36160,2.);
#3133=CIRCLE('',#36162,28.3018268963564);
#3134=CIRCLE('',#36163,59.00430282);
#3135=CIRCLE('',#36164,28.3018268963564);
#3136=CIRCLE('',#36165,64.5);
#3137=CIRCLE('',#36166,28.3018268963564);
#3138=CIRCLE('',#36167,59.00430282);
#3139=CIRCLE('',#36168,28.3018268963564);
#3140=CIRCLE('',#36169,64.5);
#3141=CIRCLE('',#36170,28.3018268963564);
#3142=CIRCLE('',#36171,59.00430282);
#3143=CIRCLE('',#36172,28.3018268963564);
#3144=CIRCLE('',#36173,64.5);
#3145=CIRCLE('',#36174,28.3018268963564);
#3146=CIRCLE('',#36175,59.00430282);
#3147=CIRCLE('',#36176,28.3018268963564);
#3148=CIRCLE('',#36177,64.5);
#3149=CIRCLE('',#36178,28.3018268963564);
#3150=CIRCLE('',#36179,59.00430282);
#3151=CIRCLE('',#36180,28.3018268963564);
#3152=CIRCLE('',#36181,64.5);
#3153=CIRCLE('',#36182,28.3018268963564);
#3154=CIRCLE('',#36183,59.00430282);
#3155=CIRCLE('',#36184,28.3018268963564);
#3156=CIRCLE('',#36185,64.5);
#3157=CIRCLE('',#36186,28.3018268963564);
#3158=CIRCLE('',#36187,59.00430282);
#3159=CIRCLE('',#36188,28.3018268963564);
#3160=CIRCLE('',#36189,64.5);
#3161=CIRCLE('',#36190,28.3018268963564);
#3162=CIRCLE('',#36191,59.00430282);
#3163=CIRCLE('',#36192,28.3018268963564);
#3164=CIRCLE('',#36193,64.5);
#3165=CIRCLE('',#36194,28.3018268963564);
#3166=CIRCLE('',#36195,59.00430282);
#3167=CIRCLE('',#36196,28.3018268963564);
#3168=CIRCLE('',#36197,64.5);
#3169=CIRCLE('',#36198,28.3018268963564);
#3170=CIRCLE('',#36199,59.00430282);
#3171=CIRCLE('',#36200,28.3018268963564);
#3172=CIRCLE('',#36201,64.5);
#3173=CIRCLE('',#36202,28.3018268963564);
#3174=CIRCLE('',#36203,59.00430282);
#3175=CIRCLE('',#36204,28.3018268963564);
#3176=CIRCLE('',#36205,64.5);
#3177=CIRCLE('',#36206,28.3018268963564);
#3178=CIRCLE('',#36207,59.00430282);
#3179=CIRCLE('',#36208,28.3018268963564);
#3180=CIRCLE('',#36209,64.5);
#3181=CIRCLE('',#36210,28.3018268963564);
#3182=CIRCLE('',#36211,59.00430282);
#3183=CIRCLE('',#36212,28.3018268963564);
#3184=CIRCLE('',#36213,64.5);
#3185=CIRCLE('',#36214,28.3018268963564);
#3186=CIRCLE('',#36215,59.00430282);
#3187=CIRCLE('',#36216,28.3018268963564);
#3188=CIRCLE('',#36217,64.5);
#3189=CIRCLE('',#36218,28.3018268963564);
#3190=CIRCLE('',#36219,59.00430282);
#3191=CIRCLE('',#36220,28.3018268963564);
#3192=CIRCLE('',#36221,64.5);
#3193=CIRCLE('',#36222,28.3018268963564);
#3194=CIRCLE('',#36223,59.00430282);
#3195=CIRCLE('',#36224,28.3018268963564);
#3196=CIRCLE('',#36225,64.5);
#3197=CIRCLE('',#36226,28.3018268963564);
#3198=CIRCLE('',#36227,59.00430282);
#3199=CIRCLE('',#36228,28.3018268963564);
#3200=CIRCLE('',#36229,64.5);
#3201=CIRCLE('',#36230,28.3018268963564);
#3202=CIRCLE('',#36231,59.00430282);
#3203=CIRCLE('',#36232,28.3018268963564);
#3204=CIRCLE('',#36233,64.5);
#3205=CIRCLE('',#36234,28.3018268963564);
#3206=CIRCLE('',#36235,59.00430282);
#3207=CIRCLE('',#36236,28.3018268963564);
#3208=CIRCLE('',#36237,64.5);
#3209=CIRCLE('',#36238,28.3018268963564);
#3210=CIRCLE('',#36239,59.00430282);
#3211=CIRCLE('',#36240,28.3018268963564);
#3212=CIRCLE('',#36241,64.5);
#3213=CIRCLE('',#36242,28.3018268963564);
#3214=CIRCLE('',#36243,59.00430282);
#3215=CIRCLE('',#36244,28.3018268963564);
#3216=CIRCLE('',#36245,64.5);
#3217=CIRCLE('',#36246,28.3018268963564);
#3218=CIRCLE('',#36247,59.00430282);
#3219=CIRCLE('',#36248,28.3018268963564);
#3220=CIRCLE('',#36249,64.5);
#3221=CIRCLE('',#36250,28.3018268963564);
#3222=CIRCLE('',#36251,59.00430282);
#3223=CIRCLE('',#36252,28.3018268963564);
#3224=CIRCLE('',#36253,64.5);
#3225=CIRCLE('',#36254,28.3018268963564);
#3226=CIRCLE('',#36255,59.00430282);
#3227=CIRCLE('',#36256,28.3018268963564);
#3228=CIRCLE('',#36257,64.5);
#3229=CIRCLE('',#36258,28.3018268963564);
#3230=CIRCLE('',#36259,59.00430282);
#3231=CIRCLE('',#36260,28.3018268963564);
#3232=CIRCLE('',#36261,64.5);
#3233=CIRCLE('',#36262,28.3018268963564);
#3234=CIRCLE('',#36263,59.00430282);
#3235=CIRCLE('',#36264,28.3018268963564);
#3236=CIRCLE('',#36265,64.5);
#3237=CIRCLE('',#36266,28.3018268963564);
#3238=CIRCLE('',#36267,59.00430282);
#3239=CIRCLE('',#36268,28.3018268963564);
#3240=CIRCLE('',#36269,64.5);
#3241=CIRCLE('',#36270,28.3018268963564);
#3242=CIRCLE('',#36271,59.00430282);
#3243=CIRCLE('',#36272,28.3018268963564);
#3244=CIRCLE('',#36273,64.5);
#3245=CIRCLE('',#36274,28.3018268963564);
#3246=CIRCLE('',#36275,59.00430282);
#3247=CIRCLE('',#36276,28.3018268963564);
#3248=CIRCLE('',#36277,64.5);
#3249=CIRCLE('',#36278,28.3018268963564);
#3250=CIRCLE('',#36279,59.00430282);
#3251=CIRCLE('',#36280,28.3018268963564);
#3252=CIRCLE('',#36281,64.5);
#3253=CIRCLE('',#36282,28.3018268963564);
#3254=CIRCLE('',#36283,59.00430282);
#3255=CIRCLE('',#36284,28.3018268963564);
#3256=CIRCLE('',#36285,64.5);
#3257=CIRCLE('',#36286,28.3018268963564);
#3258=CIRCLE('',#36287,59.00430282);
#3259=CIRCLE('',#36288,28.3018268963564);
#3260=CIRCLE('',#36289,64.5);
#3261=CIRCLE('',#36290,28.3018268963564);
#3262=CIRCLE('',#36291,59.00430282);
#3263=CIRCLE('',#36292,28.3018268963564);
#3264=CIRCLE('',#36293,64.5);
#3265=CIRCLE('',#36294,28.3018268963564);
#3266=CIRCLE('',#36295,59.00430282);
#3267=CIRCLE('',#36296,28.3018268963564);
#3268=CIRCLE('',#36297,64.5);
#3269=CIRCLE('',#36298,28.3018268963564);
#3270=CIRCLE('',#36299,59.00430282);
#3271=CIRCLE('',#36300,28.3018268963564);
#3272=CIRCLE('',#36301,64.5);
#3273=CIRCLE('',#36302,28.3018268963564);
#3274=CIRCLE('',#36303,59.00430282);
#3275=CIRCLE('',#36304,28.3018268963564);
#3276=CIRCLE('',#36305,64.5);
#3277=CIRCLE('',#36306,28.3018268963564);
#3278=CIRCLE('',#36307,59.00430282);
#3279=CIRCLE('',#36308,28.3018268963564);
#3280=CIRCLE('',#36309,64.5);
#3281=CIRCLE('',#36310,28.3018268963564);
#3282=CIRCLE('',#36311,59.00430282);
#3283=CIRCLE('',#36312,28.3018268963564);
#3284=CIRCLE('',#36313,64.5);
#3285=CIRCLE('',#36314,28.3018268963564);
#3286=CIRCLE('',#36315,59.00430282);
#3287=CIRCLE('',#36316,28.3018268963564);
#3288=CIRCLE('',#36317,64.5);
#3289=CIRCLE('',#36318,28.3018268963564);
#3290=CIRCLE('',#36319,59.00430282);
#3291=CIRCLE('',#36320,28.3018268963564);
#3292=CIRCLE('',#36321,64.5);
#3293=CIRCLE('',#36322,28.3018268963564);
#3294=CIRCLE('',#36323,59.00430282);
#3295=CIRCLE('',#36324,28.3018268963564);
#3296=CIRCLE('',#36325,64.5);
#3297=CIRCLE('',#36326,28.3018268963564);
#3298=CIRCLE('',#36327,59.00430282);
#3299=CIRCLE('',#36328,28.3018268963564);
#3300=CIRCLE('',#36329,64.5);
#3301=CIRCLE('',#36330,28.3018268963564);
#3302=CIRCLE('',#36331,59.00430282);
#3303=CIRCLE('',#36332,28.3018268963564);
#3304=CIRCLE('',#36333,64.5);
#3305=CIRCLE('',#36334,28.3018268963564);
#3306=CIRCLE('',#36335,59.00430282);
#3307=CIRCLE('',#36336,28.3018268963564);
#3308=CIRCLE('',#36337,64.5);
#3309=CIRCLE('',#36338,28.3018268963564);
#3310=CIRCLE('',#36339,59.00430282);
#3311=CIRCLE('',#36340,28.3018268963564);
#3312=CIRCLE('',#36341,64.5);
#3313=CIRCLE('',#36342,28.3018268963564);
#3314=CIRCLE('',#36343,59.00430282);
#3315=CIRCLE('',#36344,28.3018268963564);
#3316=CIRCLE('',#36345,64.5);
#3317=CIRCLE('',#36346,28.3018268963564);
#3318=CIRCLE('',#36347,59.00430282);
#3319=CIRCLE('',#36348,28.3018268963564);
#3320=CIRCLE('',#36349,64.5);
#3321=CIRCLE('',#36350,28.3018268963564);
#3322=CIRCLE('',#36351,59.00430282);
#3323=CIRCLE('',#36352,28.3018268963564);
#3324=CIRCLE('',#36353,64.5);
#3325=CIRCLE('',#36357,15.);
#3326=CIRCLE('',#36360,59.00430282);
#3327=CIRCLE('',#36362,28.3018268963564);
#3328=CIRCLE('',#36364,28.3018268963564);
#3329=CIRCLE('',#36366,59.00430282);
#3330=CIRCLE('',#36368,28.3018268963564);
#3331=CIRCLE('',#36370,28.3018268963564);
#3332=CIRCLE('',#36372,59.00430282);
#3333=CIRCLE('',#36374,28.3018268963564);
#3334=CIRCLE('',#36376,28.3018268963564);
#3335=CIRCLE('',#36378,59.00430282);
#3336=CIRCLE('',#36380,28.3018268963564);
#3337=CIRCLE('',#36382,28.3018268963564);
#3338=CIRCLE('',#36384,59.00430282);
#3339=CIRCLE('',#36386,28.3018268963564);
#3340=CIRCLE('',#36388,28.3018268963564);
#3341=CIRCLE('',#36390,59.00430282);
#3342=CIRCLE('',#36392,28.3018268963564);
#3343=CIRCLE('',#36394,28.3018268963564);
#3344=CIRCLE('',#36396,59.00430282);
#3345=CIRCLE('',#36398,28.3018268963564);
#3346=CIRCLE('',#36400,28.3018268963564);
#3347=CIRCLE('',#36402,59.00430282);
#3348=CIRCLE('',#36404,28.3018268963564);
#3349=CIRCLE('',#36406,28.3018268963564);
#3350=CIRCLE('',#36408,59.00430282);
#3351=CIRCLE('',#36410,28.3018268963564);
#3352=CIRCLE('',#36412,28.3018268963564);
#3353=CIRCLE('',#36414,59.00430282);
#3354=CIRCLE('',#36416,28.3018268963564);
#3355=CIRCLE('',#36418,28.3018268963564);
#3356=CIRCLE('',#36420,59.00430282);
#3357=CIRCLE('',#36422,28.3018268963564);
#3358=CIRCLE('',#36424,28.3018268963564);
#3359=CIRCLE('',#36426,59.00430282);
#3360=CIRCLE('',#36428,28.3018268963564);
#3361=CIRCLE('',#36430,28.3018268963564);
#3362=CIRCLE('',#36432,59.00430282);
#3363=CIRCLE('',#36434,28.3018268963564);
#3364=CIRCLE('',#36436,28.3018268963564);
#3365=CIRCLE('',#36438,59.00430282);
#3366=CIRCLE('',#36440,28.3018268963564);
#3367=CIRCLE('',#36442,28.3018268963564);
#3368=CIRCLE('',#36444,59.00430282);
#3369=CIRCLE('',#36446,28.3018268963564);
#3370=CIRCLE('',#36448,28.3018268963564);
#3371=CIRCLE('',#36450,59.00430282);
#3372=CIRCLE('',#36452,28.3018268963564);
#3373=CIRCLE('',#36454,28.3018268963564);
#3374=CIRCLE('',#36456,59.00430282);
#3375=CIRCLE('',#36458,28.3018268963564);
#3376=CIRCLE('',#36460,28.3018268963564);
#3377=CIRCLE('',#36462,59.00430282);
#3378=CIRCLE('',#36464,28.3018268963564);
#3379=CIRCLE('',#36466,28.3018268963564);
#3380=CIRCLE('',#36468,59.00430282);
#3381=CIRCLE('',#36470,28.3018268963564);
#3382=CIRCLE('',#36472,28.3018268963564);
#3383=CIRCLE('',#36474,59.00430282);
#3384=CIRCLE('',#36476,28.3018268963564);
#3385=CIRCLE('',#36478,28.3018268963564);
#3386=CIRCLE('',#36480,59.00430282);
#3387=CIRCLE('',#36482,28.3018268963564);
#3388=CIRCLE('',#36484,28.3018268963564);
#3389=CIRCLE('',#36486,59.00430282);
#3390=CIRCLE('',#36488,28.3018268963564);
#3391=CIRCLE('',#36490,28.3018268963564);
#3392=CIRCLE('',#36492,59.00430282);
#3393=CIRCLE('',#36494,28.3018268963564);
#3394=CIRCLE('',#36496,28.3018268963564);
#3395=CIRCLE('',#36498,59.00430282);
#3396=CIRCLE('',#36500,28.3018268963564);
#3397=CIRCLE('',#36502,28.3018268963564);
#3398=CIRCLE('',#36504,59.00430282);
#3399=CIRCLE('',#36506,28.3018268963564);
#3400=CIRCLE('',#36508,28.3018268963564);
#3401=CIRCLE('',#36510,59.00430282);
#3402=CIRCLE('',#36512,28.3018268963564);
#3403=CIRCLE('',#36514,28.3018268963564);
#3404=CIRCLE('',#36516,59.00430282);
#3405=CIRCLE('',#36518,28.3018268963564);
#3406=CIRCLE('',#36520,28.3018268963564);
#3407=CIRCLE('',#36522,59.00430282);
#3408=CIRCLE('',#36524,28.3018268963564);
#3409=CIRCLE('',#36526,28.3018268963564);
#3410=CIRCLE('',#36528,59.00430282);
#3411=CIRCLE('',#36530,28.3018268963564);
#3412=CIRCLE('',#36532,28.3018268963564);
#3413=CIRCLE('',#36534,59.00430282);
#3414=CIRCLE('',#36536,28.3018268963564);
#3415=CIRCLE('',#36538,28.3018268963564);
#3416=CIRCLE('',#36540,59.00430282);
#3417=CIRCLE('',#36542,28.3018268963564);
#3418=CIRCLE('',#36544,28.3018268963564);
#3419=CIRCLE('',#36546,59.00430282);
#3420=CIRCLE('',#36548,28.3018268963564);
#3421=CIRCLE('',#36550,28.3018268963564);
#3422=CIRCLE('',#36552,59.00430282);
#3423=CIRCLE('',#36554,28.3018268963564);
#3424=CIRCLE('',#36556,28.3018268963564);
#3425=CIRCLE('',#36558,59.00430282);
#3426=CIRCLE('',#36560,28.3018268963564);
#3427=CIRCLE('',#36562,28.3018268963564);
#3428=CIRCLE('',#36564,59.00430282);
#3429=CIRCLE('',#36566,28.3018268963564);
#3430=CIRCLE('',#36568,28.3018268963564);
#3431=CIRCLE('',#36570,59.00430282);
#3432=CIRCLE('',#36572,28.3018268963564);
#3433=CIRCLE('',#36574,28.3018268963564);
#3434=CIRCLE('',#36576,59.00430282);
#3435=CIRCLE('',#36578,28.3018268963564);
#3436=CIRCLE('',#36580,28.3018268963564);
#3437=CIRCLE('',#36582,59.00430282);
#3438=CIRCLE('',#36584,28.3018268963564);
#3439=CIRCLE('',#36586,28.3018268963564);
#3440=CIRCLE('',#36588,59.00430282);
#3441=CIRCLE('',#36590,28.3018268963564);
#3442=CIRCLE('',#36592,28.3018268963564);
#3443=CIRCLE('',#36594,59.00430282);
#3444=CIRCLE('',#36596,28.3018268963564);
#3445=CIRCLE('',#36598,28.3018268963564);
#3446=CIRCLE('',#36600,59.00430282);
#3447=CIRCLE('',#36602,28.3018268963564);
#3448=CIRCLE('',#36604,28.3018268963564);
#3449=CIRCLE('',#36606,59.00430282);
#3450=CIRCLE('',#36608,28.3018268963564);
#3451=CIRCLE('',#36610,28.3018268963564);
#3452=CIRCLE('',#36612,59.00430282);
#3453=CIRCLE('',#36614,28.3018268963564);
#3454=CIRCLE('',#36616,28.3018268963564);
#3455=CIRCLE('',#36618,59.00430282);
#3456=CIRCLE('',#36620,28.3018268963564);
#3457=CIRCLE('',#36622,28.3018268963564);
#3458=CIRCLE('',#36624,59.00430282);
#3459=CIRCLE('',#36626,28.3018268963564);
#3460=CIRCLE('',#36628,28.3018268963564);
#3461=CIRCLE('',#36630,59.00430282);
#3462=CIRCLE('',#36632,28.3018268963564);
#3463=CIRCLE('',#36634,28.3018268963564);
#3464=CIRCLE('',#36636,59.00430282);
#3465=CIRCLE('',#36638,28.3018268963564);
#3466=CIRCLE('',#36640,28.3018268963564);
#3467=CIRCLE('',#36642,64.5);
#3468=CIRCLE('',#36644,64.5);
#3469=CIRCLE('',#36646,64.5);
#3470=CIRCLE('',#36648,64.5);
#3471=CIRCLE('',#36650,64.5);
#3472=CIRCLE('',#36652,64.5);
#3473=CIRCLE('',#36654,64.5);
#3474=CIRCLE('',#36656,64.5);
#3475=CIRCLE('',#36658,64.5);
#3476=CIRCLE('',#36660,64.5);
#3477=CIRCLE('',#36662,64.5);
#3478=CIRCLE('',#36664,64.5);
#3479=CIRCLE('',#36666,64.5);
#3480=CIRCLE('',#36668,64.5);
#3481=CIRCLE('',#36670,64.5);
#3482=CIRCLE('',#36672,64.5);
#3483=CIRCLE('',#36674,64.5);
#3484=CIRCLE('',#36676,64.5);
#3485=CIRCLE('',#36678,64.5);
#3486=CIRCLE('',#36680,64.5);
#3487=CIRCLE('',#36682,64.5);
#3488=CIRCLE('',#36684,64.5);
#3489=CIRCLE('',#36686,64.5);
#3490=CIRCLE('',#36688,64.5);
#3491=CIRCLE('',#36690,64.5);
#3492=CIRCLE('',#36692,64.5);
#3493=CIRCLE('',#36694,64.5);
#3494=CIRCLE('',#36696,64.5);
#3495=CIRCLE('',#36698,64.5);
#3496=CIRCLE('',#36700,64.5);
#3497=CIRCLE('',#36702,64.5);
#3498=CIRCLE('',#36704,64.5);
#3499=CIRCLE('',#36706,64.5);
#3500=CIRCLE('',#36708,64.5);
#3501=CIRCLE('',#36710,64.5);
#3502=CIRCLE('',#36712,64.5);
#3503=CIRCLE('',#36714,64.5);
#3504=CIRCLE('',#36716,64.5);
#3505=CIRCLE('',#36718,64.5);
#3506=CIRCLE('',#36720,64.5);
#3507=CIRCLE('',#36722,64.5);
#3508=CIRCLE('',#36724,64.5);
#3509=CIRCLE('',#36726,64.5);
#3510=CIRCLE('',#36728,64.5);
#3511=CIRCLE('',#36730,64.5);
#3512=CIRCLE('',#36732,64.5);
#3513=CIRCLE('',#36734,64.5);
#3514=CIRCLE('',#36736,59.00430282);
#3515=CIRCLE('',#36738,28.3018268963564);
#3516=CIRCLE('',#36740,28.3018268963564);
#3517=CIRCLE('',#36742,64.5);
#3518=CIRCLE('',#36746,28.);
#3519=CIRCLE('',#36747,2.);
#3520=CIRCLE('',#36748,30.);
#3521=CIRCLE('',#36749,30.);
#3522=CIRCLE('',#36751,30.);
#3523=CIRCLE('',#36753,15.);
#3524=CIRCLE('',#36755,32.);
#3525=CIRCLE('',#36756,2.);
#3526=CIRCLE('',#36758,27.0484525317045);
#3527=CIRCLE('',#36759,46.875);
#3528=CIRCLE('',#36760,27.0484525317045);
#3529=CIRCLE('',#36761,52.37069718);
#3530=CIRCLE('',#36762,27.0484525317045);
#3531=CIRCLE('',#36763,46.875);
#3532=CIRCLE('',#36764,27.0484525317045);
#3533=CIRCLE('',#36765,52.37069718);
#3534=CIRCLE('',#36766,27.0484525317045);
#3535=CIRCLE('',#36767,46.875);
#3536=CIRCLE('',#36768,27.0484525317045);
#3537=CIRCLE('',#36769,52.37069718);
#3538=CIRCLE('',#36770,27.0484525317045);
#3539=CIRCLE('',#36771,46.875);
#3540=CIRCLE('',#36772,27.0484525317045);
#3541=CIRCLE('',#36773,52.37069718);
#3542=CIRCLE('',#36774,27.0484525317045);
#3543=CIRCLE('',#36775,46.875);
#3544=CIRCLE('',#36776,27.0484525317045);
#3545=CIRCLE('',#36777,52.37069718);
#3546=CIRCLE('',#36778,27.0484525317045);
#3547=CIRCLE('',#36779,46.875);
#3548=CIRCLE('',#36780,27.0484525317045);
#3549=CIRCLE('',#36781,52.37069718);
#3550=CIRCLE('',#36782,27.0484525317045);
#3551=CIRCLE('',#36783,46.875);
#3552=CIRCLE('',#36784,27.0484525317045);
#3553=CIRCLE('',#36785,52.37069718);
#3554=CIRCLE('',#36786,27.0484525317045);
#3555=CIRCLE('',#36787,46.875);
#3556=CIRCLE('',#36788,27.0484525317045);
#3557=CIRCLE('',#36789,52.37069718);
#3558=CIRCLE('',#36790,27.0484525317045);
#3559=CIRCLE('',#36791,46.875);
#3560=CIRCLE('',#36792,27.0484525317045);
#3561=CIRCLE('',#36793,52.37069718);
#3562=CIRCLE('',#36794,27.0484525317045);
#3563=CIRCLE('',#36795,46.875);
#3564=CIRCLE('',#36796,27.0484525317045);
#3565=CIRCLE('',#36797,52.37069718);
#3566=CIRCLE('',#36798,27.0484525317045);
#3567=CIRCLE('',#36799,46.875);
#3568=CIRCLE('',#36800,27.0484525317045);
#3569=CIRCLE('',#36801,52.37069718);
#3570=CIRCLE('',#36802,27.0484525317045);
#3571=CIRCLE('',#36803,46.875);
#3572=CIRCLE('',#36804,27.0484525317045);
#3573=CIRCLE('',#36805,52.37069718);
#3574=CIRCLE('',#36806,27.0484525317045);
#3575=CIRCLE('',#36807,46.875);
#3576=CIRCLE('',#36808,27.0484525317045);
#3577=CIRCLE('',#36809,52.37069718);
#3578=CIRCLE('',#36810,27.0484525317045);
#3579=CIRCLE('',#36811,46.875);
#3580=CIRCLE('',#36812,27.0484525317045);
#3581=CIRCLE('',#36813,52.37069718);
#3582=CIRCLE('',#36814,27.0484525317045);
#3583=CIRCLE('',#36815,46.875);
#3584=CIRCLE('',#36816,27.0484525317045);
#3585=CIRCLE('',#36817,52.37069718);
#3586=CIRCLE('',#36818,27.0484525317045);
#3587=CIRCLE('',#36819,46.875);
#3588=CIRCLE('',#36820,27.0484525317045);
#3589=CIRCLE('',#36821,52.37069718);
#3590=CIRCLE('',#36822,27.0484525317045);
#3591=CIRCLE('',#36823,46.875);
#3592=CIRCLE('',#36824,27.0484525317045);
#3593=CIRCLE('',#36825,52.37069718);
#3594=CIRCLE('',#36826,27.0484525317045);
#3595=CIRCLE('',#36827,46.875);
#3596=CIRCLE('',#36828,27.0484525317045);
#3597=CIRCLE('',#36829,52.37069718);
#3598=CIRCLE('',#36830,27.0484525317045);
#3599=CIRCLE('',#36831,46.875);
#3600=CIRCLE('',#36832,27.0484525317045);
#3601=CIRCLE('',#36833,52.37069718);
#3602=CIRCLE('',#36834,27.0484525317045);
#3603=CIRCLE('',#36835,46.875);
#3604=CIRCLE('',#36836,27.0484525317045);
#3605=CIRCLE('',#36837,52.37069718);
#3606=CIRCLE('',#36838,27.0484525317045);
#3607=CIRCLE('',#36839,46.875);
#3608=CIRCLE('',#36840,27.0484525317045);
#3609=CIRCLE('',#36841,52.37069718);
#3610=CIRCLE('',#36842,27.0484525317045);
#3611=CIRCLE('',#36843,46.875);
#3612=CIRCLE('',#36844,27.0484525317045);
#3613=CIRCLE('',#36845,52.37069718);
#3614=CIRCLE('',#36846,27.0484525317045);
#3615=CIRCLE('',#36847,46.875);
#3616=CIRCLE('',#36848,27.0484525317045);
#3617=CIRCLE('',#36849,52.37069718);
#3618=CIRCLE('',#36850,27.0484525317045);
#3619=CIRCLE('',#36851,46.875);
#3620=CIRCLE('',#36852,27.0484525317045);
#3621=CIRCLE('',#36853,52.37069718);
#3622=CIRCLE('',#36854,27.0484525317045);
#3623=CIRCLE('',#36855,46.875);
#3624=CIRCLE('',#36856,27.0484525317045);
#3625=CIRCLE('',#36857,52.37069718);
#3626=CIRCLE('',#36858,27.0484525317045);
#3627=CIRCLE('',#36859,46.875);
#3628=CIRCLE('',#36860,27.0484525317045);
#3629=CIRCLE('',#36861,52.37069718);
#3630=CIRCLE('',#36862,27.0484525317045);
#3631=CIRCLE('',#36863,46.875);
#3632=CIRCLE('',#36864,27.0484525317045);
#3633=CIRCLE('',#36865,52.37069718);
#3634=CIRCLE('',#36866,27.0484525317045);
#3635=CIRCLE('',#36867,46.875);
#3636=CIRCLE('',#36868,27.0484525317045);
#3637=CIRCLE('',#36869,52.37069718);
#3638=CIRCLE('',#36870,27.0484525317045);
#3639=CIRCLE('',#36871,46.875);
#3640=CIRCLE('',#36872,27.0484525317045);
#3641=CIRCLE('',#36873,52.37069718);
#3642=CIRCLE('',#36874,27.0484525317045);
#3643=CIRCLE('',#36875,46.875);
#3644=CIRCLE('',#36876,27.0484525317045);
#3645=CIRCLE('',#36877,52.37069718);
#3646=CIRCLE('',#36878,27.0484525317045);
#3647=CIRCLE('',#36879,46.875);
#3648=CIRCLE('',#36880,27.0484525317045);
#3649=CIRCLE('',#36881,52.37069718);
#3650=CIRCLE('',#36882,27.0484525317045);
#3651=CIRCLE('',#36883,46.875);
#3652=CIRCLE('',#36884,27.0484525317045);
#3653=CIRCLE('',#36885,52.37069718);
#3654=CIRCLE('',#36886,27.0484525317045);
#3655=CIRCLE('',#36887,46.875);
#3656=CIRCLE('',#36888,27.0484525317045);
#3657=CIRCLE('',#36889,52.37069718);
#3658=CIRCLE('',#36890,27.0484525317045);
#3659=CIRCLE('',#36891,46.875);
#3660=CIRCLE('',#36892,27.0484525317045);
#3661=CIRCLE('',#36893,52.37069718);
#3662=CIRCLE('',#36894,27.0484525317045);
#3663=CIRCLE('',#36895,46.875);
#3664=CIRCLE('',#36896,27.0484525317045);
#3665=CIRCLE('',#36897,52.37069718);
#3666=CIRCLE('',#36898,27.0484525317045);
#3667=CIRCLE('',#36899,46.875);
#3668=CIRCLE('',#36900,27.0484525317045);
#3669=CIRCLE('',#36901,52.37069718);
#3670=CIRCLE('',#36902,27.0484525317045);
#3671=CIRCLE('',#36903,46.875);
#3672=CIRCLE('',#36904,27.0484525317045);
#3673=CIRCLE('',#36905,52.37069718);
#3674=CIRCLE('',#36906,27.0484525317045);
#3675=CIRCLE('',#36907,46.875);
#3676=CIRCLE('',#36908,27.0484525317045);
#3677=CIRCLE('',#36909,52.37069718);
#3678=CIRCLE('',#36910,27.0484525317045);
#3679=CIRCLE('',#36911,46.875);
#3680=CIRCLE('',#36912,27.0484525317045);
#3681=CIRCLE('',#36913,52.37069718);
#3682=CIRCLE('',#36914,27.0484525317045);
#3683=CIRCLE('',#36915,46.875);
#3684=CIRCLE('',#36916,27.0484525317045);
#3685=CIRCLE('',#36917,52.37069718);
#3686=CIRCLE('',#36921,15.);
#3687=CIRCLE('',#36924,46.875);
#3688=CIRCLE('',#36926,27.0484525317045);
#3689=CIRCLE('',#36928,27.0484525317045);
#3690=CIRCLE('',#36930,46.875);
#3691=CIRCLE('',#36932,27.0484525317045);
#3692=CIRCLE('',#36934,27.0484525317045);
#3693=CIRCLE('',#36936,46.875);
#3694=CIRCLE('',#36938,27.0484525317045);
#3695=CIRCLE('',#36940,27.0484525317045);
#3696=CIRCLE('',#36942,46.875);
#3697=CIRCLE('',#36944,27.0484525317045);
#3698=CIRCLE('',#36946,27.0484525317045);
#3699=CIRCLE('',#36948,46.875);
#3700=CIRCLE('',#36950,27.0484525317045);
#3701=CIRCLE('',#36952,27.0484525317045);
#3702=CIRCLE('',#36954,46.875);
#3703=CIRCLE('',#36956,27.0484525317045);
#3704=CIRCLE('',#36958,27.0484525317045);
#3705=CIRCLE('',#36960,46.875);
#3706=CIRCLE('',#36962,27.0484525317045);
#3707=CIRCLE('',#36964,27.0484525317045);
#3708=CIRCLE('',#36966,46.875);
#3709=CIRCLE('',#36968,27.0484525317045);
#3710=CIRCLE('',#36970,27.0484525317045);
#3711=CIRCLE('',#36972,46.875);
#3712=CIRCLE('',#36974,27.0484525317045);
#3713=CIRCLE('',#36976,27.0484525317045);
#3714=CIRCLE('',#36978,46.875);
#3715=CIRCLE('',#36980,27.0484525317045);
#3716=CIRCLE('',#36982,27.0484525317045);
#3717=CIRCLE('',#36984,46.875);
#3718=CIRCLE('',#36986,27.0484525317045);
#3719=CIRCLE('',#36988,27.0484525317045);
#3720=CIRCLE('',#36990,46.875);
#3721=CIRCLE('',#36992,27.0484525317045);
#3722=CIRCLE('',#36994,27.0484525317045);
#3723=CIRCLE('',#36996,46.875);
#3724=CIRCLE('',#36998,27.0484525317045);
#3725=CIRCLE('',#37000,27.0484525317045);
#3726=CIRCLE('',#37002,46.875);
#3727=CIRCLE('',#37004,27.0484525317045);
#3728=CIRCLE('',#37006,27.0484525317045);
#3729=CIRCLE('',#37008,46.875);
#3730=CIRCLE('',#37010,27.0484525317045);
#3731=CIRCLE('',#37012,27.0484525317045);
#3732=CIRCLE('',#37014,46.875);
#3733=CIRCLE('',#37016,27.0484525317045);
#3734=CIRCLE('',#37018,27.0484525317045);
#3735=CIRCLE('',#37020,46.875);
#3736=CIRCLE('',#37022,27.0484525317045);
#3737=CIRCLE('',#37024,27.0484525317045);
#3738=CIRCLE('',#37026,46.875);
#3739=CIRCLE('',#37028,27.0484525317045);
#3740=CIRCLE('',#37030,27.0484525317045);
#3741=CIRCLE('',#37032,46.875);
#3742=CIRCLE('',#37034,27.0484525317045);
#3743=CIRCLE('',#37036,27.0484525317045);
#3744=CIRCLE('',#37038,46.875);
#3745=CIRCLE('',#37040,27.0484525317045);
#3746=CIRCLE('',#37042,27.0484525317045);
#3747=CIRCLE('',#37044,46.875);
#3748=CIRCLE('',#37046,27.0484525317045);
#3749=CIRCLE('',#37048,27.0484525317045);
#3750=CIRCLE('',#37050,46.875);
#3751=CIRCLE('',#37052,27.0484525317045);
#3752=CIRCLE('',#37054,27.0484525317045);
#3753=CIRCLE('',#37056,46.875);
#3754=CIRCLE('',#37058,27.0484525317045);
#3755=CIRCLE('',#37060,27.0484525317045);
#3756=CIRCLE('',#37062,46.875);
#3757=CIRCLE('',#37064,27.0484525317045);
#3758=CIRCLE('',#37066,27.0484525317045);
#3759=CIRCLE('',#37068,46.875);
#3760=CIRCLE('',#37070,27.0484525317045);
#3761=CIRCLE('',#37072,27.0484525317045);
#3762=CIRCLE('',#37074,46.875);
#3763=CIRCLE('',#37076,27.0484525317045);
#3764=CIRCLE('',#37078,27.0484525317045);
#3765=CIRCLE('',#37080,46.875);
#3766=CIRCLE('',#37082,27.0484525317045);
#3767=CIRCLE('',#37084,27.0484525317045);
#3768=CIRCLE('',#37086,46.875);
#3769=CIRCLE('',#37088,27.0484525317045);
#3770=CIRCLE('',#37090,27.0484525317045);
#3771=CIRCLE('',#37092,46.875);
#3772=CIRCLE('',#37094,27.0484525317045);
#3773=CIRCLE('',#37096,27.0484525317045);
#3774=CIRCLE('',#37098,46.875);
#3775=CIRCLE('',#37100,27.0484525317045);
#3776=CIRCLE('',#37102,27.0484525317045);
#3777=CIRCLE('',#37104,46.875);
#3778=CIRCLE('',#37106,27.0484525317045);
#3779=CIRCLE('',#37108,27.0484525317045);
#3780=CIRCLE('',#37110,46.875);
#3781=CIRCLE('',#37112,27.0484525317045);
#3782=CIRCLE('',#37114,27.0484525317045);
#3783=CIRCLE('',#37116,46.875);
#3784=CIRCLE('',#37118,27.0484525317045);
#3785=CIRCLE('',#37120,27.0484525317045);
#3786=CIRCLE('',#37122,46.875);
#3787=CIRCLE('',#37124,27.0484525317045);
#3788=CIRCLE('',#37126,27.0484525317045);
#3789=CIRCLE('',#37128,46.875);
#3790=CIRCLE('',#37130,27.0484525317045);
#3791=CIRCLE('',#37132,27.0484525317045);
#3792=CIRCLE('',#37134,46.875);
#3793=CIRCLE('',#37136,27.0484525317045);
#3794=CIRCLE('',#37138,27.0484525317045);
#3795=CIRCLE('',#37140,46.875);
#3796=CIRCLE('',#37142,27.0484525317045);
#3797=CIRCLE('',#37144,27.0484525317045);
#3798=CIRCLE('',#37146,46.875);
#3799=CIRCLE('',#37148,27.0484525317045);
#3800=CIRCLE('',#37150,27.0484525317045);
#3801=CIRCLE('',#37152,46.875);
#3802=CIRCLE('',#37154,27.0484525317045);
#3803=CIRCLE('',#37156,27.0484525317045);
#3804=CIRCLE('',#37158,52.37069718);
#3805=CIRCLE('',#37160,52.37069718);
#3806=CIRCLE('',#37162,52.37069718);
#3807=CIRCLE('',#37164,52.37069718);
#3808=CIRCLE('',#37166,52.37069718);
#3809=CIRCLE('',#37168,52.37069718);
#3810=CIRCLE('',#37170,52.37069718);
#3811=CIRCLE('',#37172,52.37069718);
#3812=CIRCLE('',#37174,52.37069718);
#3813=CIRCLE('',#37176,52.37069718);
#3814=CIRCLE('',#37178,52.37069718);
#3815=CIRCLE('',#37180,52.37069718);
#3816=CIRCLE('',#37182,52.37069718);
#3817=CIRCLE('',#37184,52.37069718);
#3818=CIRCLE('',#37186,52.37069718);
#3819=CIRCLE('',#37188,52.37069718);
#3820=CIRCLE('',#37190,52.37069718);
#3821=CIRCLE('',#37192,52.37069718);
#3822=CIRCLE('',#37194,52.37069718);
#3823=CIRCLE('',#37196,52.37069718);
#3824=CIRCLE('',#37198,52.37069718);
#3825=CIRCLE('',#37200,52.37069718);
#3826=CIRCLE('',#37202,52.37069718);
#3827=CIRCLE('',#37204,52.37069718);
#3828=CIRCLE('',#37206,52.37069718);
#3829=CIRCLE('',#37208,52.37069718);
#3830=CIRCLE('',#37210,52.37069718);
#3831=CIRCLE('',#37212,52.37069718);
#3832=CIRCLE('',#37214,52.37069718);
#3833=CIRCLE('',#37216,52.37069718);
#3834=CIRCLE('',#37218,52.37069718);
#3835=CIRCLE('',#37220,52.37069718);
#3836=CIRCLE('',#37222,52.37069718);
#3837=CIRCLE('',#37224,52.37069718);
#3838=CIRCLE('',#37226,52.37069718);
#3839=CIRCLE('',#37228,52.37069718);
#3840=CIRCLE('',#37230,52.37069718);
#3841=CIRCLE('',#37232,52.37069718);
#3842=CIRCLE('',#37234,52.37069718);
#3843=CIRCLE('',#37236,46.875);
#3844=CIRCLE('',#37238,27.0484525317045);
#3845=CIRCLE('',#37240,27.0484525317045);
#3846=CIRCLE('',#37242,52.37069718);
#3847=CIRCLE('',#37249,3.22047616);
#3848=CIRCLE('',#37250,3.22047616);
#3849=CIRCLE('',#37251,3.15163199999999);
#3850=CIRCLE('',#37254,3.22047616);
#3851=CIRCLE('',#37255,3.22047616);
#3852=CIRCLE('',#37258,3.9116);
#3853=CIRCLE('',#37259,3.9116);
#3854=CIRCLE('',#37261,4.19099999999999);
#3855=CIRCLE('',#37263,4.19100000000001);
#3856=CIRCLE('',#37266,3.22047616);
#3857=CIRCLE('',#37267,3.22047616);
#3858=CIRCLE('',#37268,3.151632);
#3859=CIRCLE('',#37271,3.22047616000001);
#3860=CIRCLE('',#37272,3.22047616000001);
#3861=CIRCLE('',#37275,3.9116);
#3862=CIRCLE('',#37276,3.9116);
#3863=CIRCLE('',#37278,4.19099999999999);
#3864=CIRCLE('',#37280,4.191);
#3865=CIRCLE('',#37283,2.74750784);
#3866=CIRCLE('',#37284,2.68671039999999);
#3867=CIRCLE('',#37285,2.74750784);
#3868=CIRCLE('',#37288,2.74750784);
#3869=CIRCLE('',#37289,2.74750784);
#3870=CIRCLE('',#37292,3.3528);
#3871=CIRCLE('',#37293,3.35280000000001);
#3872=CIRCLE('',#37295,3.6322);
#3873=CIRCLE('',#37297,3.6322);
#3874=CIRCLE('',#37300,3.9116);
#3875=CIRCLE('',#37301,3.9116);
#3876=CIRCLE('',#37303,4.191);
#3877=CIRCLE('',#37305,4.19099999999999);
#3878=CIRCLE('',#37308,3.22047616);
#3879=CIRCLE('',#37309,3.22047616);
#3880=CIRCLE('',#37310,3.15163200000001);
#3881=CIRCLE('',#37313,3.22047616);
#3882=CIRCLE('',#37314,3.22047616);
#3883=CIRCLE('',#37317,3.9116);
#3884=CIRCLE('',#37318,3.9116);
#3885=CIRCLE('',#37320,4.191);
#3886=CIRCLE('',#37322,4.191);
#3887=CIRCLE('',#37325,3.22047616000001);
#3888=CIRCLE('',#37326,3.22047616000001);
#3889=CIRCLE('',#37327,3.151632);
#3890=CIRCLE('',#37330,3.22047616);
#3891=CIRCLE('',#37331,3.22047616);
#3892=CIRCLE('',#37335,62.3964875794553);
#3893=CIRCLE('',#37336,60.8301548187703);
#3894=CIRCLE('',#37339,62.3964875794704);
#3895=CIRCLE('',#37340,60.8301548187776);
#3896=CIRCLE('',#37344,13.9758160535843);
#3897=CIRCLE('',#37346,13.9758160535819);
#3898=CIRCLE('',#37349,17.7292483264849);
#3899=CIRCLE('',#37350,17.729248326485);
#3900=CIRCLE('',#37351,17.7292483264851);
#3901=CIRCLE('',#37352,17.7292483264851);
#3902=CIRCLE('',#37353,30.1930816);
#3903=CIRCLE('',#37355,4.70822528);
#3904=CIRCLE('',#37356,4.70822528);
#3905=CIRCLE('',#37357,4.70822528);
#3906=CIRCLE('',#37361,4.70822528);
#3907=CIRCLE('',#37362,4.70822528);
#3908=CIRCLE('',#37363,4.70822528000005);
#3909=CIRCLE('',#37365,4.70822528);
#3910=CIRCLE('',#37366,4.70822528);
#3911=CIRCLE('',#37373,4.70822528000005);
#3912=CIRCLE('',#37374,4.70822528000005);
#3913=CIRCLE('',#37378,4.70822527999999);
#3914=CIRCLE('',#37379,4.70822527999999);
#3915=CIRCLE('',#37384,5.87573292967013);
#3916=CIRCLE('',#37386,28.8698432);
#3917=CIRCLE('',#37387,28.8698432);
#3918=CIRCLE('',#37388,28.8698432);
#3919=CIRCLE('',#37389,28.8698432);
#3920=CIRCLE('',#37393,28.8519616);
#3921=CIRCLE('',#37394,28.8519616);
#3922=CIRCLE('',#37395,28.8519616);
#3923=CIRCLE('',#37405,27.9578816);
#3924=CIRCLE('',#37407,21.82583392);
#3925=CIRCLE('',#37409,4.70822527999999);
#3926=CIRCLE('',#37410,4.70822527999999);
#3927=CIRCLE('',#37411,4.70822528);
#3928=CIRCLE('',#37413,4.70822528);
#3929=CIRCLE('',#37414,4.70822528);
#3930=CIRCLE('',#37415,4.70822528);
#3931=CIRCLE('',#37417,4.70822528);
#3932=CIRCLE('',#37418,4.70822528);
#3933=CIRCLE('',#37419,4.70822528);
#3934=CIRCLE('',#37421,4.70822528);
#3935=CIRCLE('',#37422,4.70822528);
#3936=CIRCLE('',#37423,4.70822528);
#3937=CIRCLE('',#37428,5.87573292967001);
#3938=CIRCLE('',#37429,5.87573292967001);
#3939=CIRCLE('',#37431,14.6657199888249);
#3940=CIRCLE('',#37433,22.5);
#3941=CIRCLE('',#37434,22.5);
#3942=CIRCLE('',#37441,5.64835039999983);
#3943=CIRCLE('',#37443,5.6483504000001);
#3944=CIRCLE('',#37445,5.64835039999984);
#3945=CIRCLE('',#37447,5.64835040000001);
#3946=CIRCLE('',#37449,5.64835039999994);
#3947=CIRCLE('',#37453,5.64835039999982);
#3948=CIRCLE('',#37460,5.64835040000232);
#3949=CIRCLE('',#37462,5.64835039999654);
#3950=CIRCLE('',#37464,5.64835040000021);
#3951=CIRCLE('',#37466,5.64835039999982);
#3952=CIRCLE('',#37468,5.64835040000023);
#3953=CIRCLE('',#37472,5.64835040000259);
#3954=CIRCLE('',#37487,5.17762544927992);
#3955=CIRCLE('',#37489,5.17762544927979);
#3956=CIRCLE('',#37498,5.17762544928);
#3957=CIRCLE('',#37508,5.17762544927989);
#3958=CIRCLE('',#37514,5.44243151077326);
#3959=CIRCLE('',#37517,2.74750784);
#3960=CIRCLE('',#37518,2.74750784);
#3961=CIRCLE('',#37520,2.74750784);
#3962=CIRCLE('',#37521,2.74750784);
#3963=CIRCLE('',#37523,3.35280000000001);
#3964=CIRCLE('',#37525,2.74750784);
#3965=CIRCLE('',#37526,2.74750784);
#3966=CIRCLE('',#37528,2.74750784000001);
#3967=CIRCLE('',#37529,2.74750784000001);
#3968=CIRCLE('',#37531,3.3528);
#3969=CIRCLE('',#37533,2.74750784);
#3970=CIRCLE('',#37534,2.74750784);
#3971=CIRCLE('',#37536,2.74750784000001);
#3972=CIRCLE('',#37537,2.74750784000001);
#3973=CIRCLE('',#37539,3.3528);
#3974=CIRCLE('',#37541,3.22047616000005);
#3975=CIRCLE('',#37542,3.22047616000005);
#3976=CIRCLE('',#37543,3.9116);
#3977=CIRCLE('',#37545,3.22047616000005);
#3978=CIRCLE('',#37546,3.22047616000005);
#3979=CIRCLE('',#37549,3.22047616);
#3980=CIRCLE('',#37550,3.22047616);
#3981=CIRCLE('',#37551,3.9116);
#3982=CIRCLE('',#37553,3.22047616);
#3983=CIRCLE('',#37554,3.22047616);
#3984=CIRCLE('',#37557,3.22047616000005);
#3985=CIRCLE('',#37558,3.22047616000005);
#3986=CIRCLE('',#37559,3.9116);
#3987=CIRCLE('',#37561,3.22047616000005);
#3988=CIRCLE('',#37562,3.22047616000005);
#3989=CIRCLE('',#37565,3.22047616000001);
#3990=CIRCLE('',#37566,3.22047616000001);
#3991=CIRCLE('',#37567,3.9116);
#3992=CIRCLE('',#37569,3.22047616000001);
#3993=CIRCLE('',#37570,3.22047616000001);
#3994=CIRCLE('',#37590,67.056);
#3995=CIRCLE('',#37591,46.9481408);
#3996=CIRCLE('',#37593,46.9481408);
#3997=CIRCLE('',#37595,46.9481408);
#3998=CIRCLE('',#37596,47.4643381286771);
#3999=CIRCLE('',#37597,46.9481408);
#4000=CIRCLE('',#37611,67.056);
#4001=CIRCLE('',#37612,67.056);
#4002=CIRCLE('',#37613,67.6754367944125);
#4003=CIRCLE('',#37616,29.386040528677);
#4004=CIRCLE('',#37621,46.9481408);
#4005=CIRCLE('',#37622,46.9481408);
#4006=CIRCLE('',#37624,46.9481408);
#4007=CIRCLE('',#37625,46.9481408);
#4008=CIRCLE('',#37626,47.4643381286771);
#4009=CIRCLE('',#37629,67.0291776);
#4010=CIRCLE('',#37631,67.0291776000001);
#4011=CIRCLE('',#37634,2.74750784);
#4012=CIRCLE('',#37635,2.74750784);
#4013=CIRCLE('',#37636,2.74750784);
#4014=CIRCLE('',#37638,37.9894592000001);
#4015=CIRCLE('',#37639,37.9894592000001);
#4016=CIRCLE('',#37640,37.3700224055875);
#4017=CIRCLE('',#37642,14.6657199888249);
#4018=CIRCLE('',#37644,13.4268464);
#4019=CIRCLE('',#37646,28.7097683677432);
#4020=CIRCLE('',#37648,13.4268464);
#4021=CIRCLE('',#37650,2.74750784);
#4022=CIRCLE('',#37651,2.74750784);
#4023=CIRCLE('',#37652,2.74750784);
#4024=CIRCLE('',#37669,2.68671040000002);
#4025=CIRCLE('',#37671,3.35279999999999);
#4026=CIRCLE('',#37672,3.35279999999999);
#4027=CIRCLE('',#37675,2.74750783999999);
#4028=CIRCLE('',#37676,2.74750783999999);
#4029=CIRCLE('',#37677,2.6867104);
#4030=CIRCLE('',#37680,2.68671040000002);
#4031=CIRCLE('',#37682,3.3528);
#4032=CIRCLE('',#37683,3.3528);
#4033=CIRCLE('',#37699,2.6867104);
#4034=CIRCLE('',#37701,3.35279999999998);
#4035=CIRCLE('',#37702,3.35279999999998);
#4036=CIRCLE('',#37705,2.74750783999999);
#4037=CIRCLE('',#37706,2.74750783999999);
#4038=CIRCLE('',#37707,2.6867104);
#4039=CIRCLE('',#37710,2.6867104);
#4040=CIRCLE('',#37712,3.3528);
#4041=CIRCLE('',#37713,3.3528);
#4042=CIRCLE('',#37716,2.6867104);
#4043=CIRCLE('',#37721,2.6867104);
#4044=CIRCLE('',#37725,37.9894592000001);
#4045=CIRCLE('',#37726,37.9894592000001);
#4046=CIRCLE('',#37727,37.9894592);
#4047=CIRCLE('',#37733,37.9894592);
#4048=CIRCLE('',#37735,37.9894592);
#4049=CIRCLE('',#37737,46.9481408);
#4050=CIRCLE('',#37740,37.9894592);
#4051=CIRCLE('',#37743,46.9481408);
#4052=CIRCLE('',#37746,5.64835039999681);
#4053=CIRCLE('',#37747,5.64835040000208);
#4054=CIRCLE('',#37748,5.64835039999998);
#4055=CIRCLE('',#37749,5.64835040000009);
#4056=CIRCLE('',#37750,5.64835040000009);
#4057=CIRCLE('',#37751,5.64835040000243);
#4058=CIRCLE('',#37765,5.64835039999982);
#4059=CIRCLE('',#37766,5.64835040000004);
#4060=CIRCLE('',#37767,5.64835040000006);
#4061=CIRCLE('',#37768,5.64835039999973);
#4062=CIRCLE('',#37769,5.64835039999998);
#4063=CIRCLE('',#37770,5.64835039999987);
#4064=CIRCLE('',#37784,3.63220000000001);
#4065=CIRCLE('',#37786,3.6322);
#4066=CIRCLE('',#37788,3.63220000000001);
#4067=CIRCLE('',#37790,2.74750784);
#4068=CIRCLE('',#37791,2.74750784);
#4069=CIRCLE('',#37793,2.74750784);
#4070=CIRCLE('',#37794,2.74750784);
#4071=CIRCLE('',#37796,21.82583392);
#4072=CIRCLE('',#37798,3.6322);
#4073=CIRCLE('',#37799,3.6322);
#4074=CIRCLE('',#37801,3.6322);
#4075=CIRCLE('',#37802,3.6322);
#4076=CIRCLE('',#37804,3.6322);
#4077=CIRCLE('',#37805,3.6322);
#4078=CIRCLE('',#37807,3.6322);
#4079=CIRCLE('',#37808,3.6322);
#4080=CIRCLE('',#37810,45.0616320000016);
#4081=CIRCLE('',#37811,2.14579199999995);
#4082=CIRCLE('',#37812,2.14579200000003);
#4083=CIRCLE('',#37813,55.4329599999972);
#4084=CIRCLE('',#37814,2.14579200000022);
#4085=CIRCLE('',#37815,2.14579200000003);
#4086=CIRCLE('',#37818,2.14579200000017);
#4087=CIRCLE('',#37819,2.14579200000006);
#4088=CIRCLE('',#37821,55.4329599999999);
#4089=CIRCLE('',#37822,55.4329599999999);
#4090=CIRCLE('',#37824,2.14579200000009);
#4091=CIRCLE('',#37825,2.14579199999991);
#4092=CIRCLE('',#37828,2.14579200000003);
#4093=CIRCLE('',#37829,2.14579200000003);
#4094=CIRCLE('',#37831,45.0616320000003);
#4095=CIRCLE('',#37832,45.0616320000003);
#4096=CIRCLE('',#37834,2.14579199999998);
#4097=CIRCLE('',#37835,2.14579199999998);
#4098=CIRCLE('',#37839,2.14579200000001);
#4099=CIRCLE('',#37840,2.14579200000002);
#4100=CIRCLE('',#37842,55.4329600000002);
#4101=CIRCLE('',#37843,55.4329600000002);
#4102=CIRCLE('',#37845,2.14579200000004);
#4103=CIRCLE('',#37846,2.14579200000004);
#4104=CIRCLE('',#37849,2.1457919999999);
#4105=CIRCLE('',#37850,2.14579200000004);
#4106=CIRCLE('',#37852,45.0616320000005);
#4107=CIRCLE('',#37853,45.0616320000005);
#4108=CIRCLE('',#37855,2.14579199999994);
#4109=CIRCLE('',#37856,2.14579199999996);
#4110=CIRCLE('',#37860,2.14579200000037);
#4111=CIRCLE('',#37861,2.14579200000037);
#4112=CIRCLE('',#37863,55.432960000001);
#4113=CIRCLE('',#37864,55.432960000001);
#4114=CIRCLE('',#37866,2.14579200000004);
#4115=CIRCLE('',#37867,2.14579200000016);
#4116=CIRCLE('',#37870,2.14579199999993);
#4117=CIRCLE('',#37871,2.14579200000008);
#4118=CIRCLE('',#37873,45.0616319999978);
#4119=CIRCLE('',#37874,45.0616319999978);
#4120=CIRCLE('',#37876,2.14579200000014);
#4121=CIRCLE('',#37877,2.14579200000014);
#4122=CIRCLE('',#37880,3.6322);
#4123=CIRCLE('',#37882,3.6322);
#4124=CIRCLE('',#37884,3.6322);
#4125=CIRCLE('',#37886,40.2514816);
#4126=CIRCLE('',#37888,40.2514816000002);
#4127=CIRCLE('',#37892,40.2514816000021);
#4128=CIRCLE('',#37893,1249.18823030311);
#4129=CIRCLE('',#37894,40.2514815999989);
#4130=CIRCLE('',#37895,1249.18823049325);
#4131=CIRCLE('',#37899,40.2514815999998);
#4132=CIRCLE('',#37901,40.2514815999992);
#4133=CIRCLE('',#37904,8.94079999999999);
#4134=CIRCLE('',#37905,8.5349144993668);
#4135=CIRCLE('',#37907,8.53491449936691);
#4136=CIRCLE('',#37908,8.94079999999999);
#4137=CIRCLE('',#37910,8.5349144993666);
#4138=CIRCLE('',#37911,8.9408);
#4139=CIRCLE('',#37912,4.91296959999996);
#4140=CIRCLE('',#37914,58.1152000000001);
#4141=CIRCLE('',#37915,58.0210179209497);
#4142=CIRCLE('',#37916,58.0210179209497);
#4143=CIRCLE('',#37923,8.94080000000002);
#4144=CIRCLE('',#37926,8.94079999999995);
#4145=CIRCLE('',#37929,8.53491449936659);
#4146=CIRCLE('',#37930,8.94079999999992);
#4147=CIRCLE('',#37932,1249.18889184763);
#4148=CIRCLE('',#37933,1249.18889156446);
#4149=CIRCLE('',#37935,8.94080000000007);
#4150=CIRCLE('',#37937,8.94079999999999);
#4151=CIRCLE('',#37938,8.94079999999999);
#4152=CIRCLE('',#37939,8.94080000000001);
#4153=CIRCLE('',#37940,8.94079999999999);
#4154=CIRCLE('',#37943,8.94079999999999);
#4155=CIRCLE('',#37956,40.2514816000013);
#4156=CIRCLE('',#37957,40.2514815999992);
#4157=CIRCLE('',#37960,2.14579200000002);
#4158=CIRCLE('',#37961,2.14579200000014);
#4159=CIRCLE('',#37964,2.14579199999958);
#4160=CIRCLE('',#37965,2.14579199999958);
#4161=CIRCLE('',#37967,45.0616320000041);
#4162=CIRCLE('',#37968,45.061632000004);
#4163=CIRCLE('',#37970,2.14579200000037);
#4164=CIRCLE('',#37971,2.14579200000037);
#4165=CIRCLE('',#37974,2.14579200000006);
#4166=CIRCLE('',#37975,2.14579200000006);
#4167=CIRCLE('',#37977,55.4329600000085);
#4168=CIRCLE('',#37978,55.4329600000085);
#4169=CIRCLE('',#37982,2.14579200000079);
#4170=CIRCLE('',#37983,2.14579200000084);
#4171=CIRCLE('',#37985,45.0616319999978);
#4172=CIRCLE('',#37986,45.0616319999971);
#4173=CIRCLE('',#37988,2.14579199999999);
#4174=CIRCLE('',#37989,2.14579199999999);
#4175=CIRCLE('',#37992,2.14579200000036);
#4176=CIRCLE('',#37993,2.14579200000036);
#4177=CIRCLE('',#37995,55.4329600000016);
#4178=CIRCLE('',#37996,55.4329600000016);
#4179=CIRCLE('',#37998,2.14579199999924);
#4180=CIRCLE('',#37999,2.14579199999924);
#4181=CIRCLE('',#38002,55.4329599999945);
#4182=CIRCLE('',#38003,55.4329599999945);
#4183=CIRCLE('',#38005,2.1457919999994);
#4184=CIRCLE('',#38006,2.1457919999994);
#4185=CIRCLE('',#38009,2.14579200000024);
#4186=CIRCLE('',#38010,2.14579200000024);
#4187=CIRCLE('',#38012,45.0616320000037);
#4188=CIRCLE('',#38013,45.0616320000037);
#4189=CIRCLE('',#38015,2.1457919999996);
#4190=CIRCLE('',#38016,2.1457919999996);
#4191=CIRCLE('',#38019,2.14579200000019);
#4192=CIRCLE('',#38020,2.14579200000016);
#4193=CIRCLE('',#38023,55.4329599999988);
#4194=CIRCLE('',#38024,55.432959999998);
#4195=CIRCLE('',#38026,2.1457920000003);
#4196=CIRCLE('',#38027,2.1457920000003);
#4197=CIRCLE('',#38030,2.14579200000034);
#4198=CIRCLE('',#38031,2.14579200000023);
#4199=CIRCLE('',#38033,45.0616319999981);
#4200=CIRCLE('',#38034,45.0616319999962);
#4201=CIRCLE('',#38036,2.14579199999954);
#4202=CIRCLE('',#38037,2.14579199999954);
#4203=CIRCLE('',#38040,2.14579199999923);
#4204=CIRCLE('',#38041,2.14579199999923);
#4205=CIRCLE('',#38044,45.0616320000016);
#4206=CIRCLE('',#38046,2.14579200000003);
#4207=CIRCLE('',#38049,2.14579200000008);
#4208=CIRCLE('',#38051,55.4329599999972);
#4209=CIRCLE('',#38053,2.14579200000014);
#4210=CIRCLE('',#38055,2.14579199999995);
#4211=CIRCLE('',#38058,1.78815999999988);
#4212=CIRCLE('',#38059,56.2331302663788);
#4213=CIRCLE('',#38072,5.0247296);
#4214=CIRCLE('',#38073,5.0247296);
#4215=CIRCLE('',#38074,4.5776896);
#4216=CIRCLE('',#38076,5.0247296);
#4217=CIRCLE('',#38077,5.0247296);
#4218=CIRCLE('',#38089,12.);
#4219=CIRCLE('',#38090,12.);
#4220=CIRCLE('',#38096,22.5);
#4221=CIRCLE('',#38098,22.5);
#4222=CIRCLE('',#38100,25.);
#4223=CIRCLE('',#38101,25.);
#4224=CIRCLE('',#38102,25.);
#4225=CIRCLE('',#38103,25.);
#4226=CIRCLE('',#38105,20.);
#4227=CIRCLE('',#38108,35.);
#4228=CIRCLE('',#38109,35.);
#4229=CIRCLE('',#38110,29.9999999999998);
#4230=CIRCLE('',#38112,35.0000000000001);
#4231=CIRCLE('',#38113,35.0000000000001);
#4232=FACE_OUTER_BOUND('',#6110,.T.);
#4233=FACE_OUTER_BOUND('',#6111,.T.);
#4234=FACE_OUTER_BOUND('',#6112,.T.);
#4235=FACE_OUTER_BOUND('',#6113,.T.);
#4236=FACE_OUTER_BOUND('',#6115,.T.);
#4237=FACE_OUTER_BOUND('',#6116,.T.);
#4238=FACE_OUTER_BOUND('',#6117,.T.);
#4239=FACE_OUTER_BOUND('',#6118,.T.);
#4240=FACE_OUTER_BOUND('',#6119,.T.);
#4241=FACE_OUTER_BOUND('',#6120,.T.);
#4242=FACE_OUTER_BOUND('',#6121,.T.);
#4243=FACE_OUTER_BOUND('',#6122,.T.);
#4244=FACE_OUTER_BOUND('',#6123,.T.);
#4245=FACE_OUTER_BOUND('',#6124,.T.);
#4246=FACE_OUTER_BOUND('',#6125,.T.);
#4247=FACE_OUTER_BOUND('',#6126,.T.);
#4248=FACE_OUTER_BOUND('',#6127,.T.);
#4249=FACE_OUTER_BOUND('',#6128,.T.);
#4250=FACE_OUTER_BOUND('',#6129,.T.);
#4251=FACE_OUTER_BOUND('',#6130,.T.);
#4252=FACE_OUTER_BOUND('',#6131,.T.);
#4253=FACE_OUTER_BOUND('',#6133,.T.);
#4254=FACE_OUTER_BOUND('',#6139,.T.);
#4255=FACE_OUTER_BOUND('',#6140,.T.);
#4256=FACE_OUTER_BOUND('',#6141,.T.);
#4257=FACE_OUTER_BOUND('',#6142,.T.);
#4258=FACE_OUTER_BOUND('',#6144,.T.);
#4259=FACE_OUTER_BOUND('',#6146,.T.);
#4260=FACE_OUTER_BOUND('',#6148,.T.);
#4261=FACE_OUTER_BOUND('',#6150,.T.);
#4262=FACE_OUTER_BOUND('',#6151,.T.);
#4263=FACE_OUTER_BOUND('',#6152,.T.);
#4264=FACE_OUTER_BOUND('',#6153,.T.);
#4265=FACE_OUTER_BOUND('',#6154,.T.);
#4266=FACE_OUTER_BOUND('',#6155,.T.);
#4267=FACE_OUTER_BOUND('',#6156,.T.);
#4268=FACE_OUTER_BOUND('',#6157,.T.);
#4269=FACE_OUTER_BOUND('',#6158,.T.);
#4270=FACE_OUTER_BOUND('',#6159,.T.);
#4271=FACE_OUTER_BOUND('',#6160,.T.);
#4272=FACE_OUTER_BOUND('',#6161,.T.);
#4273=FACE_OUTER_BOUND('',#6162,.T.);
#4274=FACE_OUTER_BOUND('',#6163,.T.);
#4275=FACE_OUTER_BOUND('',#6164,.T.);
#4276=FACE_OUTER_BOUND('',#6165,.T.);
#4277=FACE_OUTER_BOUND('',#6166,.T.);
#4278=FACE_OUTER_BOUND('',#6167,.T.);
#4279=FACE_OUTER_BOUND('',#6168,.T.);
#4280=FACE_OUTER_BOUND('',#6169,.T.);
#4281=FACE_OUTER_BOUND('',#6170,.T.);
#4282=FACE_OUTER_BOUND('',#6171,.T.);
#4283=FACE_OUTER_BOUND('',#6172,.T.);
#4284=FACE_OUTER_BOUND('',#6173,.T.);
#4285=FACE_OUTER_BOUND('',#6174,.T.);
#4286=FACE_OUTER_BOUND('',#6175,.T.);
#4287=FACE_OUTER_BOUND('',#6176,.T.);
#4288=FACE_OUTER_BOUND('',#6177,.T.);
#4289=FACE_OUTER_BOUND('',#6178,.T.);
#4290=FACE_OUTER_BOUND('',#6179,.T.);
#4291=FACE_OUTER_BOUND('',#6180,.T.);
#4292=FACE_OUTER_BOUND('',#6181,.T.);
#4293=FACE_OUTER_BOUND('',#6182,.T.);
#4294=FACE_OUTER_BOUND('',#6183,.T.);
#4295=FACE_OUTER_BOUND('',#6184,.T.);
#4296=FACE_OUTER_BOUND('',#6185,.T.);
#4297=FACE_OUTER_BOUND('',#6186,.T.);
#4298=FACE_OUTER_BOUND('',#6187,.T.);
#4299=FACE_OUTER_BOUND('',#6188,.T.);
#4300=FACE_OUTER_BOUND('',#6189,.T.);
#4301=FACE_OUTER_BOUND('',#6190,.T.);
#4302=FACE_OUTER_BOUND('',#6191,.T.);
#4303=FACE_OUTER_BOUND('',#6192,.T.);
#4304=FACE_OUTER_BOUND('',#6193,.T.);
#4305=FACE_OUTER_BOUND('',#6194,.T.);
#4306=FACE_OUTER_BOUND('',#6195,.T.);
#4307=FACE_OUTER_BOUND('',#6196,.T.);
#4308=FACE_OUTER_BOUND('',#6197,.T.);
#4309=FACE_OUTER_BOUND('',#6198,.T.);
#4310=FACE_OUTER_BOUND('',#6199,.T.);
#4311=FACE_OUTER_BOUND('',#6200,.T.);
#4312=FACE_OUTER_BOUND('',#6201,.T.);
#4313=FACE_OUTER_BOUND('',#6202,.T.);
#4314=FACE_OUTER_BOUND('',#6203,.T.);
#4315=FACE_OUTER_BOUND('',#6204,.T.);
#4316=FACE_OUTER_BOUND('',#6205,.T.);
#4317=FACE_OUTER_BOUND('',#6206,.T.);
#4318=FACE_OUTER_BOUND('',#6207,.T.);
#4319=FACE_OUTER_BOUND('',#6208,.T.);
#4320=FACE_OUTER_BOUND('',#6209,.T.);
#4321=FACE_OUTER_BOUND('',#6210,.T.);
#4322=FACE_OUTER_BOUND('',#6211,.T.);
#4323=FACE_OUTER_BOUND('',#6212,.T.);
#4324=FACE_OUTER_BOUND('',#6213,.T.);
#4325=FACE_OUTER_BOUND('',#6214,.T.);
#4326=FACE_OUTER_BOUND('',#6215,.T.);
#4327=FACE_OUTER_BOUND('',#6216,.T.);
#4328=FACE_OUTER_BOUND('',#6217,.T.);
#4329=FACE_OUTER_BOUND('',#6218,.T.);
#4330=FACE_OUTER_BOUND('',#6219,.T.);
#4331=FACE_OUTER_BOUND('',#6220,.T.);
#4332=FACE_OUTER_BOUND('',#6221,.T.);
#4333=FACE_OUTER_BOUND('',#6222,.T.);
#4334=FACE_OUTER_BOUND('',#6223,.T.);
#4335=FACE_OUTER_BOUND('',#6224,.T.);
#4336=FACE_OUTER_BOUND('',#6225,.T.);
#4337=FACE_OUTER_BOUND('',#6226,.T.);
#4338=FACE_OUTER_BOUND('',#6227,.T.);
#4339=FACE_OUTER_BOUND('',#6228,.T.);
#4340=FACE_OUTER_BOUND('',#6229,.T.);
#4341=FACE_OUTER_BOUND('',#6230,.T.);
#4342=FACE_OUTER_BOUND('',#6231,.T.);
#4343=FACE_OUTER_BOUND('',#6232,.T.);
#4344=FACE_OUTER_BOUND('',#6233,.T.);
#4345=FACE_OUTER_BOUND('',#6234,.T.);
#4346=FACE_OUTER_BOUND('',#6235,.T.);
#4347=FACE_OUTER_BOUND('',#6236,.T.);
#4348=FACE_OUTER_BOUND('',#6237,.T.);
#4349=FACE_OUTER_BOUND('',#6239,.T.);
#4350=FACE_OUTER_BOUND('',#6240,.T.);
#4351=FACE_OUTER_BOUND('',#6241,.T.);
#4352=FACE_OUTER_BOUND('',#6243,.T.);
#4353=FACE_OUTER_BOUND('',#6244,.T.);
#4354=FACE_OUTER_BOUND('',#6246,.T.);
#4355=FACE_OUTER_BOUND('',#6247,.T.);
#4356=FACE_OUTER_BOUND('',#6249,.T.);
#4357=FACE_OUTER_BOUND('',#6250,.T.);
#4358=FACE_OUTER_BOUND('',#6252,.T.);
#4359=FACE_OUTER_BOUND('',#6253,.T.);
#4360=FACE_OUTER_BOUND('',#6255,.T.);
#4361=FACE_OUTER_BOUND('',#6256,.T.);
#4362=FACE_OUTER_BOUND('',#6258,.T.);
#4363=FACE_OUTER_BOUND('',#6259,.T.);
#4364=FACE_OUTER_BOUND('',#6261,.T.);
#4365=FACE_OUTER_BOUND('',#6262,.T.);
#4366=FACE_OUTER_BOUND('',#6263,.T.);
#4367=FACE_OUTER_BOUND('',#6264,.T.);
#4368=FACE_OUTER_BOUND('',#6265,.T.);
#4369=FACE_OUTER_BOUND('',#6266,.T.);
#4370=FACE_OUTER_BOUND('',#6267,.T.);
#4371=FACE_OUTER_BOUND('',#6268,.T.);
#4372=FACE_OUTER_BOUND('',#6269,.T.);
#4373=FACE_OUTER_BOUND('',#6270,.T.);
#4374=FACE_OUTER_BOUND('',#6271,.T.);
#4375=FACE_OUTER_BOUND('',#6273,.T.);
#4376=FACE_OUTER_BOUND('',#6274,.T.);
#4377=FACE_OUTER_BOUND('',#6275,.T.);
#4378=FACE_OUTER_BOUND('',#6276,.T.);
#4379=FACE_OUTER_BOUND('',#6278,.T.);
#4380=FACE_OUTER_BOUND('',#6279,.T.);
#4381=FACE_OUTER_BOUND('',#6280,.T.);
#4382=FACE_OUTER_BOUND('',#6281,.T.);
#4383=FACE_OUTER_BOUND('',#6282,.T.);
#4384=FACE_OUTER_BOUND('',#6283,.T.);
#4385=FACE_OUTER_BOUND('',#6284,.T.);
#4386=FACE_OUTER_BOUND('',#6285,.T.);
#4387=FACE_OUTER_BOUND('',#6286,.T.);
#4388=FACE_OUTER_BOUND('',#6287,.T.);
#4389=FACE_OUTER_BOUND('',#6288,.T.);
#4390=FACE_OUTER_BOUND('',#6290,.T.);
#4391=FACE_OUTER_BOUND('',#6291,.T.);
#4392=FACE_OUTER_BOUND('',#6292,.T.);
#4393=FACE_OUTER_BOUND('',#6293,.T.);
#4394=FACE_OUTER_BOUND('',#6295,.T.);
#4395=FACE_OUTER_BOUND('',#6296,.T.);
#4396=FACE_OUTER_BOUND('',#6297,.T.);
#4397=FACE_OUTER_BOUND('',#6298,.T.);
#4398=FACE_OUTER_BOUND('',#6299,.T.);
#4399=FACE_OUTER_BOUND('',#6300,.T.);
#4400=FACE_OUTER_BOUND('',#6301,.T.);
#4401=FACE_OUTER_BOUND('',#6302,.T.);
#4402=FACE_OUTER_BOUND('',#6303,.T.);
#4403=FACE_OUTER_BOUND('',#6304,.T.);
#4404=FACE_OUTER_BOUND('',#6305,.T.);
#4405=FACE_OUTER_BOUND('',#6307,.T.);
#4406=FACE_OUTER_BOUND('',#6308,.T.);
#4407=FACE_OUTER_BOUND('',#6309,.T.);
#4408=FACE_OUTER_BOUND('',#6310,.T.);
#4409=FACE_OUTER_BOUND('',#6312,.T.);
#4410=FACE_OUTER_BOUND('',#6313,.T.);
#4411=FACE_OUTER_BOUND('',#6314,.T.);
#4412=FACE_OUTER_BOUND('',#6315,.T.);
#4413=FACE_OUTER_BOUND('',#6316,.T.);
#4414=FACE_OUTER_BOUND('',#6317,.T.);
#4415=FACE_OUTER_BOUND('',#6318,.T.);
#4416=FACE_OUTER_BOUND('',#6319,.T.);
#4417=FACE_OUTER_BOUND('',#6320,.T.);
#4418=FACE_OUTER_BOUND('',#6321,.T.);
#4419=FACE_OUTER_BOUND('',#6322,.T.);
#4420=FACE_OUTER_BOUND('',#6324,.T.);
#4421=FACE_OUTER_BOUND('',#6325,.T.);
#4422=FACE_OUTER_BOUND('',#6326,.T.);
#4423=FACE_OUTER_BOUND('',#6327,.T.);
#4424=FACE_OUTER_BOUND('',#6328,.T.);
#4425=FACE_OUTER_BOUND('',#6329,.T.);
#4426=FACE_OUTER_BOUND('',#6330,.T.);
#4427=FACE_OUTER_BOUND('',#6331,.T.);
#4428=FACE_OUTER_BOUND('',#6332,.T.);
#4429=FACE_OUTER_BOUND('',#6333,.T.);
#4430=FACE_OUTER_BOUND('',#6334,.T.);
#4431=FACE_OUTER_BOUND('',#6335,.T.);
#4432=FACE_OUTER_BOUND('',#6337,.T.);
#4433=FACE_OUTER_BOUND('',#6338,.T.);
#4434=FACE_OUTER_BOUND('',#6339,.T.);
#4435=FACE_OUTER_BOUND('',#6340,.T.);
#4436=FACE_OUTER_BOUND('',#6341,.T.);
#4437=FACE_OUTER_BOUND('',#6342,.T.);
#4438=FACE_OUTER_BOUND('',#6343,.T.);
#4439=FACE_OUTER_BOUND('',#6344,.T.);
#4440=FACE_OUTER_BOUND('',#6345,.T.);
#4441=FACE_OUTER_BOUND('',#6346,.T.);
#4442=FACE_OUTER_BOUND('',#6347,.T.);
#4443=FACE_OUTER_BOUND('',#6348,.T.);
#4444=FACE_OUTER_BOUND('',#6349,.T.);
#4445=FACE_OUTER_BOUND('',#6350,.T.);
#4446=FACE_OUTER_BOUND('',#6352,.T.);
#4447=FACE_OUTER_BOUND('',#6353,.T.);
#4448=FACE_OUTER_BOUND('',#6354,.T.);
#4449=FACE_OUTER_BOUND('',#6355,.T.);
#4450=FACE_OUTER_BOUND('',#6356,.T.);
#4451=FACE_OUTER_BOUND('',#6358,.T.);
#4452=FACE_OUTER_BOUND('',#6360,.T.);
#4453=FACE_OUTER_BOUND('',#6361,.T.);
#4454=FACE_OUTER_BOUND('',#6362,.T.);
#4455=FACE_OUTER_BOUND('',#6363,.T.);
#4456=FACE_OUTER_BOUND('',#6364,.T.);
#4457=FACE_OUTER_BOUND('',#6365,.T.);
#4458=FACE_OUTER_BOUND('',#6366,.T.);
#4459=FACE_OUTER_BOUND('',#6374,.T.);
#4460=FACE_OUTER_BOUND('',#6375,.T.);
#4461=FACE_OUTER_BOUND('',#6376,.T.);
#4462=FACE_OUTER_BOUND('',#6377,.T.);
#4463=FACE_OUTER_BOUND('',#6378,.T.);
#4464=FACE_OUTER_BOUND('',#6379,.T.);
#4465=FACE_OUTER_BOUND('',#6380,.T.);
#4466=FACE_OUTER_BOUND('',#6381,.T.);
#4467=FACE_OUTER_BOUND('',#6382,.T.);
#4468=FACE_OUTER_BOUND('',#6383,.T.);
#4469=FACE_OUTER_BOUND('',#6384,.T.);
#4470=FACE_OUTER_BOUND('',#6385,.T.);
#4471=FACE_OUTER_BOUND('',#6386,.T.);
#4472=FACE_OUTER_BOUND('',#6387,.T.);
#4473=FACE_OUTER_BOUND('',#6388,.T.);
#4474=FACE_OUTER_BOUND('',#6396,.T.);
#4475=FACE_OUTER_BOUND('',#6397,.T.);
#4476=FACE_OUTER_BOUND('',#6398,.T.);
#4477=FACE_OUTER_BOUND('',#6400,.T.);
#4478=FACE_OUTER_BOUND('',#6401,.T.);
#4479=FACE_OUTER_BOUND('',#6402,.T.);
#4480=FACE_OUTER_BOUND('',#6403,.T.);
#4481=FACE_OUTER_BOUND('',#6404,.T.);
#4482=FACE_OUTER_BOUND('',#6405,.T.);
#4483=FACE_OUTER_BOUND('',#6406,.T.);
#4484=FACE_OUTER_BOUND('',#6407,.T.);
#4485=FACE_OUTER_BOUND('',#6408,.T.);
#4486=FACE_OUTER_BOUND('',#6411,.T.);
#4487=FACE_OUTER_BOUND('',#6412,.T.);
#4488=FACE_OUTER_BOUND('',#6413,.T.);
#4489=FACE_OUTER_BOUND('',#6414,.T.);
#4490=FACE_OUTER_BOUND('',#6415,.T.);
#4491=FACE_OUTER_BOUND('',#6416,.T.);
#4492=FACE_OUTER_BOUND('',#6417,.T.);
#4493=FACE_OUTER_BOUND('',#6420,.T.);
#4494=FACE_OUTER_BOUND('',#6421,.T.);
#4495=FACE_OUTER_BOUND('',#6423,.T.);
#4496=FACE_OUTER_BOUND('',#6424,.T.);
#4497=FACE_OUTER_BOUND('',#6425,.T.);
#4498=FACE_OUTER_BOUND('',#6426,.T.);
#4499=FACE_OUTER_BOUND('',#6427,.T.);
#4500=FACE_OUTER_BOUND('',#6428,.T.);
#4501=FACE_OUTER_BOUND('',#6429,.T.);
#4502=FACE_OUTER_BOUND('',#6430,.T.);
#4503=FACE_OUTER_BOUND('',#6431,.T.);
#4504=FACE_OUTER_BOUND('',#6432,.T.);
#4505=FACE_OUTER_BOUND('',#6433,.T.);
#4506=FACE_OUTER_BOUND('',#6434,.T.);
#4507=FACE_OUTER_BOUND('',#6435,.T.);
#4508=FACE_OUTER_BOUND('',#6436,.T.);
#4509=FACE_OUTER_BOUND('',#6437,.T.);
#4510=FACE_OUTER_BOUND('',#6438,.T.);
#4511=FACE_OUTER_BOUND('',#6439,.T.);
#4512=FACE_OUTER_BOUND('',#6440,.T.);
#4513=FACE_OUTER_BOUND('',#6441,.T.);
#4514=FACE_OUTER_BOUND('',#6443,.T.);
#4515=FACE_OUTER_BOUND('',#6444,.T.);
#4516=FACE_OUTER_BOUND('',#6445,.T.);
#4517=FACE_OUTER_BOUND('',#6446,.T.);
#4518=FACE_OUTER_BOUND('',#6447,.T.);
#4519=FACE_OUTER_BOUND('',#6448,.T.);
#4520=FACE_OUTER_BOUND('',#6449,.T.);
#4521=FACE_OUTER_BOUND('',#6450,.T.);
#4522=FACE_OUTER_BOUND('',#6451,.T.);
#4523=FACE_OUTER_BOUND('',#6452,.T.);
#4524=FACE_OUTER_BOUND('',#6453,.T.);
#4525=FACE_OUTER_BOUND('',#6455,.T.);
#4526=FACE_OUTER_BOUND('',#6459,.T.);
#4527=FACE_OUTER_BOUND('',#6460,.T.);
#4528=FACE_OUTER_BOUND('',#6461,.T.);
#4529=FACE_OUTER_BOUND('',#6462,.T.);
#4530=FACE_OUTER_BOUND('',#6463,.T.);
#4531=FACE_OUTER_BOUND('',#6464,.T.);
#4532=FACE_OUTER_BOUND('',#6465,.T.);
#4533=FACE_OUTER_BOUND('',#6466,.T.);
#4534=FACE_OUTER_BOUND('',#6467,.T.);
#4535=FACE_OUTER_BOUND('',#6468,.T.);
#4536=FACE_OUTER_BOUND('',#6470,.T.);
#4537=FACE_OUTER_BOUND('',#6471,.T.);
#4538=FACE_OUTER_BOUND('',#6473,.T.);
#4539=FACE_OUTER_BOUND('',#6474,.T.);
#4540=FACE_OUTER_BOUND('',#6475,.T.);
#4541=FACE_OUTER_BOUND('',#6476,.T.);
#4542=FACE_OUTER_BOUND('',#6477,.T.);
#4543=FACE_OUTER_BOUND('',#6478,.T.);
#4544=FACE_OUTER_BOUND('',#6479,.T.);
#4545=FACE_OUTER_BOUND('',#6480,.T.);
#4546=FACE_OUTER_BOUND('',#6481,.T.);
#4547=FACE_OUTER_BOUND('',#6482,.T.);
#4548=FACE_OUTER_BOUND('',#6483,.T.);
#4549=FACE_OUTER_BOUND('',#6484,.T.);
#4550=FACE_OUTER_BOUND('',#6485,.T.);
#4551=FACE_OUTER_BOUND('',#6486,.T.);
#4552=FACE_OUTER_BOUND('',#6487,.T.);
#4553=FACE_OUTER_BOUND('',#6488,.T.);
#4554=FACE_OUTER_BOUND('',#6489,.T.);
#4555=FACE_OUTER_BOUND('',#6490,.T.);
#4556=FACE_OUTER_BOUND('',#6491,.T.);
#4557=FACE_OUTER_BOUND('',#6492,.T.);
#4558=FACE_OUTER_BOUND('',#6493,.T.);
#4559=FACE_OUTER_BOUND('',#6494,.T.);
#4560=FACE_OUTER_BOUND('',#6495,.T.);
#4561=FACE_OUTER_BOUND('',#6496,.T.);
#4562=FACE_OUTER_BOUND('',#6497,.T.);
#4563=FACE_OUTER_BOUND('',#6498,.T.);
#4564=FACE_OUTER_BOUND('',#6499,.T.);
#4565=FACE_OUTER_BOUND('',#6500,.T.);
#4566=FACE_OUTER_BOUND('',#6501,.T.);
#4567=FACE_OUTER_BOUND('',#6502,.T.);
#4568=FACE_OUTER_BOUND('',#6503,.T.);
#4569=FACE_OUTER_BOUND('',#6504,.T.);
#4570=FACE_OUTER_BOUND('',#6505,.T.);
#4571=FACE_OUTER_BOUND('',#6506,.T.);
#4572=FACE_OUTER_BOUND('',#6507,.T.);
#4573=FACE_OUTER_BOUND('',#6508,.T.);
#4574=FACE_OUTER_BOUND('',#6509,.T.);
#4575=FACE_OUTER_BOUND('',#6510,.T.);
#4576=FACE_OUTER_BOUND('',#6511,.T.);
#4577=FACE_OUTER_BOUND('',#6512,.T.);
#4578=FACE_OUTER_BOUND('',#6513,.T.);
#4579=FACE_OUTER_BOUND('',#6514,.T.);
#4580=FACE_OUTER_BOUND('',#6515,.T.);
#4581=FACE_OUTER_BOUND('',#6516,.T.);
#4582=FACE_OUTER_BOUND('',#6517,.T.);
#4583=FACE_OUTER_BOUND('',#6518,.T.);
#4584=FACE_OUTER_BOUND('',#6519,.T.);
#4585=FACE_OUTER_BOUND('',#6520,.T.);
#4586=FACE_OUTER_BOUND('',#6522,.T.);
#4587=FACE_OUTER_BOUND('',#6523,.T.);
#4588=FACE_OUTER_BOUND('',#6524,.T.);
#4589=FACE_OUTER_BOUND('',#6525,.T.);
#4590=FACE_OUTER_BOUND('',#6526,.T.);
#4591=FACE_OUTER_BOUND('',#6527,.T.);
#4592=FACE_OUTER_BOUND('',#6528,.T.);
#4593=FACE_OUTER_BOUND('',#6529,.T.);
#4594=FACE_OUTER_BOUND('',#6530,.T.);
#4595=FACE_OUTER_BOUND('',#6531,.T.);
#4596=FACE_OUTER_BOUND('',#6532,.T.);
#4597=FACE_OUTER_BOUND('',#6533,.T.);
#4598=FACE_OUTER_BOUND('',#6534,.T.);
#4599=FACE_OUTER_BOUND('',#6535,.T.);
#4600=FACE_OUTER_BOUND('',#6536,.T.);
#4601=FACE_OUTER_BOUND('',#6537,.T.);
#4602=FACE_OUTER_BOUND('',#6538,.T.);
#4603=FACE_OUTER_BOUND('',#6540,.T.);
#4604=FACE_OUTER_BOUND('',#6541,.T.);
#4605=FACE_OUTER_BOUND('',#6542,.T.);
#4606=FACE_OUTER_BOUND('',#6543,.T.);
#4607=FACE_OUTER_BOUND('',#6544,.T.);
#4608=FACE_OUTER_BOUND('',#6545,.T.);
#4609=FACE_OUTER_BOUND('',#6546,.T.);
#4610=FACE_OUTER_BOUND('',#6547,.T.);
#4611=FACE_OUTER_BOUND('',#6548,.T.);
#4612=FACE_OUTER_BOUND('',#6549,.T.);
#4613=FACE_OUTER_BOUND('',#6550,.T.);
#4614=FACE_OUTER_BOUND('',#6551,.T.);
#4615=FACE_OUTER_BOUND('',#6553,.T.);
#4616=FACE_OUTER_BOUND('',#6554,.T.);
#4617=FACE_OUTER_BOUND('',#6555,.T.);
#4618=FACE_OUTER_BOUND('',#6556,.T.);
#4619=FACE_OUTER_BOUND('',#6557,.T.);
#4620=FACE_OUTER_BOUND('',#6558,.T.);
#4621=FACE_OUTER_BOUND('',#6559,.T.);
#4622=FACE_OUTER_BOUND('',#6560,.T.);
#4623=FACE_OUTER_BOUND('',#6561,.T.);
#4624=FACE_OUTER_BOUND('',#6562,.T.);
#4625=FACE_OUTER_BOUND('',#6563,.T.);
#4626=FACE_OUTER_BOUND('',#6567,.T.);
#4627=FACE_OUTER_BOUND('',#6568,.T.);
#4628=FACE_OUTER_BOUND('',#6569,.T.);
#4629=FACE_OUTER_BOUND('',#6571,.T.);
#4630=FACE_OUTER_BOUND('',#6572,.T.);
#4631=FACE_OUTER_BOUND('',#6573,.T.);
#4632=FACE_OUTER_BOUND('',#6574,.T.);
#4633=FACE_OUTER_BOUND('',#6575,.T.);
#4634=FACE_OUTER_BOUND('',#6576,.T.);
#4635=FACE_OUTER_BOUND('',#6578,.T.);
#4636=FACE_OUTER_BOUND('',#6579,.T.);
#4637=FACE_OUTER_BOUND('',#6580,.T.);
#4638=FACE_OUTER_BOUND('',#6581,.T.);
#4639=FACE_OUTER_BOUND('',#6582,.T.);
#4640=FACE_OUTER_BOUND('',#6584,.T.);
#4641=FACE_OUTER_BOUND('',#6585,.T.);
#4642=FACE_OUTER_BOUND('',#6586,.T.);
#4643=FACE_OUTER_BOUND('',#6587,.T.);
#4644=FACE_OUTER_BOUND('',#6588,.T.);
#4645=FACE_OUTER_BOUND('',#6589,.T.);
#4646=FACE_OUTER_BOUND('',#6590,.T.);
#4647=FACE_OUTER_BOUND('',#6591,.T.);
#4648=FACE_OUTER_BOUND('',#6592,.T.);
#4649=FACE_OUTER_BOUND('',#6593,.T.);
#4650=FACE_OUTER_BOUND('',#6594,.T.);
#4651=FACE_OUTER_BOUND('',#6595,.T.);
#4652=FACE_OUTER_BOUND('',#6596,.T.);
#4653=FACE_OUTER_BOUND('',#6597,.T.);
#4654=FACE_OUTER_BOUND('',#6598,.T.);
#4655=FACE_OUTER_BOUND('',#6599,.T.);
#4656=FACE_OUTER_BOUND('',#6600,.T.);
#4657=FACE_OUTER_BOUND('',#6601,.T.);
#4658=FACE_OUTER_BOUND('',#6611,.T.);
#4659=FACE_OUTER_BOUND('',#6612,.T.);
#4660=FACE_OUTER_BOUND('',#6614,.T.);
#4661=FACE_OUTER_BOUND('',#6615,.T.);
#4662=FACE_OUTER_BOUND('',#6619,.T.);
#4663=FACE_OUTER_BOUND('',#6620,.T.);
#4664=FACE_OUTER_BOUND('',#6622,.T.);
#4665=FACE_OUTER_BOUND('',#6623,.T.);
#4666=FACE_OUTER_BOUND('',#6625,.T.);
#4667=FACE_OUTER_BOUND('',#6626,.T.);
#4668=FACE_OUTER_BOUND('',#6627,.T.);
#4669=FACE_OUTER_BOUND('',#6628,.T.);
#4670=FACE_OUTER_BOUND('',#6629,.T.);
#4671=FACE_OUTER_BOUND('',#6631,.T.);
#4672=FACE_OUTER_BOUND('',#6632,.T.);
#4673=FACE_OUTER_BOUND('',#6633,.T.);
#4674=FACE_OUTER_BOUND('',#6634,.T.);
#4675=FACE_OUTER_BOUND('',#6635,.T.);
#4676=FACE_OUTER_BOUND('',#6637,.T.);
#4677=FACE_OUTER_BOUND('',#6638,.T.);
#4678=FACE_OUTER_BOUND('',#6639,.T.);
#4679=FACE_OUTER_BOUND('',#6641,.T.);
#4680=FACE_OUTER_BOUND('',#6642,.T.);
#4681=FACE_OUTER_BOUND('',#6643,.T.);
#4682=FACE_OUTER_BOUND('',#6644,.T.);
#4683=FACE_OUTER_BOUND('',#6645,.T.);
#4684=FACE_OUTER_BOUND('',#6646,.T.);
#4685=FACE_OUTER_BOUND('',#6648,.T.);
#4686=FACE_OUTER_BOUND('',#6649,.T.);
#4687=FACE_OUTER_BOUND('',#6650,.T.);
#4688=FACE_OUTER_BOUND('',#6651,.T.);
#4689=FACE_OUTER_BOUND('',#6653,.T.);
#4690=FACE_OUTER_BOUND('',#6654,.T.);
#4691=FACE_OUTER_BOUND('',#6655,.T.);
#4692=FACE_OUTER_BOUND('',#6657,.T.);
#4693=FACE_OUTER_BOUND('',#6659,.T.);
#4694=FACE_OUTER_BOUND('',#6661,.T.);
#4695=FACE_OUTER_BOUND('',#6662,.T.);
#4696=FACE_OUTER_BOUND('',#6663,.T.);
#4697=FACE_OUTER_BOUND('',#6665,.T.);
#4698=FACE_OUTER_BOUND('',#6666,.T.);
#4699=FACE_OUTER_BOUND('',#6667,.T.);
#4700=FACE_OUTER_BOUND('',#6668,.T.);
#4701=FACE_OUTER_BOUND('',#6669,.T.);
#4702=FACE_OUTER_BOUND('',#6670,.T.);
#4703=FACE_OUTER_BOUND('',#6671,.T.);
#4704=FACE_OUTER_BOUND('',#6672,.T.);
#4705=FACE_OUTER_BOUND('',#6673,.T.);
#4706=FACE_OUTER_BOUND('',#6674,.T.);
#4707=FACE_OUTER_BOUND('',#6675,.T.);
#4708=FACE_OUTER_BOUND('',#6676,.T.);
#4709=FACE_OUTER_BOUND('',#6677,.T.);
#4710=FACE_OUTER_BOUND('',#6678,.T.);
#4711=FACE_OUTER_BOUND('',#6679,.T.);
#4712=FACE_OUTER_BOUND('',#6680,.T.);
#4713=FACE_OUTER_BOUND('',#6681,.T.);
#4714=FACE_OUTER_BOUND('',#6682,.T.);
#4715=FACE_OUTER_BOUND('',#6683,.T.);
#4716=FACE_OUTER_BOUND('',#6684,.T.);
#4717=FACE_OUTER_BOUND('',#6685,.T.);
#4718=FACE_OUTER_BOUND('',#6686,.T.);
#4719=FACE_OUTER_BOUND('',#6687,.T.);
#4720=FACE_OUTER_BOUND('',#6688,.T.);
#4721=FACE_OUTER_BOUND('',#6689,.T.);
#4722=FACE_OUTER_BOUND('',#6690,.T.);
#4723=FACE_OUTER_BOUND('',#6691,.T.);
#4724=FACE_OUTER_BOUND('',#6692,.T.);
#4725=FACE_OUTER_BOUND('',#6693,.T.);
#4726=FACE_OUTER_BOUND('',#6694,.T.);
#4727=FACE_OUTER_BOUND('',#6695,.T.);
#4728=FACE_OUTER_BOUND('',#6696,.T.);
#4729=FACE_OUTER_BOUND('',#6697,.T.);
#4730=FACE_OUTER_BOUND('',#6703,.T.);
#4731=FACE_OUTER_BOUND('',#6704,.T.);
#4732=FACE_OUTER_BOUND('',#6705,.T.);
#4733=FACE_OUTER_BOUND('',#6706,.T.);
#4734=FACE_OUTER_BOUND('',#6707,.T.);
#4735=FACE_OUTER_BOUND('',#6708,.T.);
#4736=FACE_OUTER_BOUND('',#6709,.T.);
#4737=FACE_OUTER_BOUND('',#6710,.T.);
#4738=FACE_OUTER_BOUND('',#6711,.T.);
#4739=FACE_OUTER_BOUND('',#6712,.T.);
#4740=FACE_OUTER_BOUND('',#6713,.T.);
#4741=FACE_OUTER_BOUND('',#6714,.T.);
#4742=FACE_OUTER_BOUND('',#6715,.T.);
#4743=FACE_OUTER_BOUND('',#6716,.T.);
#4744=FACE_OUTER_BOUND('',#6717,.T.);
#4745=FACE_OUTER_BOUND('',#6718,.T.);
#4746=FACE_OUTER_BOUND('',#6719,.T.);
#4747=FACE_OUTER_BOUND('',#6720,.T.);
#4748=FACE_OUTER_BOUND('',#6721,.T.);
#4749=FACE_OUTER_BOUND('',#6722,.T.);
#4750=FACE_OUTER_BOUND('',#6723,.T.);
#4751=FACE_OUTER_BOUND('',#6724,.T.);
#4752=FACE_OUTER_BOUND('',#6725,.T.);
#4753=FACE_OUTER_BOUND('',#6726,.T.);
#4754=FACE_OUTER_BOUND('',#6727,.T.);
#4755=FACE_OUTER_BOUND('',#6728,.T.);
#4756=FACE_OUTER_BOUND('',#6729,.T.);
#4757=FACE_OUTER_BOUND('',#6730,.T.);
#4758=FACE_OUTER_BOUND('',#6731,.T.);
#4759=FACE_OUTER_BOUND('',#6732,.T.);
#4760=FACE_OUTER_BOUND('',#6733,.T.);
#4761=FACE_OUTER_BOUND('',#6734,.T.);
#4762=FACE_OUTER_BOUND('',#6735,.T.);
#4763=FACE_OUTER_BOUND('',#6736,.T.);
#4764=FACE_OUTER_BOUND('',#6737,.T.);
#4765=FACE_OUTER_BOUND('',#6738,.T.);
#4766=FACE_OUTER_BOUND('',#6739,.T.);
#4767=FACE_OUTER_BOUND('',#6740,.T.);
#4768=FACE_OUTER_BOUND('',#6741,.T.);
#4769=FACE_OUTER_BOUND('',#6742,.T.);
#4770=FACE_OUTER_BOUND('',#6743,.T.);
#4771=FACE_OUTER_BOUND('',#6744,.T.);
#4772=FACE_OUTER_BOUND('',#6745,.T.);
#4773=FACE_OUTER_BOUND('',#6746,.T.);
#4774=FACE_OUTER_BOUND('',#6747,.T.);
#4775=FACE_OUTER_BOUND('',#6753,.T.);
#4776=FACE_OUTER_BOUND('',#6754,.T.);
#4777=FACE_OUTER_BOUND('',#6755,.T.);
#4778=FACE_OUTER_BOUND('',#6756,.T.);
#4779=FACE_OUTER_BOUND('',#6757,.T.);
#4780=FACE_OUTER_BOUND('',#6758,.T.);
#4781=FACE_OUTER_BOUND('',#6759,.T.);
#4782=FACE_OUTER_BOUND('',#6760,.T.);
#4783=FACE_OUTER_BOUND('',#6761,.T.);
#4784=FACE_OUTER_BOUND('',#6762,.T.);
#4785=FACE_OUTER_BOUND('',#6763,.T.);
#4786=FACE_OUTER_BOUND('',#6764,.T.);
#4787=FACE_OUTER_BOUND('',#6765,.T.);
#4788=FACE_OUTER_BOUND('',#6766,.T.);
#4789=FACE_OUTER_BOUND('',#6767,.T.);
#4790=FACE_OUTER_BOUND('',#6768,.T.);
#4791=FACE_OUTER_BOUND('',#6769,.T.);
#4792=FACE_OUTER_BOUND('',#6770,.T.);
#4793=FACE_OUTER_BOUND('',#6771,.T.);
#4794=FACE_OUTER_BOUND('',#6772,.T.);
#4795=FACE_OUTER_BOUND('',#6773,.T.);
#4796=FACE_OUTER_BOUND('',#6774,.T.);
#4797=FACE_OUTER_BOUND('',#6775,.T.);
#4798=FACE_OUTER_BOUND('',#6776,.T.);
#4799=FACE_OUTER_BOUND('',#6777,.T.);
#4800=FACE_OUTER_BOUND('',#6778,.T.);
#4801=FACE_OUTER_BOUND('',#6779,.T.);
#4802=FACE_OUTER_BOUND('',#6780,.T.);
#4803=FACE_OUTER_BOUND('',#6781,.T.);
#4804=FACE_OUTER_BOUND('',#6782,.T.);
#4805=FACE_OUTER_BOUND('',#6783,.T.);
#4806=FACE_OUTER_BOUND('',#6784,.T.);
#4807=FACE_OUTER_BOUND('',#6785,.T.);
#4808=FACE_OUTER_BOUND('',#6786,.T.);
#4809=FACE_OUTER_BOUND('',#6787,.T.);
#4810=FACE_OUTER_BOUND('',#6788,.T.);
#4811=FACE_OUTER_BOUND('',#6789,.T.);
#4812=FACE_OUTER_BOUND('',#6790,.T.);
#4813=FACE_OUTER_BOUND('',#6791,.T.);
#4814=FACE_OUTER_BOUND('',#6792,.T.);
#4815=FACE_OUTER_BOUND('',#6793,.T.);
#4816=FACE_OUTER_BOUND('',#6794,.T.);
#4817=FACE_OUTER_BOUND('',#6795,.T.);
#4818=FACE_OUTER_BOUND('',#6796,.T.);
#4819=FACE_OUTER_BOUND('',#6797,.T.);
#4820=FACE_OUTER_BOUND('',#6798,.T.);
#4821=FACE_OUTER_BOUND('',#6799,.T.);
#4822=FACE_OUTER_BOUND('',#6800,.T.);
#4823=FACE_OUTER_BOUND('',#6802,.T.);
#4824=FACE_OUTER_BOUND('',#6804,.T.);
#4825=FACE_OUTER_BOUND('',#6805,.T.);
#4826=FACE_OUTER_BOUND('',#6806,.T.);
#4827=FACE_OUTER_BOUND('',#6807,.T.);
#4828=FACE_OUTER_BOUND('',#6808,.T.);
#4829=FACE_OUTER_BOUND('',#6809,.T.);
#4830=FACE_OUTER_BOUND('',#6810,.T.);
#4831=FACE_OUTER_BOUND('',#6811,.T.);
#4832=FACE_OUTER_BOUND('',#6812,.T.);
#4833=FACE_OUTER_BOUND('',#6813,.T.);
#4834=FACE_OUTER_BOUND('',#6814,.T.);
#4835=FACE_OUTER_BOUND('',#6815,.T.);
#4836=FACE_OUTER_BOUND('',#6816,.T.);
#4837=FACE_OUTER_BOUND('',#6817,.T.);
#4838=FACE_OUTER_BOUND('',#6818,.T.);
#4839=FACE_OUTER_BOUND('',#6819,.T.);
#4840=FACE_OUTER_BOUND('',#6820,.T.);
#4841=FACE_OUTER_BOUND('',#6822,.T.);
#4842=FACE_OUTER_BOUND('',#6824,.T.);
#4843=FACE_OUTER_BOUND('',#6825,.T.);
#4844=FACE_OUTER_BOUND('',#6826,.T.);
#4845=FACE_OUTER_BOUND('',#6827,.T.);
#4846=FACE_OUTER_BOUND('',#6828,.T.);
#4847=FACE_OUTER_BOUND('',#6829,.T.);
#4848=FACE_OUTER_BOUND('',#6830,.T.);
#4849=FACE_OUTER_BOUND('',#6831,.T.);
#4850=FACE_OUTER_BOUND('',#6832,.T.);
#4851=FACE_OUTER_BOUND('',#6833,.T.);
#4852=FACE_OUTER_BOUND('',#6834,.T.);
#4853=FACE_OUTER_BOUND('',#6835,.T.);
#4854=FACE_OUTER_BOUND('',#6836,.T.);
#4855=FACE_OUTER_BOUND('',#6837,.T.);
#4856=FACE_OUTER_BOUND('',#6838,.T.);
#4857=FACE_OUTER_BOUND('',#6839,.T.);
#4858=FACE_OUTER_BOUND('',#6840,.T.);
#4859=FACE_OUTER_BOUND('',#6842,.T.);
#4860=FACE_OUTER_BOUND('',#6844,.T.);
#4861=FACE_OUTER_BOUND('',#6845,.T.);
#4862=FACE_OUTER_BOUND('',#6846,.T.);
#4863=FACE_OUTER_BOUND('',#6847,.T.);
#4864=FACE_OUTER_BOUND('',#6848,.T.);
#4865=FACE_OUTER_BOUND('',#6849,.T.);
#4866=FACE_OUTER_BOUND('',#6850,.T.);
#4867=FACE_OUTER_BOUND('',#6851,.T.);
#4868=FACE_OUTER_BOUND('',#6852,.T.);
#4869=FACE_OUTER_BOUND('',#6853,.T.);
#4870=FACE_OUTER_BOUND('',#6854,.T.);
#4871=FACE_OUTER_BOUND('',#6855,.T.);
#4872=FACE_OUTER_BOUND('',#6856,.T.);
#4873=FACE_OUTER_BOUND('',#6857,.T.);
#4874=FACE_OUTER_BOUND('',#6858,.T.);
#4875=FACE_OUTER_BOUND('',#6859,.T.);
#4876=FACE_OUTER_BOUND('',#6860,.T.);
#4877=FACE_OUTER_BOUND('',#6862,.T.);
#4878=FACE_OUTER_BOUND('',#6864,.T.);
#4879=FACE_OUTER_BOUND('',#6866,.T.);
#4880=FACE_OUTER_BOUND('',#6867,.T.);
#4881=FACE_OUTER_BOUND('',#6868,.T.);
#4882=FACE_OUTER_BOUND('',#6869,.T.);
#4883=FACE_OUTER_BOUND('',#6870,.T.);
#4884=FACE_OUTER_BOUND('',#6871,.T.);
#4885=FACE_OUTER_BOUND('',#6872,.T.);
#4886=FACE_OUTER_BOUND('',#6873,.T.);
#4887=FACE_OUTER_BOUND('',#6875,.T.);
#4888=FACE_OUTER_BOUND('',#6876,.T.);
#4889=FACE_OUTER_BOUND('',#6877,.T.);
#4890=FACE_OUTER_BOUND('',#6878,.T.);
#4891=FACE_OUTER_BOUND('',#6879,.T.);
#4892=FACE_OUTER_BOUND('',#6880,.T.);
#4893=FACE_OUTER_BOUND('',#6881,.T.);
#4894=FACE_OUTER_BOUND('',#6882,.T.);
#4895=FACE_OUTER_BOUND('',#6883,.T.);
#4896=FACE_OUTER_BOUND('',#6884,.T.);
#4897=FACE_OUTER_BOUND('',#6886,.T.);
#4898=FACE_OUTER_BOUND('',#6887,.T.);
#4899=FACE_OUTER_BOUND('',#6888,.T.);
#4900=FACE_OUTER_BOUND('',#6889,.T.);
#4901=FACE_OUTER_BOUND('',#6890,.T.);
#4902=FACE_OUTER_BOUND('',#6891,.T.);
#4903=FACE_OUTER_BOUND('',#6892,.T.);
#4904=FACE_OUTER_BOUND('',#6893,.T.);
#4905=FACE_OUTER_BOUND('',#6894,.T.);
#4906=FACE_OUTER_BOUND('',#6896,.T.);
#4907=FACE_OUTER_BOUND('',#6897,.T.);
#4908=FACE_OUTER_BOUND('',#6898,.T.);
#4909=FACE_OUTER_BOUND('',#6899,.T.);
#4910=FACE_OUTER_BOUND('',#6900,.T.);
#4911=FACE_OUTER_BOUND('',#6901,.T.);
#4912=FACE_OUTER_BOUND('',#6902,.T.);
#4913=FACE_OUTER_BOUND('',#6903,.T.);
#4914=FACE_OUTER_BOUND('',#6904,.T.);
#4915=FACE_OUTER_BOUND('',#6906,.T.);
#4916=FACE_OUTER_BOUND('',#6907,.T.);
#4917=FACE_OUTER_BOUND('',#6908,.T.);
#4918=FACE_OUTER_BOUND('',#6909,.T.);
#4919=FACE_OUTER_BOUND('',#6910,.T.);
#4920=FACE_OUTER_BOUND('',#6911,.T.);
#4921=FACE_OUTER_BOUND('',#6912,.T.);
#4922=FACE_OUTER_BOUND('',#6913,.T.);
#4923=FACE_OUTER_BOUND('',#6914,.T.);
#4924=FACE_OUTER_BOUND('',#6916,.T.);
#4925=FACE_OUTER_BOUND('',#6917,.T.);
#4926=FACE_OUTER_BOUND('',#6918,.T.);
#4927=FACE_OUTER_BOUND('',#6919,.T.);
#4928=FACE_OUTER_BOUND('',#6920,.T.);
#4929=FACE_OUTER_BOUND('',#6921,.T.);
#4930=FACE_OUTER_BOUND('',#6922,.T.);
#4931=FACE_OUTER_BOUND('',#6923,.T.);
#4932=FACE_OUTER_BOUND('',#6924,.T.);
#4933=FACE_OUTER_BOUND('',#6926,.T.);
#4934=FACE_OUTER_BOUND('',#6927,.T.);
#4935=FACE_OUTER_BOUND('',#6928,.T.);
#4936=FACE_OUTER_BOUND('',#6929,.T.);
#4937=FACE_OUTER_BOUND('',#6930,.T.);
#4938=FACE_OUTER_BOUND('',#6931,.T.);
#4939=FACE_OUTER_BOUND('',#6932,.T.);
#4940=FACE_OUTER_BOUND('',#6933,.T.);
#4941=FACE_OUTER_BOUND('',#6934,.T.);
#4942=FACE_OUTER_BOUND('',#6936,.T.);
#4943=FACE_OUTER_BOUND('',#6937,.T.);
#4944=FACE_OUTER_BOUND('',#6938,.T.);
#4945=FACE_OUTER_BOUND('',#6939,.T.);
#4946=FACE_OUTER_BOUND('',#6940,.T.);
#4947=FACE_OUTER_BOUND('',#6941,.T.);
#4948=FACE_OUTER_BOUND('',#6942,.T.);
#4949=FACE_OUTER_BOUND('',#6943,.T.);
#4950=FACE_OUTER_BOUND('',#6944,.T.);
#4951=FACE_OUTER_BOUND('',#6945,.T.);
#4952=FACE_OUTER_BOUND('',#6946,.T.);
#4953=FACE_OUTER_BOUND('',#6947,.T.);
#4954=FACE_OUTER_BOUND('',#6948,.T.);
#4955=FACE_OUTER_BOUND('',#6949,.T.);
#4956=FACE_OUTER_BOUND('',#6950,.T.);
#4957=FACE_OUTER_BOUND('',#6951,.T.);
#4958=FACE_OUTER_BOUND('',#6952,.T.);
#4959=FACE_OUTER_BOUND('',#6953,.T.);
#4960=FACE_OUTER_BOUND('',#6954,.T.);
#4961=FACE_OUTER_BOUND('',#6955,.T.);
#4962=FACE_OUTER_BOUND('',#6956,.T.);
#4963=FACE_OUTER_BOUND('',#6957,.T.);
#4964=FACE_OUTER_BOUND('',#6958,.T.);
#4965=FACE_OUTER_BOUND('',#6959,.T.);
#4966=FACE_OUTER_BOUND('',#6960,.T.);
#4967=FACE_OUTER_BOUND('',#6962,.T.);
#4968=FACE_OUTER_BOUND('',#6964,.T.);
#4969=FACE_OUTER_BOUND('',#6965,.T.);
#4970=FACE_OUTER_BOUND('',#6966,.T.);
#4971=FACE_OUTER_BOUND('',#6967,.T.);
#4972=FACE_OUTER_BOUND('',#6968,.T.);
#4973=FACE_OUTER_BOUND('',#6969,.T.);
#4974=FACE_OUTER_BOUND('',#6970,.T.);
#4975=FACE_OUTER_BOUND('',#6971,.T.);
#4976=FACE_OUTER_BOUND('',#6972,.T.);
#4977=FACE_OUTER_BOUND('',#6973,.T.);
#4978=FACE_OUTER_BOUND('',#6974,.T.);
#4979=FACE_OUTER_BOUND('',#6975,.T.);
#4980=FACE_OUTER_BOUND('',#6976,.T.);
#4981=FACE_OUTER_BOUND('',#6977,.T.);
#4982=FACE_OUTER_BOUND('',#6978,.T.);
#4983=FACE_OUTER_BOUND('',#6979,.T.);
#4984=FACE_OUTER_BOUND('',#6980,.T.);
#4985=FACE_OUTER_BOUND('',#6982,.T.);
#4986=FACE_OUTER_BOUND('',#6984,.T.);
#4987=FACE_OUTER_BOUND('',#6985,.T.);
#4988=FACE_OUTER_BOUND('',#6986,.T.);
#4989=FACE_OUTER_BOUND('',#6987,.T.);
#4990=FACE_OUTER_BOUND('',#6988,.T.);
#4991=FACE_OUTER_BOUND('',#6989,.T.);
#4992=FACE_OUTER_BOUND('',#6990,.T.);
#4993=FACE_OUTER_BOUND('',#6991,.T.);
#4994=FACE_OUTER_BOUND('',#6992,.T.);
#4995=FACE_OUTER_BOUND('',#6993,.T.);
#4996=FACE_OUTER_BOUND('',#6994,.T.);
#4997=FACE_OUTER_BOUND('',#6995,.T.);
#4998=FACE_OUTER_BOUND('',#6996,.T.);
#4999=FACE_OUTER_BOUND('',#6997,.T.);
#5000=FACE_OUTER_BOUND('',#6998,.T.);
#5001=FACE_OUTER_BOUND('',#6999,.T.);
#5002=FACE_OUTER_BOUND('',#7000,.T.);
#5003=FACE_OUTER_BOUND('',#7002,.T.);
#5004=FACE_OUTER_BOUND('',#7004,.T.);
#5005=FACE_OUTER_BOUND('',#7005,.T.);
#5006=FACE_OUTER_BOUND('',#7006,.T.);
#5007=FACE_OUTER_BOUND('',#7007,.T.);
#5008=FACE_OUTER_BOUND('',#7008,.T.);
#5009=FACE_OUTER_BOUND('',#7009,.T.);
#5010=FACE_OUTER_BOUND('',#7010,.T.);
#5011=FACE_OUTER_BOUND('',#7011,.T.);
#5012=FACE_OUTER_BOUND('',#7012,.T.);
#5013=FACE_OUTER_BOUND('',#7013,.T.);
#5014=FACE_OUTER_BOUND('',#7014,.T.);
#5015=FACE_OUTER_BOUND('',#7015,.T.);
#5016=FACE_OUTER_BOUND('',#7016,.T.);
#5017=FACE_OUTER_BOUND('',#7017,.T.);
#5018=FACE_OUTER_BOUND('',#7018,.T.);
#5019=FACE_OUTER_BOUND('',#7019,.T.);
#5020=FACE_OUTER_BOUND('',#7020,.T.);
#5021=FACE_OUTER_BOUND('',#7022,.T.);
#5022=FACE_OUTER_BOUND('',#7024,.T.);
#5023=FACE_OUTER_BOUND('',#7025,.T.);
#5024=FACE_OUTER_BOUND('',#7026,.T.);
#5025=FACE_OUTER_BOUND('',#7027,.T.);
#5026=FACE_OUTER_BOUND('',#7028,.T.);
#5027=FACE_OUTER_BOUND('',#7029,.T.);
#5028=FACE_OUTER_BOUND('',#7030,.T.);
#5029=FACE_OUTER_BOUND('',#7031,.T.);
#5030=FACE_OUTER_BOUND('',#7032,.T.);
#5031=FACE_OUTER_BOUND('',#7033,.T.);
#5032=FACE_OUTER_BOUND('',#7034,.T.);
#5033=FACE_OUTER_BOUND('',#7035,.T.);
#5034=FACE_OUTER_BOUND('',#7036,.T.);
#5035=FACE_OUTER_BOUND('',#7037,.T.);
#5036=FACE_OUTER_BOUND('',#7038,.T.);
#5037=FACE_OUTER_BOUND('',#7039,.T.);
#5038=FACE_OUTER_BOUND('',#7040,.T.);
#5039=FACE_OUTER_BOUND('',#7042,.T.);
#5040=FACE_OUTER_BOUND('',#7044,.T.);
#5041=FACE_OUTER_BOUND('',#7045,.T.);
#5042=FACE_OUTER_BOUND('',#7046,.T.);
#5043=FACE_OUTER_BOUND('',#7047,.T.);
#5044=FACE_OUTER_BOUND('',#7048,.T.);
#5045=FACE_OUTER_BOUND('',#7049,.T.);
#5046=FACE_OUTER_BOUND('',#7050,.T.);
#5047=FACE_OUTER_BOUND('',#7051,.T.);
#5048=FACE_OUTER_BOUND('',#7052,.T.);
#5049=FACE_OUTER_BOUND('',#7053,.T.);
#5050=FACE_OUTER_BOUND('',#7054,.T.);
#5051=FACE_OUTER_BOUND('',#7055,.T.);
#5052=FACE_OUTER_BOUND('',#7056,.T.);
#5053=FACE_OUTER_BOUND('',#7057,.T.);
#5054=FACE_OUTER_BOUND('',#7058,.T.);
#5055=FACE_OUTER_BOUND('',#7059,.T.);
#5056=FACE_OUTER_BOUND('',#7060,.T.);
#5057=FACE_OUTER_BOUND('',#7062,.T.);
#5058=FACE_OUTER_BOUND('',#7064,.T.);
#5059=FACE_OUTER_BOUND('',#7065,.T.);
#5060=FACE_OUTER_BOUND('',#7066,.T.);
#5061=FACE_OUTER_BOUND('',#7067,.T.);
#5062=FACE_OUTER_BOUND('',#7068,.T.);
#5063=FACE_OUTER_BOUND('',#7069,.T.);
#5064=FACE_OUTER_BOUND('',#7070,.T.);
#5065=FACE_OUTER_BOUND('',#7071,.T.);
#5066=FACE_OUTER_BOUND('',#7072,.T.);
#5067=FACE_OUTER_BOUND('',#7073,.T.);
#5068=FACE_OUTER_BOUND('',#7074,.T.);
#5069=FACE_OUTER_BOUND('',#7075,.T.);
#5070=FACE_OUTER_BOUND('',#7076,.T.);
#5071=FACE_OUTER_BOUND('',#7077,.T.);
#5072=FACE_OUTER_BOUND('',#7078,.T.);
#5073=FACE_OUTER_BOUND('',#7079,.T.);
#5074=FACE_OUTER_BOUND('',#7080,.T.);
#5075=FACE_OUTER_BOUND('',#7082,.T.);
#5076=FACE_OUTER_BOUND('',#7084,.T.);
#5077=FACE_OUTER_BOUND('',#7085,.T.);
#5078=FACE_OUTER_BOUND('',#7086,.T.);
#5079=FACE_OUTER_BOUND('',#7087,.T.);
#5080=FACE_OUTER_BOUND('',#7088,.T.);
#5081=FACE_OUTER_BOUND('',#7089,.T.);
#5082=FACE_OUTER_BOUND('',#7090,.T.);
#5083=FACE_OUTER_BOUND('',#7091,.T.);
#5084=FACE_OUTER_BOUND('',#7092,.T.);
#5085=FACE_OUTER_BOUND('',#7093,.T.);
#5086=FACE_OUTER_BOUND('',#7094,.T.);
#5087=FACE_OUTER_BOUND('',#7095,.T.);
#5088=FACE_OUTER_BOUND('',#7096,.T.);
#5089=FACE_OUTER_BOUND('',#7097,.T.);
#5090=FACE_OUTER_BOUND('',#7098,.T.);
#5091=FACE_OUTER_BOUND('',#7099,.T.);
#5092=FACE_OUTER_BOUND('',#7100,.T.);
#5093=FACE_OUTER_BOUND('',#7109,.T.);
#5094=FACE_OUTER_BOUND('',#7110,.T.);
#5095=FACE_OUTER_BOUND('',#7119,.T.);
#5096=FACE_OUTER_BOUND('',#7120,.T.);
#5097=FACE_OUTER_BOUND('',#7122,.T.);
#5098=FACE_OUTER_BOUND('',#7131,.T.);
#5099=FACE_OUTER_BOUND('',#7132,.T.);
#5100=FACE_OUTER_BOUND('',#7141,.T.);
#5101=FACE_OUTER_BOUND('',#7142,.T.);
#5102=FACE_OUTER_BOUND('',#7144,.T.);
#5103=FACE_OUTER_BOUND('',#7148,.T.);
#5104=FACE_OUTER_BOUND('',#7152,.T.);
#5105=FACE_OUTER_BOUND('',#7153,.T.);
#5106=FACE_OUTER_BOUND('',#7154,.T.);
#5107=FACE_OUTER_BOUND('',#7155,.T.);
#5108=FACE_OUTER_BOUND('',#7156,.T.);
#5109=FACE_OUTER_BOUND('',#7157,.T.);
#5110=FACE_OUTER_BOUND('',#7158,.T.);
#5111=FACE_OUTER_BOUND('',#7159,.T.);
#5112=FACE_OUTER_BOUND('',#7160,.T.);
#5113=FACE_OUTER_BOUND('',#7161,.T.);
#5114=FACE_OUTER_BOUND('',#7162,.T.);
#5115=FACE_OUTER_BOUND('',#7163,.T.);
#5116=FACE_OUTER_BOUND('',#7164,.T.);
#5117=FACE_OUTER_BOUND('',#7165,.T.);
#5118=FACE_OUTER_BOUND('',#7166,.T.);
#5119=FACE_OUTER_BOUND('',#7167,.T.);
#5120=FACE_OUTER_BOUND('',#7168,.T.);
#5121=FACE_OUTER_BOUND('',#7169,.T.);
#5122=FACE_OUTER_BOUND('',#7170,.T.);
#5123=FACE_OUTER_BOUND('',#7171,.T.);
#5124=FACE_OUTER_BOUND('',#7172,.T.);
#5125=FACE_OUTER_BOUND('',#7173,.T.);
#5126=FACE_OUTER_BOUND('',#7174,.T.);
#5127=FACE_OUTER_BOUND('',#7175,.T.);
#5128=FACE_OUTER_BOUND('',#7186,.T.);
#5129=FACE_OUTER_BOUND('',#7187,.T.);
#5130=FACE_OUTER_BOUND('',#7198,.T.);
#5131=FACE_OUTER_BOUND('',#7202,.T.);
#5132=FACE_OUTER_BOUND('',#7206,.T.);
#5133=FACE_OUTER_BOUND('',#7207,.T.);
#5134=FACE_OUTER_BOUND('',#7208,.T.);
#5135=FACE_OUTER_BOUND('',#7209,.T.);
#5136=FACE_OUTER_BOUND('',#7210,.T.);
#5137=FACE_OUTER_BOUND('',#7211,.T.);
#5138=FACE_OUTER_BOUND('',#7212,.T.);
#5139=FACE_OUTER_BOUND('',#7213,.T.);
#5140=FACE_OUTER_BOUND('',#7214,.T.);
#5141=FACE_OUTER_BOUND('',#7215,.T.);
#5142=FACE_OUTER_BOUND('',#7216,.T.);
#5143=FACE_OUTER_BOUND('',#7217,.T.);
#5144=FACE_OUTER_BOUND('',#7218,.T.);
#5145=FACE_OUTER_BOUND('',#7219,.T.);
#5146=FACE_OUTER_BOUND('',#7220,.T.);
#5147=FACE_OUTER_BOUND('',#7221,.T.);
#5148=FACE_OUTER_BOUND('',#7222,.T.);
#5149=FACE_OUTER_BOUND('',#7223,.T.);
#5150=FACE_OUTER_BOUND('',#7224,.T.);
#5151=FACE_OUTER_BOUND('',#7225,.T.);
#5152=FACE_OUTER_BOUND('',#7226,.T.);
#5153=FACE_OUTER_BOUND('',#7227,.T.);
#5154=FACE_OUTER_BOUND('',#7228,.T.);
#5155=FACE_OUTER_BOUND('',#7229,.T.);
#5156=FACE_OUTER_BOUND('',#7240,.T.);
#5157=FACE_OUTER_BOUND('',#7241,.T.);
#5158=FACE_OUTER_BOUND('',#7252,.T.);
#5159=FACE_OUTER_BOUND('',#7253,.T.);
#5160=FACE_OUTER_BOUND('',#7254,.T.);
#5161=FACE_OUTER_BOUND('',#7255,.T.);
#5162=FACE_OUTER_BOUND('',#7256,.T.);
#5163=FACE_OUTER_BOUND('',#7257,.T.);
#5164=FACE_OUTER_BOUND('',#7258,.T.);
#5165=FACE_OUTER_BOUND('',#7259,.T.);
#5166=FACE_OUTER_BOUND('',#7260,.T.);
#5167=FACE_OUTER_BOUND('',#7261,.T.);
#5168=FACE_OUTER_BOUND('',#7262,.T.);
#5169=FACE_OUTER_BOUND('',#7269,.T.);
#5170=FACE_OUTER_BOUND('',#7276,.T.);
#5171=FACE_OUTER_BOUND('',#7277,.T.);
#5172=FACE_OUTER_BOUND('',#7278,.T.);
#5173=FACE_OUTER_BOUND('',#7279,.T.);
#5174=FACE_OUTER_BOUND('',#7280,.T.);
#5175=FACE_OUTER_BOUND('',#7281,.T.);
#5176=FACE_OUTER_BOUND('',#7282,.T.);
#5177=FACE_OUTER_BOUND('',#7283,.T.);
#5178=FACE_OUTER_BOUND('',#7284,.T.);
#5179=FACE_OUTER_BOUND('',#7285,.T.);
#5180=FACE_OUTER_BOUND('',#7286,.T.);
#5181=FACE_OUTER_BOUND('',#7287,.T.);
#5182=FACE_OUTER_BOUND('',#7288,.T.);
#5183=FACE_OUTER_BOUND('',#7289,.T.);
#5184=FACE_OUTER_BOUND('',#7290,.T.);
#5185=FACE_OUTER_BOUND('',#7291,.T.);
#5186=FACE_OUTER_BOUND('',#7292,.T.);
#5187=FACE_OUTER_BOUND('',#7293,.T.);
#5188=FACE_OUTER_BOUND('',#7294,.T.);
#5189=FACE_OUTER_BOUND('',#7295,.T.);
#5190=FACE_OUTER_BOUND('',#7296,.T.);
#5191=FACE_OUTER_BOUND('',#7297,.T.);
#5192=FACE_OUTER_BOUND('',#7298,.T.);
#5193=FACE_OUTER_BOUND('',#7304,.T.);
#5194=FACE_OUTER_BOUND('',#7310,.T.);
#5195=FACE_OUTER_BOUND('',#7311,.T.);
#5196=FACE_OUTER_BOUND('',#7312,.T.);
#5197=FACE_OUTER_BOUND('',#7313,.T.);
#5198=FACE_OUTER_BOUND('',#7314,.T.);
#5199=FACE_OUTER_BOUND('',#7315,.T.);
#5200=FACE_OUTER_BOUND('',#7316,.T.);
#5201=FACE_OUTER_BOUND('',#7317,.T.);
#5202=FACE_OUTER_BOUND('',#7319,.T.);
#5203=FACE_OUTER_BOUND('',#7321,.T.);
#5204=FACE_OUTER_BOUND('',#7322,.T.);
#5205=FACE_OUTER_BOUND('',#7324,.T.);
#5206=FACE_OUTER_BOUND('',#7325,.T.);
#5207=FACE_OUTER_BOUND('',#7326,.T.);
#5208=FACE_OUTER_BOUND('',#7327,.T.);
#5209=FACE_OUTER_BOUND('',#7328,.T.);
#5210=FACE_OUTER_BOUND('',#7329,.T.);
#5211=FACE_OUTER_BOUND('',#7330,.T.);
#5212=FACE_OUTER_BOUND('',#7331,.T.);
#5213=FACE_OUTER_BOUND('',#7332,.T.);
#5214=FACE_OUTER_BOUND('',#7333,.T.);
#5215=FACE_OUTER_BOUND('',#7334,.T.);
#5216=FACE_OUTER_BOUND('',#7335,.T.);
#5217=FACE_OUTER_BOUND('',#7336,.T.);
#5218=FACE_OUTER_BOUND('',#7337,.T.);
#5219=FACE_OUTER_BOUND('',#7338,.T.);
#5220=FACE_OUTER_BOUND('',#7339,.T.);
#5221=FACE_OUTER_BOUND('',#7340,.T.);
#5222=FACE_OUTER_BOUND('',#7342,.T.);
#5223=FACE_OUTER_BOUND('',#7343,.T.);
#5224=FACE_OUTER_BOUND('',#7344,.T.);
#5225=FACE_OUTER_BOUND('',#7346,.T.);
#5226=FACE_OUTER_BOUND('',#7347,.T.);
#5227=FACE_OUTER_BOUND('',#7348,.T.);
#5228=FACE_OUTER_BOUND('',#7349,.T.);
#5229=FACE_OUTER_BOUND('',#7351,.T.);
#5230=FACE_OUTER_BOUND('',#7352,.T.);
#5231=FACE_OUTER_BOUND('',#7353,.T.);
#5232=FACE_OUTER_BOUND('',#7354,.T.);
#5233=FACE_OUTER_BOUND('',#7356,.T.);
#5234=FACE_OUTER_BOUND('',#7357,.T.);
#5235=FACE_OUTER_BOUND('',#7358,.T.);
#5236=FACE_OUTER_BOUND('',#7359,.T.);
#5237=FACE_OUTER_BOUND('',#7360,.T.);
#5238=FACE_OUTER_BOUND('',#7361,.T.);
#5239=FACE_OUTER_BOUND('',#7362,.T.);
#5240=FACE_OUTER_BOUND('',#7364,.T.);
#5241=FACE_OUTER_BOUND('',#7365,.T.);
#5242=FACE_OUTER_BOUND('',#7366,.T.);
#5243=FACE_OUTER_BOUND('',#7367,.T.);
#5244=FACE_OUTER_BOUND('',#7368,.T.);
#5245=FACE_OUTER_BOUND('',#7370,.T.);
#5246=FACE_OUTER_BOUND('',#7371,.T.);
#5247=FACE_OUTER_BOUND('',#7372,.T.);
#5248=FACE_OUTER_BOUND('',#7373,.T.);
#5249=FACE_OUTER_BOUND('',#7374,.T.);
#5250=FACE_OUTER_BOUND('',#7375,.T.);
#5251=FACE_OUTER_BOUND('',#7376,.T.);
#5252=FACE_OUTER_BOUND('',#7377,.T.);
#5253=FACE_OUTER_BOUND('',#7378,.T.);
#5254=FACE_OUTER_BOUND('',#7379,.T.);
#5255=FACE_OUTER_BOUND('',#7380,.T.);
#5256=FACE_OUTER_BOUND('',#7381,.T.);
#5257=FACE_OUTER_BOUND('',#7383,.T.);
#5258=FACE_OUTER_BOUND('',#7384,.T.);
#5259=FACE_OUTER_BOUND('',#7385,.T.);
#5260=FACE_OUTER_BOUND('',#7387,.T.);
#5261=FACE_OUTER_BOUND('',#7388,.T.);
#5262=FACE_OUTER_BOUND('',#7389,.T.);
#5263=FACE_OUTER_BOUND('',#7390,.T.);
#5264=FACE_OUTER_BOUND('',#7391,.T.);
#5265=FACE_OUTER_BOUND('',#7393,.T.);
#5266=FACE_OUTER_BOUND('',#7394,.T.);
#5267=FACE_OUTER_BOUND('',#7395,.T.);
#5268=FACE_OUTER_BOUND('',#7397,.T.);
#5269=FACE_OUTER_BOUND('',#7398,.T.);
#5270=FACE_OUTER_BOUND('',#7399,.T.);
#5271=FACE_OUTER_BOUND('',#7401,.T.);
#5272=FACE_OUTER_BOUND('',#7403,.T.);
#5273=FACE_OUTER_BOUND('',#7404,.T.);
#5274=FACE_OUTER_BOUND('',#7405,.T.);
#5275=FACE_OUTER_BOUND('',#7407,.T.);
#5276=FACE_OUTER_BOUND('',#7408,.T.);
#5277=FACE_OUTER_BOUND('',#7410,.T.);
#5278=FACE_OUTER_BOUND('',#7411,.T.);
#5279=FACE_OUTER_BOUND('',#7412,.T.);
#5280=FACE_OUTER_BOUND('',#7413,.T.);
#5281=FACE_OUTER_BOUND('',#7414,.T.);
#5282=FACE_OUTER_BOUND('',#7415,.T.);
#5283=FACE_OUTER_BOUND('',#7416,.T.);
#5284=FACE_OUTER_BOUND('',#7417,.T.);
#5285=FACE_OUTER_BOUND('',#7418,.T.);
#5286=FACE_OUTER_BOUND('',#7419,.T.);
#5287=FACE_OUTER_BOUND('',#7420,.T.);
#5288=FACE_OUTER_BOUND('',#7421,.T.);
#5289=FACE_OUTER_BOUND('',#7422,.T.);
#5290=FACE_OUTER_BOUND('',#7423,.T.);
#5291=FACE_OUTER_BOUND('',#7424,.T.);
#5292=FACE_OUTER_BOUND('',#7425,.T.);
#5293=FACE_OUTER_BOUND('',#7426,.T.);
#5294=FACE_OUTER_BOUND('',#7427,.T.);
#5295=FACE_OUTER_BOUND('',#7428,.T.);
#5296=FACE_OUTER_BOUND('',#7429,.T.);
#5297=FACE_OUTER_BOUND('',#7430,.T.);
#5298=FACE_OUTER_BOUND('',#7431,.T.);
#5299=FACE_OUTER_BOUND('',#7432,.T.);
#5300=FACE_OUTER_BOUND('',#7433,.T.);
#5301=FACE_OUTER_BOUND('',#7434,.T.);
#5302=FACE_OUTER_BOUND('',#7435,.T.);
#5303=FACE_OUTER_BOUND('',#7436,.T.);
#5304=FACE_OUTER_BOUND('',#7437,.T.);
#5305=FACE_OUTER_BOUND('',#7438,.T.);
#5306=FACE_OUTER_BOUND('',#7439,.T.);
#5307=FACE_OUTER_BOUND('',#7440,.T.);
#5308=FACE_OUTER_BOUND('',#7441,.T.);
#5309=FACE_OUTER_BOUND('',#7442,.T.);
#5310=FACE_OUTER_BOUND('',#7443,.T.);
#5311=FACE_OUTER_BOUND('',#7444,.T.);
#5312=FACE_OUTER_BOUND('',#7445,.T.);
#5313=FACE_OUTER_BOUND('',#7446,.T.);
#5314=FACE_OUTER_BOUND('',#7447,.T.);
#5315=FACE_OUTER_BOUND('',#7448,.T.);
#5316=FACE_OUTER_BOUND('',#7449,.T.);
#5317=FACE_OUTER_BOUND('',#7450,.T.);
#5318=FACE_OUTER_BOUND('',#7451,.T.);
#5319=FACE_OUTER_BOUND('',#7452,.T.);
#5320=FACE_OUTER_BOUND('',#7453,.T.);
#5321=FACE_OUTER_BOUND('',#7454,.T.);
#5322=FACE_OUTER_BOUND('',#7455,.T.);
#5323=FACE_OUTER_BOUND('',#7456,.T.);
#5324=FACE_OUTER_BOUND('',#7457,.T.);
#5325=FACE_OUTER_BOUND('',#7458,.T.);
#5326=FACE_OUTER_BOUND('',#7459,.T.);
#5327=FACE_OUTER_BOUND('',#7460,.T.);
#5328=FACE_OUTER_BOUND('',#7461,.T.);
#5329=FACE_OUTER_BOUND('',#7462,.T.);
#5330=FACE_OUTER_BOUND('',#7463,.T.);
#5331=FACE_OUTER_BOUND('',#7464,.T.);
#5332=FACE_OUTER_BOUND('',#7465,.T.);
#5333=FACE_OUTER_BOUND('',#7466,.T.);
#5334=FACE_OUTER_BOUND('',#7467,.T.);
#5335=FACE_OUTER_BOUND('',#7468,.T.);
#5336=FACE_OUTER_BOUND('',#7469,.T.);
#5337=FACE_OUTER_BOUND('',#7470,.T.);
#5338=FACE_OUTER_BOUND('',#7471,.T.);
#5339=FACE_OUTER_BOUND('',#7472,.T.);
#5340=FACE_OUTER_BOUND('',#7473,.T.);
#5341=FACE_OUTER_BOUND('',#7474,.T.);
#5342=FACE_OUTER_BOUND('',#7475,.T.);
#5343=FACE_OUTER_BOUND('',#7476,.T.);
#5344=FACE_OUTER_BOUND('',#7477,.T.);
#5345=FACE_OUTER_BOUND('',#7478,.T.);
#5346=FACE_OUTER_BOUND('',#7479,.T.);
#5347=FACE_OUTER_BOUND('',#7480,.T.);
#5348=FACE_OUTER_BOUND('',#7481,.T.);
#5349=FACE_OUTER_BOUND('',#7482,.T.);
#5350=FACE_OUTER_BOUND('',#7483,.T.);
#5351=FACE_OUTER_BOUND('',#7484,.T.);
#5352=FACE_OUTER_BOUND('',#7485,.T.);
#5353=FACE_OUTER_BOUND('',#7486,.T.);
#5354=FACE_OUTER_BOUND('',#7487,.T.);
#5355=FACE_OUTER_BOUND('',#7488,.T.);
#5356=FACE_OUTER_BOUND('',#7489,.T.);
#5357=FACE_OUTER_BOUND('',#7490,.T.);
#5358=FACE_OUTER_BOUND('',#7491,.T.);
#5359=FACE_OUTER_BOUND('',#7492,.T.);
#5360=FACE_OUTER_BOUND('',#7493,.T.);
#5361=FACE_OUTER_BOUND('',#7494,.T.);
#5362=FACE_OUTER_BOUND('',#7495,.T.);
#5363=FACE_OUTER_BOUND('',#7496,.T.);
#5364=FACE_OUTER_BOUND('',#7497,.T.);
#5365=FACE_OUTER_BOUND('',#7498,.T.);
#5366=FACE_OUTER_BOUND('',#7499,.T.);
#5367=FACE_OUTER_BOUND('',#7500,.T.);
#5368=FACE_OUTER_BOUND('',#7501,.T.);
#5369=FACE_OUTER_BOUND('',#7502,.T.);
#5370=FACE_OUTER_BOUND('',#7503,.T.);
#5371=FACE_OUTER_BOUND('',#7504,.T.);
#5372=FACE_OUTER_BOUND('',#7505,.T.);
#5373=FACE_OUTER_BOUND('',#7506,.T.);
#5374=FACE_OUTER_BOUND('',#7507,.T.);
#5375=FACE_OUTER_BOUND('',#7508,.T.);
#5376=FACE_OUTER_BOUND('',#7509,.T.);
#5377=FACE_OUTER_BOUND('',#7510,.T.);
#5378=FACE_OUTER_BOUND('',#7511,.T.);
#5379=FACE_OUTER_BOUND('',#7512,.T.);
#5380=FACE_OUTER_BOUND('',#7513,.T.);
#5381=FACE_OUTER_BOUND('',#7514,.T.);
#5382=FACE_OUTER_BOUND('',#7515,.T.);
#5383=FACE_OUTER_BOUND('',#7516,.T.);
#5384=FACE_OUTER_BOUND('',#7517,.T.);
#5385=FACE_OUTER_BOUND('',#7518,.T.);
#5386=FACE_OUTER_BOUND('',#7519,.T.);
#5387=FACE_OUTER_BOUND('',#7520,.T.);
#5388=FACE_OUTER_BOUND('',#7521,.T.);
#5389=FACE_OUTER_BOUND('',#7522,.T.);
#5390=FACE_OUTER_BOUND('',#7523,.T.);
#5391=FACE_OUTER_BOUND('',#7524,.T.);
#5392=FACE_OUTER_BOUND('',#7525,.T.);
#5393=FACE_OUTER_BOUND('',#7526,.T.);
#5394=FACE_OUTER_BOUND('',#7527,.T.);
#5395=FACE_OUTER_BOUND('',#7528,.T.);
#5396=FACE_OUTER_BOUND('',#7529,.T.);
#5397=FACE_OUTER_BOUND('',#7530,.T.);
#5398=FACE_OUTER_BOUND('',#7531,.T.);
#5399=FACE_OUTER_BOUND('',#7532,.T.);
#5400=FACE_OUTER_BOUND('',#7533,.T.);
#5401=FACE_OUTER_BOUND('',#7534,.T.);
#5402=FACE_OUTER_BOUND('',#7535,.T.);
#5403=FACE_OUTER_BOUND('',#7536,.T.);
#5404=FACE_OUTER_BOUND('',#7537,.T.);
#5405=FACE_OUTER_BOUND('',#7538,.T.);
#5406=FACE_OUTER_BOUND('',#7539,.T.);
#5407=FACE_OUTER_BOUND('',#7540,.T.);
#5408=FACE_OUTER_BOUND('',#7541,.T.);
#5409=FACE_OUTER_BOUND('',#7542,.T.);
#5410=FACE_OUTER_BOUND('',#7543,.T.);
#5411=FACE_OUTER_BOUND('',#7544,.T.);
#5412=FACE_OUTER_BOUND('',#7545,.T.);
#5413=FACE_OUTER_BOUND('',#7546,.T.);
#5414=FACE_OUTER_BOUND('',#7547,.T.);
#5415=FACE_OUTER_BOUND('',#7548,.T.);
#5416=FACE_OUTER_BOUND('',#7549,.T.);
#5417=FACE_OUTER_BOUND('',#7550,.T.);
#5418=FACE_OUTER_BOUND('',#7551,.T.);
#5419=FACE_OUTER_BOUND('',#7552,.T.);
#5420=FACE_OUTER_BOUND('',#7553,.T.);
#5421=FACE_OUTER_BOUND('',#7554,.T.);
#5422=FACE_OUTER_BOUND('',#7555,.T.);
#5423=FACE_OUTER_BOUND('',#7556,.T.);
#5424=FACE_OUTER_BOUND('',#7557,.T.);
#5425=FACE_OUTER_BOUND('',#7558,.T.);
#5426=FACE_OUTER_BOUND('',#7559,.T.);
#5427=FACE_OUTER_BOUND('',#7560,.T.);
#5428=FACE_OUTER_BOUND('',#7561,.T.);
#5429=FACE_OUTER_BOUND('',#7562,.T.);
#5430=FACE_OUTER_BOUND('',#7563,.T.);
#5431=FACE_OUTER_BOUND('',#7564,.T.);
#5432=FACE_OUTER_BOUND('',#7565,.T.);
#5433=FACE_OUTER_BOUND('',#7566,.T.);
#5434=FACE_OUTER_BOUND('',#7567,.T.);
#5435=FACE_OUTER_BOUND('',#7568,.T.);
#5436=FACE_OUTER_BOUND('',#7569,.T.);
#5437=FACE_OUTER_BOUND('',#7570,.T.);
#5438=FACE_OUTER_BOUND('',#7571,.T.);
#5439=FACE_OUTER_BOUND('',#7572,.T.);
#5440=FACE_OUTER_BOUND('',#7573,.T.);
#5441=FACE_OUTER_BOUND('',#7574,.T.);
#5442=FACE_OUTER_BOUND('',#7575,.T.);
#5443=FACE_OUTER_BOUND('',#7576,.T.);
#5444=FACE_OUTER_BOUND('',#7577,.T.);
#5445=FACE_OUTER_BOUND('',#7578,.T.);
#5446=FACE_OUTER_BOUND('',#7579,.T.);
#5447=FACE_OUTER_BOUND('',#7580,.T.);
#5448=FACE_OUTER_BOUND('',#7581,.T.);
#5449=FACE_OUTER_BOUND('',#7582,.T.);
#5450=FACE_OUTER_BOUND('',#7583,.T.);
#5451=FACE_OUTER_BOUND('',#7584,.T.);
#5452=FACE_OUTER_BOUND('',#7585,.T.);
#5453=FACE_OUTER_BOUND('',#7586,.T.);
#5454=FACE_OUTER_BOUND('',#7587,.T.);
#5455=FACE_OUTER_BOUND('',#7588,.T.);
#5456=FACE_OUTER_BOUND('',#7589,.T.);
#5457=FACE_OUTER_BOUND('',#7590,.T.);
#5458=FACE_OUTER_BOUND('',#7591,.T.);
#5459=FACE_OUTER_BOUND('',#7592,.T.);
#5460=FACE_OUTER_BOUND('',#7593,.T.);
#5461=FACE_OUTER_BOUND('',#7594,.T.);
#5462=FACE_OUTER_BOUND('',#7595,.T.);
#5463=FACE_OUTER_BOUND('',#7596,.T.);
#5464=FACE_OUTER_BOUND('',#7597,.T.);
#5465=FACE_OUTER_BOUND('',#7598,.T.);
#5466=FACE_OUTER_BOUND('',#7599,.T.);
#5467=FACE_OUTER_BOUND('',#7600,.T.);
#5468=FACE_OUTER_BOUND('',#7601,.T.);
#5469=FACE_OUTER_BOUND('',#7602,.T.);
#5470=FACE_OUTER_BOUND('',#7603,.T.);
#5471=FACE_OUTER_BOUND('',#7604,.T.);
#5472=FACE_OUTER_BOUND('',#7605,.T.);
#5473=FACE_OUTER_BOUND('',#7606,.T.);
#5474=FACE_OUTER_BOUND('',#7608,.T.);
#5475=FACE_OUTER_BOUND('',#7609,.T.);
#5476=FACE_OUTER_BOUND('',#7610,.T.);
#5477=FACE_OUTER_BOUND('',#7612,.T.);
#5478=FACE_OUTER_BOUND('',#7613,.T.);
#5479=FACE_OUTER_BOUND('',#7615,.T.);
#5480=FACE_OUTER_BOUND('',#7616,.T.);
#5481=FACE_OUTER_BOUND('',#7617,.T.);
#5482=FACE_OUTER_BOUND('',#7618,.T.);
#5483=FACE_OUTER_BOUND('',#7619,.T.);
#5484=FACE_OUTER_BOUND('',#7620,.T.);
#5485=FACE_OUTER_BOUND('',#7621,.T.);
#5486=FACE_OUTER_BOUND('',#7622,.T.);
#5487=FACE_OUTER_BOUND('',#7623,.T.);
#5488=FACE_OUTER_BOUND('',#7624,.T.);
#5489=FACE_OUTER_BOUND('',#7625,.T.);
#5490=FACE_OUTER_BOUND('',#7626,.T.);
#5491=FACE_OUTER_BOUND('',#7627,.T.);
#5492=FACE_OUTER_BOUND('',#7628,.T.);
#5493=FACE_OUTER_BOUND('',#7629,.T.);
#5494=FACE_OUTER_BOUND('',#7630,.T.);
#5495=FACE_OUTER_BOUND('',#7631,.T.);
#5496=FACE_OUTER_BOUND('',#7632,.T.);
#5497=FACE_OUTER_BOUND('',#7633,.T.);
#5498=FACE_OUTER_BOUND('',#7634,.T.);
#5499=FACE_OUTER_BOUND('',#7635,.T.);
#5500=FACE_OUTER_BOUND('',#7636,.T.);
#5501=FACE_OUTER_BOUND('',#7637,.T.);
#5502=FACE_OUTER_BOUND('',#7638,.T.);
#5503=FACE_OUTER_BOUND('',#7639,.T.);
#5504=FACE_OUTER_BOUND('',#7640,.T.);
#5505=FACE_OUTER_BOUND('',#7641,.T.);
#5506=FACE_OUTER_BOUND('',#7642,.T.);
#5507=FACE_OUTER_BOUND('',#7643,.T.);
#5508=FACE_OUTER_BOUND('',#7644,.T.);
#5509=FACE_OUTER_BOUND('',#7645,.T.);
#5510=FACE_OUTER_BOUND('',#7646,.T.);
#5511=FACE_OUTER_BOUND('',#7647,.T.);
#5512=FACE_OUTER_BOUND('',#7648,.T.);
#5513=FACE_OUTER_BOUND('',#7649,.T.);
#5514=FACE_OUTER_BOUND('',#7650,.T.);
#5515=FACE_OUTER_BOUND('',#7651,.T.);
#5516=FACE_OUTER_BOUND('',#7652,.T.);
#5517=FACE_OUTER_BOUND('',#7653,.T.);
#5518=FACE_OUTER_BOUND('',#7654,.T.);
#5519=FACE_OUTER_BOUND('',#7655,.T.);
#5520=FACE_OUTER_BOUND('',#7656,.T.);
#5521=FACE_OUTER_BOUND('',#7657,.T.);
#5522=FACE_OUTER_BOUND('',#7658,.T.);
#5523=FACE_OUTER_BOUND('',#7659,.T.);
#5524=FACE_OUTER_BOUND('',#7660,.T.);
#5525=FACE_OUTER_BOUND('',#7661,.T.);
#5526=FACE_OUTER_BOUND('',#7662,.T.);
#5527=FACE_OUTER_BOUND('',#7663,.T.);
#5528=FACE_OUTER_BOUND('',#7664,.T.);
#5529=FACE_OUTER_BOUND('',#7665,.T.);
#5530=FACE_OUTER_BOUND('',#7666,.T.);
#5531=FACE_OUTER_BOUND('',#7667,.T.);
#5532=FACE_OUTER_BOUND('',#7668,.T.);
#5533=FACE_OUTER_BOUND('',#7669,.T.);
#5534=FACE_OUTER_BOUND('',#7670,.T.);
#5535=FACE_OUTER_BOUND('',#7671,.T.);
#5536=FACE_OUTER_BOUND('',#7672,.T.);
#5537=FACE_OUTER_BOUND('',#7673,.T.);
#5538=FACE_OUTER_BOUND('',#7674,.T.);
#5539=FACE_OUTER_BOUND('',#7675,.T.);
#5540=FACE_OUTER_BOUND('',#7676,.T.);
#5541=FACE_OUTER_BOUND('',#7677,.T.);
#5542=FACE_OUTER_BOUND('',#7678,.T.);
#5543=FACE_OUTER_BOUND('',#7679,.T.);
#5544=FACE_OUTER_BOUND('',#7680,.T.);
#5545=FACE_OUTER_BOUND('',#7681,.T.);
#5546=FACE_OUTER_BOUND('',#7682,.T.);
#5547=FACE_OUTER_BOUND('',#7683,.T.);
#5548=FACE_OUTER_BOUND('',#7684,.T.);
#5549=FACE_OUTER_BOUND('',#7685,.T.);
#5550=FACE_OUTER_BOUND('',#7686,.T.);
#5551=FACE_OUTER_BOUND('',#7687,.T.);
#5552=FACE_OUTER_BOUND('',#7688,.T.);
#5553=FACE_OUTER_BOUND('',#7689,.T.);
#5554=FACE_OUTER_BOUND('',#7690,.T.);
#5555=FACE_OUTER_BOUND('',#7691,.T.);
#5556=FACE_OUTER_BOUND('',#7692,.T.);
#5557=FACE_OUTER_BOUND('',#7693,.T.);
#5558=FACE_OUTER_BOUND('',#7694,.T.);
#5559=FACE_OUTER_BOUND('',#7695,.T.);
#5560=FACE_OUTER_BOUND('',#7696,.T.);
#5561=FACE_OUTER_BOUND('',#7697,.T.);
#5562=FACE_OUTER_BOUND('',#7698,.T.);
#5563=FACE_OUTER_BOUND('',#7699,.T.);
#5564=FACE_OUTER_BOUND('',#7700,.T.);
#5565=FACE_OUTER_BOUND('',#7701,.T.);
#5566=FACE_OUTER_BOUND('',#7702,.T.);
#5567=FACE_OUTER_BOUND('',#7703,.T.);
#5568=FACE_OUTER_BOUND('',#7704,.T.);
#5569=FACE_OUTER_BOUND('',#7705,.T.);
#5570=FACE_OUTER_BOUND('',#7706,.T.);
#5571=FACE_OUTER_BOUND('',#7707,.T.);
#5572=FACE_OUTER_BOUND('',#7708,.T.);
#5573=FACE_OUTER_BOUND('',#7709,.T.);
#5574=FACE_OUTER_BOUND('',#7710,.T.);
#5575=FACE_OUTER_BOUND('',#7711,.T.);
#5576=FACE_OUTER_BOUND('',#7712,.T.);
#5577=FACE_OUTER_BOUND('',#7713,.T.);
#5578=FACE_OUTER_BOUND('',#7714,.T.);
#5579=FACE_OUTER_BOUND('',#7715,.T.);
#5580=FACE_OUTER_BOUND('',#7716,.T.);
#5581=FACE_OUTER_BOUND('',#7717,.T.);
#5582=FACE_OUTER_BOUND('',#7718,.T.);
#5583=FACE_OUTER_BOUND('',#7719,.T.);
#5584=FACE_OUTER_BOUND('',#7720,.T.);
#5585=FACE_OUTER_BOUND('',#7721,.T.);
#5586=FACE_OUTER_BOUND('',#7722,.T.);
#5587=FACE_OUTER_BOUND('',#7723,.T.);
#5588=FACE_OUTER_BOUND('',#7724,.T.);
#5589=FACE_OUTER_BOUND('',#7725,.T.);
#5590=FACE_OUTER_BOUND('',#7726,.T.);
#5591=FACE_OUTER_BOUND('',#7727,.T.);
#5592=FACE_OUTER_BOUND('',#7728,.T.);
#5593=FACE_OUTER_BOUND('',#7729,.T.);
#5594=FACE_OUTER_BOUND('',#7730,.T.);
#5595=FACE_OUTER_BOUND('',#7731,.T.);
#5596=FACE_OUTER_BOUND('',#7732,.T.);
#5597=FACE_OUTER_BOUND('',#7733,.T.);
#5598=FACE_OUTER_BOUND('',#7734,.T.);
#5599=FACE_OUTER_BOUND('',#7735,.T.);
#5600=FACE_OUTER_BOUND('',#7736,.T.);
#5601=FACE_OUTER_BOUND('',#7737,.T.);
#5602=FACE_OUTER_BOUND('',#7738,.T.);
#5603=FACE_OUTER_BOUND('',#7739,.T.);
#5604=FACE_OUTER_BOUND('',#7740,.T.);
#5605=FACE_OUTER_BOUND('',#7741,.T.);
#5606=FACE_OUTER_BOUND('',#7742,.T.);
#5607=FACE_OUTER_BOUND('',#7743,.T.);
#5608=FACE_OUTER_BOUND('',#7744,.T.);
#5609=FACE_OUTER_BOUND('',#7745,.T.);
#5610=FACE_OUTER_BOUND('',#7746,.T.);
#5611=FACE_OUTER_BOUND('',#7747,.T.);
#5612=FACE_OUTER_BOUND('',#7748,.T.);
#5613=FACE_OUTER_BOUND('',#7749,.T.);
#5614=FACE_OUTER_BOUND('',#7750,.T.);
#5615=FACE_OUTER_BOUND('',#7751,.T.);
#5616=FACE_OUTER_BOUND('',#7752,.T.);
#5617=FACE_OUTER_BOUND('',#7753,.T.);
#5618=FACE_OUTER_BOUND('',#7754,.T.);
#5619=FACE_OUTER_BOUND('',#7755,.T.);
#5620=FACE_OUTER_BOUND('',#7756,.T.);
#5621=FACE_OUTER_BOUND('',#7757,.T.);
#5622=FACE_OUTER_BOUND('',#7758,.T.);
#5623=FACE_OUTER_BOUND('',#7759,.T.);
#5624=FACE_OUTER_BOUND('',#7760,.T.);
#5625=FACE_OUTER_BOUND('',#7761,.T.);
#5626=FACE_OUTER_BOUND('',#7762,.T.);
#5627=FACE_OUTER_BOUND('',#7763,.T.);
#5628=FACE_OUTER_BOUND('',#7764,.T.);
#5629=FACE_OUTER_BOUND('',#7765,.T.);
#5630=FACE_OUTER_BOUND('',#7766,.T.);
#5631=FACE_OUTER_BOUND('',#7767,.T.);
#5632=FACE_OUTER_BOUND('',#7768,.T.);
#5633=FACE_OUTER_BOUND('',#7769,.T.);
#5634=FACE_OUTER_BOUND('',#7770,.T.);
#5635=FACE_OUTER_BOUND('',#7771,.T.);
#5636=FACE_OUTER_BOUND('',#7772,.T.);
#5637=FACE_OUTER_BOUND('',#7773,.T.);
#5638=FACE_OUTER_BOUND('',#7774,.T.);
#5639=FACE_OUTER_BOUND('',#7775,.T.);
#5640=FACE_OUTER_BOUND('',#7776,.T.);
#5641=FACE_OUTER_BOUND('',#7777,.T.);
#5642=FACE_OUTER_BOUND('',#7778,.T.);
#5643=FACE_OUTER_BOUND('',#7779,.T.);
#5644=FACE_OUTER_BOUND('',#7781,.T.);
#5645=FACE_OUTER_BOUND('',#7782,.T.);
#5646=FACE_OUTER_BOUND('',#7783,.T.);
#5647=FACE_OUTER_BOUND('',#7784,.T.);
#5648=FACE_OUTER_BOUND('',#7785,.T.);
#5649=FACE_OUTER_BOUND('',#7786,.T.);
#5650=FACE_OUTER_BOUND('',#7788,.T.);
#5651=FACE_OUTER_BOUND('',#7790,.T.);
#5652=FACE_OUTER_BOUND('',#7791,.T.);
#5653=FACE_OUTER_BOUND('',#7792,.T.);
#5654=FACE_OUTER_BOUND('',#7793,.T.);
#5655=FACE_OUTER_BOUND('',#7794,.T.);
#5656=FACE_OUTER_BOUND('',#7795,.T.);
#5657=FACE_OUTER_BOUND('',#7796,.T.);
#5658=FACE_OUTER_BOUND('',#7798,.T.);
#5659=FACE_OUTER_BOUND('',#7800,.T.);
#5660=FACE_OUTER_BOUND('',#7801,.T.);
#5661=FACE_OUTER_BOUND('',#7802,.T.);
#5662=FACE_OUTER_BOUND('',#7803,.T.);
#5663=FACE_OUTER_BOUND('',#7804,.T.);
#5664=FACE_OUTER_BOUND('',#7805,.T.);
#5665=FACE_OUTER_BOUND('',#7806,.T.);
#5666=FACE_OUTER_BOUND('',#7808,.T.);
#5667=FACE_OUTER_BOUND('',#7809,.T.);
#5668=FACE_OUTER_BOUND('',#7811,.T.);
#5669=FACE_OUTER_BOUND('',#7812,.T.);
#5670=FACE_OUTER_BOUND('',#7814,.T.);
#5671=FACE_OUTER_BOUND('',#7815,.T.);
#5672=FACE_OUTER_BOUND('',#7817,.T.);
#5673=FACE_OUTER_BOUND('',#7818,.T.);
#5674=FACE_OUTER_BOUND('',#7819,.T.);
#5675=FACE_OUTER_BOUND('',#7820,.T.);
#5676=FACE_OUTER_BOUND('',#7821,.T.);
#5677=FACE_OUTER_BOUND('',#7822,.T.);
#5678=FACE_OUTER_BOUND('',#7824,.T.);
#5679=FACE_OUTER_BOUND('',#7825,.T.);
#5680=FACE_OUTER_BOUND('',#7827,.T.);
#5681=FACE_OUTER_BOUND('',#7828,.T.);
#5682=FACE_OUTER_BOUND('',#7829,.T.);
#5683=FACE_OUTER_BOUND('',#7830,.T.);
#5684=FACE_OUTER_BOUND('',#7831,.T.);
#5685=FACE_OUTER_BOUND('',#7832,.T.);
#5686=FACE_OUTER_BOUND('',#7833,.T.);
#5687=FACE_OUTER_BOUND('',#7834,.T.);
#5688=FACE_OUTER_BOUND('',#7835,.T.);
#5689=FACE_OUTER_BOUND('',#7836,.T.);
#5690=FACE_OUTER_BOUND('',#7837,.T.);
#5691=FACE_OUTER_BOUND('',#7838,.T.);
#5692=FACE_OUTER_BOUND('',#7839,.T.);
#5693=FACE_OUTER_BOUND('',#7840,.T.);
#5694=FACE_OUTER_BOUND('',#7842,.T.);
#5695=FACE_OUTER_BOUND('',#7843,.T.);
#5696=FACE_OUTER_BOUND('',#7844,.T.);
#5697=FACE_OUTER_BOUND('',#7849,.T.);
#5698=FACE_OUTER_BOUND('',#7850,.T.);
#5699=FACE_OUTER_BOUND('',#7851,.T.);
#5700=FACE_OUTER_BOUND('',#7852,.T.);
#5701=FACE_OUTER_BOUND('',#7853,.T.);
#5702=FACE_OUTER_BOUND('',#7854,.T.);
#5703=FACE_OUTER_BOUND('',#7855,.T.);
#5704=FACE_OUTER_BOUND('',#7856,.T.);
#5705=FACE_OUTER_BOUND('',#7857,.T.);
#5706=FACE_OUTER_BOUND('',#7858,.T.);
#5707=FACE_OUTER_BOUND('',#7859,.T.);
#5708=FACE_OUTER_BOUND('',#7860,.T.);
#5709=FACE_OUTER_BOUND('',#7861,.T.);
#5710=FACE_OUTER_BOUND('',#7862,.T.);
#5711=FACE_OUTER_BOUND('',#7863,.T.);
#5712=FACE_OUTER_BOUND('',#7864,.T.);
#5713=FACE_OUTER_BOUND('',#7865,.T.);
#5714=FACE_OUTER_BOUND('',#7866,.T.);
#5715=FACE_OUTER_BOUND('',#7867,.T.);
#5716=FACE_OUTER_BOUND('',#7869,.T.);
#5717=FACE_OUTER_BOUND('',#7870,.T.);
#5718=FACE_OUTER_BOUND('',#7871,.T.);
#5719=FACE_OUTER_BOUND('',#7872,.T.);
#5720=FACE_OUTER_BOUND('',#7873,.T.);
#5721=FACE_OUTER_BOUND('',#7874,.T.);
#5722=FACE_OUTER_BOUND('',#7875,.T.);
#5723=FACE_OUTER_BOUND('',#7876,.T.);
#5724=FACE_OUTER_BOUND('',#7878,.T.);
#5725=FACE_OUTER_BOUND('',#7879,.T.);
#5726=FACE_OUTER_BOUND('',#7880,.T.);
#5727=FACE_OUTER_BOUND('',#7881,.T.);
#5728=FACE_OUTER_BOUND('',#7882,.T.);
#5729=FACE_OUTER_BOUND('',#7883,.T.);
#5730=FACE_OUTER_BOUND('',#7884,.T.);
#5731=FACE_OUTER_BOUND('',#7885,.T.);
#5732=FACE_OUTER_BOUND('',#7886,.T.);
#5733=FACE_OUTER_BOUND('',#7887,.T.);
#5734=FACE_OUTER_BOUND('',#7888,.T.);
#5735=FACE_OUTER_BOUND('',#7889,.T.);
#5736=FACE_OUTER_BOUND('',#7890,.T.);
#5737=FACE_OUTER_BOUND('',#7891,.T.);
#5738=FACE_OUTER_BOUND('',#7892,.T.);
#5739=FACE_OUTER_BOUND('',#7893,.T.);
#5740=FACE_OUTER_BOUND('',#7894,.T.);
#5741=FACE_OUTER_BOUND('',#7895,.T.);
#5742=FACE_OUTER_BOUND('',#7896,.T.);
#5743=FACE_OUTER_BOUND('',#7897,.T.);
#5744=FACE_OUTER_BOUND('',#7898,.T.);
#5745=FACE_OUTER_BOUND('',#7899,.T.);
#5746=FACE_OUTER_BOUND('',#7900,.T.);
#5747=FACE_OUTER_BOUND('',#7901,.T.);
#5748=FACE_OUTER_BOUND('',#7902,.T.);
#5749=FACE_OUTER_BOUND('',#7903,.T.);
#5750=FACE_OUTER_BOUND('',#7904,.T.);
#5751=FACE_OUTER_BOUND('',#7905,.T.);
#5752=FACE_OUTER_BOUND('',#7906,.T.);
#5753=FACE_OUTER_BOUND('',#7907,.T.);
#5754=FACE_OUTER_BOUND('',#7908,.T.);
#5755=FACE_OUTER_BOUND('',#7909,.T.);
#5756=FACE_OUTER_BOUND('',#7910,.T.);
#5757=FACE_OUTER_BOUND('',#7911,.T.);
#5758=FACE_OUTER_BOUND('',#7912,.T.);
#5759=FACE_OUTER_BOUND('',#7913,.T.);
#5760=FACE_OUTER_BOUND('',#7914,.T.);
#5761=FACE_OUTER_BOUND('',#7915,.T.);
#5762=FACE_OUTER_BOUND('',#7916,.T.);
#5763=FACE_OUTER_BOUND('',#7917,.T.);
#5764=FACE_OUTER_BOUND('',#7918,.T.);
#5765=FACE_OUTER_BOUND('',#7919,.T.);
#5766=FACE_OUTER_BOUND('',#7920,.T.);
#5767=FACE_OUTER_BOUND('',#7921,.T.);
#5768=FACE_OUTER_BOUND('',#7922,.T.);
#5769=FACE_OUTER_BOUND('',#7923,.T.);
#5770=FACE_OUTER_BOUND('',#7924,.T.);
#5771=FACE_OUTER_BOUND('',#7925,.T.);
#5772=FACE_OUTER_BOUND('',#7926,.T.);
#5773=FACE_OUTER_BOUND('',#7927,.T.);
#5774=FACE_OUTER_BOUND('',#7929,.T.);
#5775=FACE_OUTER_BOUND('',#7930,.T.);
#5776=FACE_OUTER_BOUND('',#7931,.T.);
#5777=FACE_OUTER_BOUND('',#7932,.T.);
#5778=FACE_OUTER_BOUND('',#7933,.T.);
#5779=FACE_OUTER_BOUND('',#7934,.T.);
#5780=FACE_OUTER_BOUND('',#7935,.T.);
#5781=FACE_OUTER_BOUND('',#7936,.T.);
#5782=FACE_OUTER_BOUND('',#7937,.T.);
#5783=FACE_OUTER_BOUND('',#7939,.T.);
#5784=FACE_OUTER_BOUND('',#7940,.T.);
#5785=FACE_OUTER_BOUND('',#7941,.T.);
#5786=FACE_OUTER_BOUND('',#7942,.T.);
#5787=FACE_OUTER_BOUND('',#7944,.T.);
#5788=FACE_OUTER_BOUND('',#7945,.T.);
#5789=FACE_OUTER_BOUND('',#7946,.T.);
#5790=FACE_OUTER_BOUND('',#7947,.T.);
#5791=FACE_OUTER_BOUND('',#7948,.T.);
#5792=FACE_OUTER_BOUND('',#7949,.T.);
#5793=FACE_OUTER_BOUND('',#7950,.T.);
#5794=FACE_OUTER_BOUND('',#7951,.T.);
#5795=FACE_OUTER_BOUND('',#7952,.T.);
#5796=FACE_OUTER_BOUND('',#7953,.T.);
#5797=FACE_OUTER_BOUND('',#7954,.T.);
#5798=FACE_OUTER_BOUND('',#7955,.T.);
#5799=FACE_OUTER_BOUND('',#7956,.T.);
#5800=FACE_OUTER_BOUND('',#7957,.T.);
#5801=FACE_OUTER_BOUND('',#7958,.T.);
#5802=FACE_OUTER_BOUND('',#7959,.T.);
#5803=FACE_OUTER_BOUND('',#7960,.T.);
#5804=FACE_OUTER_BOUND('',#7961,.T.);
#5805=FACE_OUTER_BOUND('',#7962,.T.);
#5806=FACE_OUTER_BOUND('',#7963,.T.);
#5807=FACE_OUTER_BOUND('',#7964,.T.);
#5808=FACE_OUTER_BOUND('',#7965,.T.);
#5809=FACE_OUTER_BOUND('',#7966,.T.);
#5810=FACE_OUTER_BOUND('',#7967,.T.);
#5811=FACE_OUTER_BOUND('',#7968,.T.);
#5812=FACE_OUTER_BOUND('',#7969,.T.);
#5813=FACE_OUTER_BOUND('',#7970,.T.);
#5814=FACE_OUTER_BOUND('',#7971,.T.);
#5815=FACE_OUTER_BOUND('',#7972,.T.);
#5816=FACE_OUTER_BOUND('',#7973,.T.);
#5817=FACE_OUTER_BOUND('',#7974,.T.);
#5818=FACE_OUTER_BOUND('',#7975,.T.);
#5819=FACE_OUTER_BOUND('',#7976,.T.);
#5820=FACE_OUTER_BOUND('',#7977,.T.);
#5821=FACE_OUTER_BOUND('',#7978,.T.);
#5822=FACE_OUTER_BOUND('',#7979,.T.);
#5823=FACE_OUTER_BOUND('',#7980,.T.);
#5824=FACE_OUTER_BOUND('',#7981,.T.);
#5825=FACE_OUTER_BOUND('',#7982,.T.);
#5826=FACE_OUTER_BOUND('',#7984,.T.);
#5827=FACE_OUTER_BOUND('',#7986,.T.);
#5828=FACE_OUTER_BOUND('',#7987,.T.);
#5829=FACE_OUTER_BOUND('',#7988,.T.);
#5830=FACE_OUTER_BOUND('',#7993,.T.);
#5831=FACE_OUTER_BOUND('',#7994,.T.);
#5832=FACE_OUTER_BOUND('',#7995,.T.);
#5833=FACE_OUTER_BOUND('',#7996,.T.);
#5834=FACE_OUTER_BOUND('',#7997,.T.);
#5835=FACE_OUTER_BOUND('',#7998,.T.);
#5836=FACE_OUTER_BOUND('',#7999,.T.);
#5837=FACE_OUTER_BOUND('',#8000,.T.);
#5838=FACE_OUTER_BOUND('',#8006,.T.);
#5839=FACE_OUTER_BOUND('',#8007,.T.);
#5840=FACE_OUTER_BOUND('',#8008,.T.);
#5841=FACE_OUTER_BOUND('',#8009,.T.);
#5842=FACE_OUTER_BOUND('',#8010,.T.);
#5843=FACE_OUTER_BOUND('',#8011,.T.);
#5844=FACE_OUTER_BOUND('',#8012,.T.);
#5845=FACE_OUTER_BOUND('',#8013,.T.);
#5846=FACE_OUTER_BOUND('',#8014,.T.);
#5847=FACE_OUTER_BOUND('',#8015,.T.);
#5848=FACE_OUTER_BOUND('',#8016,.T.);
#5849=FACE_OUTER_BOUND('',#8017,.T.);
#5850=FACE_OUTER_BOUND('',#8023,.T.);
#5851=FACE_OUTER_BOUND('',#8025,.T.);
#5852=FACE_OUTER_BOUND('',#8026,.T.);
#5853=FACE_OUTER_BOUND('',#8028,.T.);
#5854=FACE_OUTER_BOUND('',#8029,.T.);
#5855=FACE_OUTER_BOUND('',#8030,.T.);
#5856=FACE_OUTER_BOUND('',#8032,.T.);
#5857=FACE_OUTER_BOUND('',#8033,.T.);
#5858=FACE_OUTER_BOUND('',#8035,.T.);
#5859=FACE_OUTER_BOUND('',#8038,.T.);
#5860=FACE_OUTER_BOUND('',#8039,.T.);
#5861=FACE_OUTER_BOUND('',#8042,.T.);
#5862=FACE_OUTER_BOUND('',#8043,.T.);
#5863=FACE_OUTER_BOUND('',#8044,.T.);
#5864=FACE_OUTER_BOUND('',#8045,.T.);
#5865=FACE_OUTER_BOUND('',#8046,.T.);
#5866=FACE_OUTER_BOUND('',#8047,.T.);
#5867=FACE_OUTER_BOUND('',#8048,.T.);
#5868=FACE_OUTER_BOUND('',#8049,.T.);
#5869=FACE_OUTER_BOUND('',#8050,.T.);
#5870=FACE_OUTER_BOUND('',#8051,.T.);
#5871=FACE_OUTER_BOUND('',#8052,.T.);
#5872=FACE_OUTER_BOUND('',#8053,.T.);
#5873=FACE_OUTER_BOUND('',#8054,.T.);
#5874=FACE_OUTER_BOUND('',#8055,.T.);
#5875=FACE_OUTER_BOUND('',#8056,.T.);
#5876=FACE_OUTER_BOUND('',#8058,.T.);
#5877=FACE_OUTER_BOUND('',#8059,.T.);
#5878=FACE_OUTER_BOUND('',#8060,.T.);
#5879=FACE_OUTER_BOUND('',#8061,.T.);
#5880=FACE_OUTER_BOUND('',#8062,.T.);
#5881=FACE_OUTER_BOUND('',#8064,.T.);
#5882=FACE_OUTER_BOUND('',#8065,.T.);
#5883=FACE_OUTER_BOUND('',#8066,.T.);
#5884=FACE_OUTER_BOUND('',#8067,.T.);
#5885=FACE_OUTER_BOUND('',#8068,.T.);
#5886=FACE_OUTER_BOUND('',#8069,.T.);
#5887=FACE_OUTER_BOUND('',#8070,.T.);
#5888=FACE_OUTER_BOUND('',#8071,.T.);
#5889=FACE_OUTER_BOUND('',#8072,.T.);
#5890=FACE_OUTER_BOUND('',#8073,.T.);
#5891=FACE_OUTER_BOUND('',#8074,.T.);
#5892=FACE_OUTER_BOUND('',#8075,.T.);
#5893=FACE_OUTER_BOUND('',#8076,.T.);
#5894=FACE_OUTER_BOUND('',#8077,.T.);
#5895=FACE_OUTER_BOUND('',#8078,.T.);
#5896=FACE_OUTER_BOUND('',#8079,.T.);
#5897=FACE_OUTER_BOUND('',#8081,.T.);
#5898=FACE_OUTER_BOUND('',#8082,.T.);
#5899=FACE_OUTER_BOUND('',#8083,.T.);
#5900=FACE_OUTER_BOUND('',#8084,.T.);
#5901=FACE_OUTER_BOUND('',#8085,.T.);
#5902=FACE_OUTER_BOUND('',#8087,.T.);
#5903=FACE_OUTER_BOUND('',#8088,.T.);
#5904=FACE_OUTER_BOUND('',#8089,.T.);
#5905=FACE_OUTER_BOUND('',#8090,.T.);
#5906=FACE_OUTER_BOUND('',#8091,.T.);
#5907=FACE_OUTER_BOUND('',#8092,.T.);
#5908=FACE_OUTER_BOUND('',#8093,.T.);
#5909=FACE_OUTER_BOUND('',#8094,.T.);
#5910=FACE_OUTER_BOUND('',#8095,.T.);
#5911=FACE_OUTER_BOUND('',#8096,.T.);
#5912=FACE_OUTER_BOUND('',#8099,.T.);
#5913=FACE_OUTER_BOUND('',#8100,.T.);
#5914=FACE_OUTER_BOUND('',#8101,.T.);
#5915=FACE_OUTER_BOUND('',#8102,.T.);
#5916=FACE_OUTER_BOUND('',#8103,.T.);
#5917=FACE_OUTER_BOUND('',#8106,.T.);
#5918=FACE_OUTER_BOUND('',#8108,.T.);
#5919=FACE_OUTER_BOUND('',#8110,.T.);
#5920=FACE_OUTER_BOUND('',#8111,.T.);
#5921=FACE_OUTER_BOUND('',#8112,.T.);
#5922=FACE_OUTER_BOUND('',#8114,.T.);
#5923=FACE_OUTER_BOUND('',#8116,.T.);
#5924=FACE_OUTER_BOUND('',#8117,.T.);
#5925=FACE_OUTER_BOUND('',#8118,.T.);
#5926=FACE_OUTER_BOUND('',#8119,.T.);
#5927=FACE_OUTER_BOUND('',#8120,.T.);
#5928=FACE_OUTER_BOUND('',#8121,.T.);
#5929=FACE_OUTER_BOUND('',#8122,.T.);
#5930=FACE_OUTER_BOUND('',#8123,.T.);
#5931=FACE_OUTER_BOUND('',#8124,.T.);
#5932=FACE_OUTER_BOUND('',#8125,.T.);
#5933=FACE_OUTER_BOUND('',#8126,.T.);
#5934=FACE_OUTER_BOUND('',#8127,.T.);
#5935=FACE_OUTER_BOUND('',#8128,.T.);
#5936=FACE_OUTER_BOUND('',#8129,.T.);
#5937=FACE_OUTER_BOUND('',#8130,.T.);
#5938=FACE_OUTER_BOUND('',#8131,.T.);
#5939=FACE_OUTER_BOUND('',#8132,.T.);
#5940=FACE_OUTER_BOUND('',#8133,.T.);
#5941=FACE_OUTER_BOUND('',#8134,.T.);
#5942=FACE_OUTER_BOUND('',#8135,.T.);
#5943=FACE_OUTER_BOUND('',#8136,.T.);
#5944=FACE_OUTER_BOUND('',#8137,.T.);
#5945=FACE_OUTER_BOUND('',#8138,.T.);
#5946=FACE_OUTER_BOUND('',#8139,.T.);
#5947=FACE_OUTER_BOUND('',#8140,.T.);
#5948=FACE_OUTER_BOUND('',#8141,.T.);
#5949=FACE_OUTER_BOUND('',#8142,.T.);
#5950=FACE_OUTER_BOUND('',#8143,.T.);
#5951=FACE_OUTER_BOUND('',#8145,.T.);
#5952=FACE_OUTER_BOUND('',#8147,.T.);
#5953=FACE_OUTER_BOUND('',#8149,.T.);
#5954=FACE_OUTER_BOUND('',#8150,.T.);
#5955=FACE_OUTER_BOUND('',#8151,.T.);
#5956=FACE_OUTER_BOUND('',#8152,.T.);
#5957=FACE_OUTER_BOUND('',#8153,.T.);
#5958=FACE_OUTER_BOUND('',#8154,.T.);
#5959=FACE_OUTER_BOUND('',#8155,.T.);
#5960=FACE_OUTER_BOUND('',#8156,.T.);
#5961=FACE_OUTER_BOUND('',#8157,.T.);
#5962=FACE_OUTER_BOUND('',#8158,.T.);
#5963=FACE_OUTER_BOUND('',#8159,.T.);
#5964=FACE_OUTER_BOUND('',#8160,.T.);
#5965=FACE_OUTER_BOUND('',#8161,.T.);
#5966=FACE_OUTER_BOUND('',#8162,.T.);
#5967=FACE_OUTER_BOUND('',#8163,.T.);
#5968=FACE_OUTER_BOUND('',#8164,.T.);
#5969=FACE_OUTER_BOUND('',#8165,.T.);
#5970=FACE_OUTER_BOUND('',#8166,.T.);
#5971=FACE_OUTER_BOUND('',#8167,.T.);
#5972=FACE_OUTER_BOUND('',#8168,.T.);
#5973=FACE_OUTER_BOUND('',#8169,.T.);
#5974=FACE_OUTER_BOUND('',#8170,.T.);
#5975=FACE_OUTER_BOUND('',#8171,.T.);
#5976=FACE_OUTER_BOUND('',#8172,.T.);
#5977=FACE_OUTER_BOUND('',#8173,.T.);
#5978=FACE_OUTER_BOUND('',#8174,.T.);
#5979=FACE_OUTER_BOUND('',#8175,.T.);
#5980=FACE_OUTER_BOUND('',#8176,.T.);
#5981=FACE_OUTER_BOUND('',#8177,.T.);
#5982=FACE_OUTER_BOUND('',#8178,.T.);
#5983=FACE_OUTER_BOUND('',#8179,.T.);
#5984=FACE_OUTER_BOUND('',#8180,.T.);
#5985=FACE_OUTER_BOUND('',#8181,.T.);
#5986=FACE_OUTER_BOUND('',#8182,.T.);
#5987=FACE_OUTER_BOUND('',#8183,.T.);
#5988=FACE_OUTER_BOUND('',#8184,.T.);
#5989=FACE_OUTER_BOUND('',#8185,.T.);
#5990=FACE_OUTER_BOUND('',#8186,.T.);
#5991=FACE_OUTER_BOUND('',#8187,.T.);
#5992=FACE_OUTER_BOUND('',#8188,.T.);
#5993=FACE_OUTER_BOUND('',#8189,.T.);
#5994=FACE_OUTER_BOUND('',#8190,.T.);
#5995=FACE_OUTER_BOUND('',#8191,.T.);
#5996=FACE_OUTER_BOUND('',#8192,.T.);
#5997=FACE_OUTER_BOUND('',#8193,.T.);
#5998=FACE_OUTER_BOUND('',#8195,.T.);
#5999=FACE_OUTER_BOUND('',#8197,.T.);
#6000=FACE_OUTER_BOUND('',#8199,.T.);
#6001=FACE_OUTER_BOUND('',#8200,.T.);
#6002=FACE_OUTER_BOUND('',#8201,.T.);
#6003=FACE_OUTER_BOUND('',#8202,.T.);
#6004=FACE_OUTER_BOUND('',#8203,.T.);
#6005=FACE_OUTER_BOUND('',#8204,.T.);
#6006=FACE_OUTER_BOUND('',#8205,.T.);
#6007=FACE_OUTER_BOUND('',#8206,.T.);
#6008=FACE_OUTER_BOUND('',#8207,.T.);
#6009=FACE_OUTER_BOUND('',#8208,.T.);
#6010=FACE_OUTER_BOUND('',#8209,.T.);
#6011=FACE_OUTER_BOUND('',#8210,.T.);
#6012=FACE_OUTER_BOUND('',#8211,.T.);
#6013=FACE_OUTER_BOUND('',#8212,.T.);
#6014=FACE_OUTER_BOUND('',#8214,.T.);
#6015=FACE_OUTER_BOUND('',#8215,.T.);
#6016=FACE_OUTER_BOUND('',#8216,.T.);
#6017=FACE_OUTER_BOUND('',#8217,.T.);
#6018=FACE_OUTER_BOUND('',#8218,.T.);
#6019=FACE_OUTER_BOUND('',#8219,.T.);
#6020=FACE_OUTER_BOUND('',#8220,.T.);
#6021=FACE_OUTER_BOUND('',#8221,.T.);
#6022=FACE_OUTER_BOUND('',#8222,.T.);
#6023=FACE_OUTER_BOUND('',#8223,.T.);
#6024=FACE_OUTER_BOUND('',#8224,.T.);
#6025=FACE_OUTER_BOUND('',#8225,.T.);
#6026=FACE_OUTER_BOUND('',#8226,.T.);
#6027=FACE_OUTER_BOUND('',#8228,.T.);
#6028=FACE_OUTER_BOUND('',#8229,.T.);
#6029=FACE_OUTER_BOUND('',#8230,.T.);
#6030=FACE_OUTER_BOUND('',#8231,.T.);
#6031=FACE_OUTER_BOUND('',#8232,.T.);
#6032=FACE_OUTER_BOUND('',#8233,.T.);
#6033=FACE_OUTER_BOUND('',#8234,.T.);
#6034=FACE_OUTER_BOUND('',#8235,.T.);
#6035=FACE_OUTER_BOUND('',#8236,.T.);
#6036=FACE_OUTER_BOUND('',#8237,.T.);
#6037=FACE_OUTER_BOUND('',#8238,.T.);
#6038=FACE_OUTER_BOUND('',#8239,.T.);
#6039=FACE_OUTER_BOUND('',#8240,.T.);
#6040=FACE_OUTER_BOUND('',#8241,.T.);
#6041=FACE_OUTER_BOUND('',#8242,.T.);
#6042=FACE_OUTER_BOUND('',#8243,.T.);
#6043=FACE_OUTER_BOUND('',#8244,.T.);
#6044=FACE_OUTER_BOUND('',#8245,.T.);
#6045=FACE_OUTER_BOUND('',#8246,.T.);
#6046=FACE_OUTER_BOUND('',#8247,.T.);
#6047=FACE_OUTER_BOUND('',#8248,.T.);
#6048=FACE_OUTER_BOUND('',#8249,.T.);
#6049=FACE_OUTER_BOUND('',#8250,.T.);
#6050=FACE_OUTER_BOUND('',#8251,.T.);
#6051=FACE_OUTER_BOUND('',#8252,.T.);
#6052=FACE_OUTER_BOUND('',#8253,.T.);
#6053=FACE_OUTER_BOUND('',#8254,.T.);
#6054=FACE_OUTER_BOUND('',#8255,.T.);
#6055=FACE_OUTER_BOUND('',#8256,.T.);
#6056=FACE_OUTER_BOUND('',#8257,.T.);
#6057=FACE_OUTER_BOUND('',#8258,.T.);
#6058=FACE_OUTER_BOUND('',#8259,.T.);
#6059=FACE_OUTER_BOUND('',#8260,.T.);
#6060=FACE_OUTER_BOUND('',#8261,.T.);
#6061=FACE_OUTER_BOUND('',#8262,.T.);
#6062=FACE_OUTER_BOUND('',#8263,.T.);
#6063=FACE_OUTER_BOUND('',#8264,.T.);
#6064=FACE_OUTER_BOUND('',#8265,.T.);
#6065=FACE_OUTER_BOUND('',#8266,.T.);
#6066=FACE_OUTER_BOUND('',#8267,.T.);
#6067=FACE_OUTER_BOUND('',#8268,.T.);
#6068=FACE_OUTER_BOUND('',#8269,.T.);
#6069=FACE_OUTER_BOUND('',#8270,.T.);
#6070=FACE_OUTER_BOUND('',#8271,.T.);
#6071=FACE_OUTER_BOUND('',#8272,.T.);
#6072=FACE_OUTER_BOUND('',#8273,.T.);
#6073=FACE_OUTER_BOUND('',#8274,.T.);
#6074=FACE_OUTER_BOUND('',#8275,.T.);
#6075=FACE_OUTER_BOUND('',#8283,.T.);
#6076=FACE_OUTER_BOUND('',#8284,.T.);
#6077=FACE_OUTER_BOUND('',#8285,.T.);
#6078=FACE_OUTER_BOUND('',#8286,.T.);
#6079=FACE_OUTER_BOUND('',#8287,.T.);
#6080=FACE_OUTER_BOUND('',#8288,.T.);
#6081=FACE_OUTER_BOUND('',#8304,.T.);
#6082=FACE_OUTER_BOUND('',#8305,.T.);
#6083=FACE_OUTER_BOUND('',#8306,.T.);
#6084=FACE_OUTER_BOUND('',#8307,.T.);
#6085=FACE_OUTER_BOUND('',#8309,.T.);
#6086=FACE_OUTER_BOUND('',#8310,.T.);
#6087=FACE_OUTER_BOUND('',#8311,.T.);
#6088=FACE_OUTER_BOUND('',#8312,.T.);
#6089=FACE_OUTER_BOUND('',#8313,.T.);
#6090=FACE_OUTER_BOUND('',#8314,.T.);
#6091=FACE_OUTER_BOUND('',#8315,.T.);
#6092=FACE_OUTER_BOUND('',#8316,.T.);
#6093=FACE_OUTER_BOUND('',#8317,.T.);
#6094=FACE_OUTER_BOUND('',#8318,.T.);
#6095=FACE_OUTER_BOUND('',#8319,.T.);
#6096=FACE_OUTER_BOUND('',#8321,.T.);
#6097=FACE_OUTER_BOUND('',#8324,.T.);
#6098=FACE_OUTER_BOUND('',#8325,.T.);
#6099=FACE_OUTER_BOUND('',#8326,.T.);
#6100=FACE_OUTER_BOUND('',#8327,.T.);
#6101=FACE_OUTER_BOUND('',#8328,.T.);
#6102=FACE_OUTER_BOUND('',#8330,.T.);
#6103=FACE_OUTER_BOUND('',#8333,.T.);
#6104=FACE_OUTER_BOUND('',#8336,.T.);
#6105=FACE_OUTER_BOUND('',#8337,.T.);
#6106=FACE_OUTER_BOUND('',#8339,.T.);
#6107=FACE_OUTER_BOUND('',#8340,.T.);
#6108=FACE_OUTER_BOUND('',#8343,.T.);
#6109=FACE_OUTER_BOUND('',#8345,.T.);
#6110=EDGE_LOOP('',(#21458,#21459,#21460,#21461));
#6111=EDGE_LOOP('',(#21462,#21463,#21464,#21465));
#6112=EDGE_LOOP('',(#21466,#21467,#21468,#21469));
#6113=EDGE_LOOP('',(#21470,#21471,#21472,#21473,#21474,#21475,#21476,#21477,
#21478,#21479,#21480,#21481,#21482,#21483,#21484));
#6114=EDGE_LOOP('',(#21485,#21486,#21487,#21488));
#6115=EDGE_LOOP('',(#21489,#21490,#21491,#21492));
#6116=EDGE_LOOP('',(#21493,#21494,#21495,#21496));
#6117=EDGE_LOOP('',(#21497,#21498,#21499,#21500));
#6118=EDGE_LOOP('',(#21501,#21502,#21503,#21504));
#6119=EDGE_LOOP('',(#21505,#21506,#21507,#21508));
#6120=EDGE_LOOP('',(#21509,#21510,#21511,#21512));
#6121=EDGE_LOOP('',(#21513,#21514,#21515,#21516));
#6122=EDGE_LOOP('',(#21517,#21518,#21519,#21520));
#6123=EDGE_LOOP('',(#21521,#21522,#21523,#21524));
#6124=EDGE_LOOP('',(#21525,#21526,#21527,#21528));
#6125=EDGE_LOOP('',(#21529,#21530,#21531,#21532));
#6126=EDGE_LOOP('',(#21533,#21534,#21535,#21536));
#6127=EDGE_LOOP('',(#21537,#21538,#21539,#21540));
#6128=EDGE_LOOP('',(#21541,#21542,#21543,#21544));
#6129=EDGE_LOOP('',(#21545,#21546,#21547,#21548));
#6130=EDGE_LOOP('',(#21549,#21550,#21551,#21552));
#6131=EDGE_LOOP('',(#21553,#21554,#21555,#21556,#21557,#21558,#21559,#21560,
#21561,#21562,#21563,#21564,#21565,#21566,#21567));
#6132=EDGE_LOOP('',(#21568,#21569,#21570,#21571));
#6133=EDGE_LOOP('',(#21572,#21573,#21574,#21575,#21576,#21577,#21578,#21579));
#6134=EDGE_LOOP('',(#21580));
#6135=EDGE_LOOP('',(#21581));
#6136=EDGE_LOOP('',(#21582));
#6137=EDGE_LOOP('',(#21583));
#6138=EDGE_LOOP('',(#21584,#21585,#21586,#21587,#21588,#21589,#21590,#21591));
#6139=EDGE_LOOP('',(#21592,#21593,#21594,#21595));
#6140=EDGE_LOOP('',(#21596,#21597,#21598,#21599));
#6141=EDGE_LOOP('',(#21600,#21601,#21602,#21603));
#6142=EDGE_LOOP('',(#21604,#21605,#21606,#21607,#21608,#21609));
#6143=EDGE_LOOP('',(#21610));
#6144=EDGE_LOOP('',(#21611,#21612,#21613,#21614,#21615,#21616));
#6145=EDGE_LOOP('',(#21617));
#6146=EDGE_LOOP('',(#21618,#21619,#21620,#21621,#21622,#21623));
#6147=EDGE_LOOP('',(#21624));
#6148=EDGE_LOOP('',(#21625,#21626,#21627,#21628,#21629,#21630));
#6149=EDGE_LOOP('',(#21631));
#6150=EDGE_LOOP('',(#21632,#21633,#21634,#21635));
#6151=EDGE_LOOP('',(#21636,#21637,#21638,#21639));
#6152=EDGE_LOOP('',(#21640,#21641,#21642,#21643));
#6153=EDGE_LOOP('',(#21644,#21645,#21646,#21647));
#6154=EDGE_LOOP('',(#21648,#21649,#21650,#21651));
#6155=EDGE_LOOP('',(#21652,#21653,#21654,#21655));
#6156=EDGE_LOOP('',(#21656,#21657,#21658,#21659,#21660,#21661,#21662,#21663,
#21664,#21665,#21666,#21667,#21668,#21669,#21670,#21671,#21672,#21673,#21674,
#21675,#21676));
#6157=EDGE_LOOP('',(#21677,#21678,#21679,#21680,#21681));
#6158=EDGE_LOOP('',(#21682,#21683,#21684,#21685));
#6159=EDGE_LOOP('',(#21686,#21687,#21688,#21689));
#6160=EDGE_LOOP('',(#21690,#21691,#21692,#21693));
#6161=EDGE_LOOP('',(#21694,#21695,#21696,#21697));
#6162=EDGE_LOOP('',(#21698,#21699,#21700,#21701));
#6163=EDGE_LOOP('',(#21702,#21703,#21704));
#6164=EDGE_LOOP('',(#21705,#21706,#21707,#21708));
#6165=EDGE_LOOP('',(#21709,#21710,#21711));
#6166=EDGE_LOOP('',(#21712,#21713,#21714,#21715));
#6167=EDGE_LOOP('',(#21716,#21717,#21718,#21719));
#6168=EDGE_LOOP('',(#21720,#21721,#21722,#21723));
#6169=EDGE_LOOP('',(#21724,#21725,#21726,#21727,#21728,#21729,#21730,#21731));
#6170=EDGE_LOOP('',(#21732,#21733,#21734,#21735));
#6171=EDGE_LOOP('',(#21736,#21737,#21738,#21739));
#6172=EDGE_LOOP('',(#21740,#21741,#21742,#21743));
#6173=EDGE_LOOP('',(#21744,#21745,#21746,#21747,#21748,#21749,#21750,#21751));
#6174=EDGE_LOOP('',(#21752,#21753,#21754,#21755));
#6175=EDGE_LOOP('',(#21756,#21757,#21758,#21759));
#6176=EDGE_LOOP('',(#21760,#21761,#21762));
#6177=EDGE_LOOP('',(#21763,#21764,#21765,#21766));
#6178=EDGE_LOOP('',(#21767,#21768,#21769,#21770));
#6179=EDGE_LOOP('',(#21771,#21772,#21773));
#6180=EDGE_LOOP('',(#21774,#21775,#21776,#21777));
#6181=EDGE_LOOP('',(#21778,#21779,#21780,#21781));
#6182=EDGE_LOOP('',(#21782,#21783,#21784,#21785));
#6183=EDGE_LOOP('',(#21786,#21787,#21788,#21789));
#6184=EDGE_LOOP('',(#21790,#21791,#21792));
#6185=EDGE_LOOP('',(#21793,#21794,#21795,#21796));
#6186=EDGE_LOOP('',(#21797,#21798,#21799,#21800));
#6187=EDGE_LOOP('',(#21801,#21802,#21803,#21804));
#6188=EDGE_LOOP('',(#21805,#21806,#21807,#21808));
#6189=EDGE_LOOP('',(#21809,#21810,#21811));
#6190=EDGE_LOOP('',(#21812,#21813,#21814,#21815));
#6191=EDGE_LOOP('',(#21816,#21817,#21818,#21819));
#6192=EDGE_LOOP('',(#21820,#21821,#21822));
#6193=EDGE_LOOP('',(#21823,#21824,#21825,#21826));
#6194=EDGE_LOOP('',(#21827,#21828,#21829,#21830));
#6195=EDGE_LOOP('',(#21831,#21832,#21833));
#6196=EDGE_LOOP('',(#21834,#21835,#21836,#21837));
#6197=EDGE_LOOP('',(#21838,#21839,#21840,#21841));
#6198=EDGE_LOOP('',(#21842,#21843,#21844,#21845));
#6199=EDGE_LOOP('',(#21846,#21847,#21848,#21849));
#6200=EDGE_LOOP('',(#21850,#21851,#21852,#21853));
#6201=EDGE_LOOP('',(#21854,#21855,#21856));
#6202=EDGE_LOOP('',(#21857,#21858,#21859,#21860));
#6203=EDGE_LOOP('',(#21861,#21862,#21863,#21864));
#6204=EDGE_LOOP('',(#21865,#21866,#21867,#21868,#21869,#21870,#21871,#21872));
#6205=EDGE_LOOP('',(#21873,#21874,#21875,#21876));
#6206=EDGE_LOOP('',(#21877,#21878,#21879,#21880));
#6207=EDGE_LOOP('',(#21881,#21882,#21883,#21884));
#6208=EDGE_LOOP('',(#21885,#21886,#21887,#21888,#21889,#21890,#21891,#21892));
#6209=EDGE_LOOP('',(#21893,#21894,#21895,#21896));
#6210=EDGE_LOOP('',(#21897,#21898,#21899));
#6211=EDGE_LOOP('',(#21900,#21901,#21902,#21903));
#6212=EDGE_LOOP('',(#21904,#21905,#21906,#21907));
#6213=EDGE_LOOP('',(#21908,#21909,#21910,#21911));
#6214=EDGE_LOOP('',(#21912,#21913,#21914,#21915));
#6215=EDGE_LOOP('',(#21916,#21917,#21918,#21919));
#6216=EDGE_LOOP('',(#21920,#21921,#21922));
#6217=EDGE_LOOP('',(#21923,#21924,#21925,#21926));
#6218=EDGE_LOOP('',(#21927,#21928,#21929,#21930));
#6219=EDGE_LOOP('',(#21931,#21932,#21933,#21934));
#6220=EDGE_LOOP('',(#21935,#21936,#21937));
#6221=EDGE_LOOP('',(#21938,#21939,#21940));
#6222=EDGE_LOOP('',(#21941,#21942,#21943,#21944));
#6223=EDGE_LOOP('',(#21945,#21946,#21947,#21948));
#6224=EDGE_LOOP('',(#21949,#21950,#21951,#21952));
#6225=EDGE_LOOP('',(#21953,#21954,#21955,#21956));
#6226=EDGE_LOOP('',(#21957,#21958,#21959,#21960));
#6227=EDGE_LOOP('',(#21961,#21962,#21963));
#6228=EDGE_LOOP('',(#21964,#21965,#21966,#21967));
#6229=EDGE_LOOP('',(#21968,#21969,#21970,#21971));
#6230=EDGE_LOOP('',(#21972,#21973,#21974,#21975));
#6231=EDGE_LOOP('',(#21976,#21977,#21978,#21979));
#6232=EDGE_LOOP('',(#21980,#21981,#21982));
#6233=EDGE_LOOP('',(#21983,#21984,#21985,#21986));
#6234=EDGE_LOOP('',(#21987,#21988,#21989));
#6235=EDGE_LOOP('',(#21990,#21991,#21992,#21993));
#6236=EDGE_LOOP('',(#21994,#21995,#21996,#21997,#21998));
#6237=EDGE_LOOP('',(#21999));
#6238=EDGE_LOOP('',(#22000));
#6239=EDGE_LOOP('',(#22001,#22002,#22003,#22004,#22005));
#6240=EDGE_LOOP('',(#22006,#22007,#22008,#22009,#22010));
#6241=EDGE_LOOP('',(#22011));
#6242=EDGE_LOOP('',(#22012));
#6243=EDGE_LOOP('',(#22013,#22014,#22015,#22016));
#6244=EDGE_LOOP('',(#22017));
#6245=EDGE_LOOP('',(#22018));
#6246=EDGE_LOOP('',(#22019,#22020,#22021,#22022));
#6247=EDGE_LOOP('',(#22023));
#6248=EDGE_LOOP('',(#22024));
#6249=EDGE_LOOP('',(#22025,#22026,#22027,#22028));
#6250=EDGE_LOOP('',(#22029));
#6251=EDGE_LOOP('',(#22030));
#6252=EDGE_LOOP('',(#22031,#22032,#22033,#22034));
#6253=EDGE_LOOP('',(#22035));
#6254=EDGE_LOOP('',(#22036));
#6255=EDGE_LOOP('',(#22037,#22038,#22039,#22040));
#6256=EDGE_LOOP('',(#22041));
#6257=EDGE_LOOP('',(#22042));
#6258=EDGE_LOOP('',(#22043,#22044,#22045,#22046));
#6259=EDGE_LOOP('',(#22047,#22048,#22049,#22050,#22051,#22052,#22053,#22054));
#6260=EDGE_LOOP('',(#22055));
#6261=EDGE_LOOP('',(#22056,#22057,#22058,#22059));
#6262=EDGE_LOOP('',(#22060,#22061,#22062,#22063));
#6263=EDGE_LOOP('',(#22064,#22065,#22066,#22067));
#6264=EDGE_LOOP('',(#22068,#22069,#22070,#22071));
#6265=EDGE_LOOP('',(#22072,#22073,#22074,#22075));
#6266=EDGE_LOOP('',(#22076,#22077,#22078,#22079));
#6267=EDGE_LOOP('',(#22080,#22081,#22082,#22083));
#6268=EDGE_LOOP('',(#22084,#22085,#22086,#22087));
#6269=EDGE_LOOP('',(#22088,#22089,#22090,#22091,#22092));
#6270=EDGE_LOOP('',(#22093,#22094,#22095,#22096,#22097,#22098));
#6271=EDGE_LOOP('',(#22099));
#6272=EDGE_LOOP('',(#22100));
#6273=EDGE_LOOP('',(#22101,#22102,#22103,#22104,#22105));
#6274=EDGE_LOOP('',(#22106));
#6275=EDGE_LOOP('',(#22107,#22108,#22109,#22110,#22111));
#6276=EDGE_LOOP('',(#22112));
#6277=EDGE_LOOP('',(#22113,#22114,#22115,#22116,#22117,#22118));
#6278=EDGE_LOOP('',(#22119,#22120,#22121,#22122,#22123));
#6279=EDGE_LOOP('',(#22124,#22125,#22126,#22127));
#6280=EDGE_LOOP('',(#22128,#22129,#22130,#22131));
#6281=EDGE_LOOP('',(#22132,#22133,#22134,#22135));
#6282=EDGE_LOOP('',(#22136,#22137,#22138,#22139));
#6283=EDGE_LOOP('',(#22140,#22141,#22142,#22143,#22144));
#6284=EDGE_LOOP('',(#22145,#22146,#22147,#22148));
#6285=EDGE_LOOP('',(#22149,#22150,#22151,#22152,#22153,#22154,#22155,#22156,
#22157));
#6286=EDGE_LOOP('',(#22158,#22159,#22160,#22161,#22162));
#6287=EDGE_LOOP('',(#22163,#22164,#22165,#22166,#22167,#22168));
#6288=EDGE_LOOP('',(#22169));
#6289=EDGE_LOOP('',(#22170));
#6290=EDGE_LOOP('',(#22171,#22172,#22173,#22174,#22175));
#6291=EDGE_LOOP('',(#22176));
#6292=EDGE_LOOP('',(#22177,#22178,#22179,#22180,#22181));
#6293=EDGE_LOOP('',(#22182));
#6294=EDGE_LOOP('',(#22183,#22184,#22185,#22186,#22187,#22188));
#6295=EDGE_LOOP('',(#22189,#22190,#22191,#22192,#22193));
#6296=EDGE_LOOP('',(#22194,#22195,#22196,#22197));
#6297=EDGE_LOOP('',(#22198,#22199,#22200,#22201));
#6298=EDGE_LOOP('',(#22202,#22203,#22204,#22205));
#6299=EDGE_LOOP('',(#22206,#22207,#22208,#22209));
#6300=EDGE_LOOP('',(#22210,#22211,#22212,#22213,#22214));
#6301=EDGE_LOOP('',(#22215,#22216,#22217,#22218));
#6302=EDGE_LOOP('',(#22219,#22220,#22221,#22222,#22223,#22224,#22225,#22226,
#22227));
#6303=EDGE_LOOP('',(#22228,#22229,#22230,#22231,#22232));
#6304=EDGE_LOOP('',(#22233,#22234,#22235,#22236,#22237,#22238));
#6305=EDGE_LOOP('',(#22239));
#6306=EDGE_LOOP('',(#22240));
#6307=EDGE_LOOP('',(#22241,#22242,#22243,#22244,#22245));
#6308=EDGE_LOOP('',(#22246));
#6309=EDGE_LOOP('',(#22247,#22248,#22249,#22250,#22251));
#6310=EDGE_LOOP('',(#22252));
#6311=EDGE_LOOP('',(#22253,#22254,#22255,#22256,#22257,#22258));
#6312=EDGE_LOOP('',(#22259,#22260,#22261,#22262,#22263));
#6313=EDGE_LOOP('',(#22264,#22265,#22266,#22267));
#6314=EDGE_LOOP('',(#22268,#22269,#22270,#22271));
#6315=EDGE_LOOP('',(#22272,#22273,#22274,#22275));
#6316=EDGE_LOOP('',(#22276,#22277,#22278,#22279));
#6317=EDGE_LOOP('',(#22280,#22281,#22282,#22283,#22284));
#6318=EDGE_LOOP('',(#22285,#22286,#22287,#22288));
#6319=EDGE_LOOP('',(#22289,#22290,#22291,#22292,#22293,#22294,#22295,#22296,
#22297));
#6320=EDGE_LOOP('',(#22298,#22299,#22300,#22301,#22302));
#6321=EDGE_LOOP('',(#22303,#22304,#22305,#22306,#22307,#22308));
#6322=EDGE_LOOP('',(#22309));
#6323=EDGE_LOOP('',(#22310));
#6324=EDGE_LOOP('',(#22311,#22312,#22313,#22314,#22315));
#6325=EDGE_LOOP('',(#22316));
#6326=EDGE_LOOP('',(#22317,#22318,#22319));
#6327=EDGE_LOOP('',(#22320,#22321,#22322));
#6328=EDGE_LOOP('',(#22323,#22324,#22325));
#6329=EDGE_LOOP('',(#22326,#22327,#22328));
#6330=EDGE_LOOP('',(#22329,#22330,#22331));
#6331=EDGE_LOOP('',(#22332,#22333,#22334));
#6332=EDGE_LOOP('',(#22335,#22336,#22337,#22338,#22339));
#6333=EDGE_LOOP('',(#22340,#22341,#22342,#22343,#22344));
#6334=EDGE_LOOP('',(#22345,#22346,#22347,#22348,#22349));
#6335=EDGE_LOOP('',(#22350,#22351,#22352,#22353,#22354,#22355));
#6336=EDGE_LOOP('',(#22356));
#6337=EDGE_LOOP('',(#22357,#22358,#22359,#22360,#22361));
#6338=EDGE_LOOP('',(#22362,#22363,#22364,#22365,#22366));
#6339=EDGE_LOOP('',(#22367,#22368,#22369,#22370,#22371));
#6340=EDGE_LOOP('',(#22372,#22373,#22374,#22375,#22376,#22377));
#6341=EDGE_LOOP('',(#22378,#22379,#22380,#22381));
#6342=EDGE_LOOP('',(#22382,#22383,#22384,#22385));
#6343=EDGE_LOOP('',(#22386,#22387,#22388,#22389));
#6344=EDGE_LOOP('',(#22390,#22391,#22392,#22393));
#6345=EDGE_LOOP('',(#22394,#22395,#22396,#22397));
#6346=EDGE_LOOP('',(#22398,#22399,#22400,#22401));
#6347=EDGE_LOOP('',(#22402,#22403,#22404,#22405));
#6348=EDGE_LOOP('',(#22406,#22407,#22408,#22409));
#6349=EDGE_LOOP('',(#22410,#22411,#22412,#22413));
#6350=EDGE_LOOP('',(#22414,#22415,#22416,#22417));
#6351=EDGE_LOOP('',(#22418,#22419,#22420,#22421));
#6352=EDGE_LOOP('',(#22422,#22423,#22424,#22425));
#6353=EDGE_LOOP('',(#22426,#22427,#22428,#22429));
#6354=EDGE_LOOP('',(#22430,#22431,#22432,#22433));
#6355=EDGE_LOOP('',(#22434,#22435,#22436,#22437));
#6356=EDGE_LOOP('',(#22438,#22439,#22440,#22441));
#6357=EDGE_LOOP('',(#22442,#22443,#22444,#22445));
#6358=EDGE_LOOP('',(#22446,#22447,#22448,#22449));
#6359=EDGE_LOOP('',(#22450,#22451,#22452,#22453));
#6360=EDGE_LOOP('',(#22454,#22455,#22456,#22457));
#6361=EDGE_LOOP('',(#22458,#22459,#22460,#22461));
#6362=EDGE_LOOP('',(#22462,#22463,#22464,#22465));
#6363=EDGE_LOOP('',(#22466,#22467,#22468,#22469));
#6364=EDGE_LOOP('',(#22470,#22471,#22472,#22473));
#6365=EDGE_LOOP('',(#22474,#22475,#22476,#22477));
#6366=EDGE_LOOP('',(#22478,#22479,#22480,#22481));
#6367=EDGE_LOOP('',(#22482));
#6368=EDGE_LOOP('',(#22483));
#6369=EDGE_LOOP('',(#22484));
#6370=EDGE_LOOP('',(#22485));
#6371=EDGE_LOOP('',(#22486));
#6372=EDGE_LOOP('',(#22487));
#6373=EDGE_LOOP('',(#22488,#22489,#22490,#22491));
#6374=EDGE_LOOP('',(#22492,#22493,#22494,#22495));
#6375=EDGE_LOOP('',(#22496,#22497,#22498,#22499));
#6376=EDGE_LOOP('',(#22500,#22501,#22502,#22503));
#6377=EDGE_LOOP('',(#22504,#22505,#22506,#22507));
#6378=EDGE_LOOP('',(#22508,#22509,#22510,#22511));
#6379=EDGE_LOOP('',(#22512,#22513,#22514,#22515,#22516,#22517));
#6380=EDGE_LOOP('',(#22518,#22519,#22520,#22521));
#6381=EDGE_LOOP('',(#22522,#22523,#22524,#22525));
#6382=EDGE_LOOP('',(#22526,#22527,#22528,#22529));
#6383=EDGE_LOOP('',(#22530,#22531,#22532,#22533));
#6384=EDGE_LOOP('',(#22534,#22535,#22536,#22537));
#6385=EDGE_LOOP('',(#22538,#22539,#22540,#22541));
#6386=EDGE_LOOP('',(#22542,#22543,#22544,#22545,#22546,#22547,#22548,#22549));
#6387=EDGE_LOOP('',(#22550,#22551,#22552,#22553,#22554,#22555,#22556,#22557));
#6388=EDGE_LOOP('',(#22558,#22559,#22560,#22561));
#6389=EDGE_LOOP('',(#22562));
#6390=EDGE_LOOP('',(#22563));
#6391=EDGE_LOOP('',(#22564));
#6392=EDGE_LOOP('',(#22565));
#6393=EDGE_LOOP('',(#22566));
#6394=EDGE_LOOP('',(#22567));
#6395=EDGE_LOOP('',(#22568,#22569,#22570,#22571));
#6396=EDGE_LOOP('',(#22572,#22573,#22574,#22575));
#6397=EDGE_LOOP('',(#22576,#22577,#22578,#22579));
#6398=EDGE_LOOP('',(#22580,#22581,#22582,#22583));
#6399=EDGE_LOOP('',(#22584,#22585,#22586,#22587));
#6400=EDGE_LOOP('',(#22588,#22589,#22590,#22591));
#6401=EDGE_LOOP('',(#22592,#22593,#22594,#22595,#22596,#22597));
#6402=EDGE_LOOP('',(#22598,#22599,#22600,#22601,#22602,#22603,#22604,#22605,
#22606,#22607,#22608,#22609,#22610,#22611,#22612,#22613,#22614));
#6403=EDGE_LOOP('',(#22615,#22616,#22617,#22618));
#6404=EDGE_LOOP('',(#22619,#22620,#22621,#22622));
#6405=EDGE_LOOP('',(#22623,#22624,#22625,#22626));
#6406=EDGE_LOOP('',(#22627,#22628));
#6407=EDGE_LOOP('',(#22629,#22630,#22631,#22632,#22633,#22634,#22635));
#6408=EDGE_LOOP('',(#22636,#22637,#22638,#22639,#22640,#22641,#22642,#22643,
#22644,#22645));
#6409=EDGE_LOOP('',(#22646,#22647,#22648));
#6410=EDGE_LOOP('',(#22649,#22650,#22651));
#6411=EDGE_LOOP('',(#22652,#22653,#22654,#22655));
#6412=EDGE_LOOP('',(#22656,#22657,#22658,#22659));
#6413=EDGE_LOOP('',(#22660,#22661,#22662,#22663));
#6414=EDGE_LOOP('',(#22664,#22665,#22666,#22667));
#6415=EDGE_LOOP('',(#22668,#22669,#22670,#22671));
#6416=EDGE_LOOP('',(#22672,#22673,#22674,#22675,#22676,#22677));
#6417=EDGE_LOOP('',(#22678,#22679,#22680,#22681,#22682,#22683,#22684,#22685,
#22686,#22687));
#6418=EDGE_LOOP('',(#22688,#22689,#22690));
#6419=EDGE_LOOP('',(#22691,#22692,#22693));
#6420=EDGE_LOOP('',(#22694,#22695));
#6421=EDGE_LOOP('',(#22696));
#6422=EDGE_LOOP('',(#22697,#22698,#22699,#22700,#22701,#22702,#22703,#22704,
#22705,#22706,#22707,#22708));
#6423=EDGE_LOOP('',(#22709,#22710,#22711,#22712));
#6424=EDGE_LOOP('',(#22713,#22714,#22715,#22716));
#6425=EDGE_LOOP('',(#22717,#22718));
#6426=EDGE_LOOP('',(#22719,#22720,#22721,#22722,#22723,#22724));
#6427=EDGE_LOOP('',(#22725,#22726,#22727,#22728,#22729,#22730));
#6428=EDGE_LOOP('',(#22731,#22732,#22733,#22734));
#6429=EDGE_LOOP('',(#22735,#22736,#22737,#22738));
#6430=EDGE_LOOP('',(#22739,#22740,#22741,#22742));
#6431=EDGE_LOOP('',(#22743,#22744,#22745,#22746));
#6432=EDGE_LOOP('',(#22747,#22748,#22749,#22750));
#6433=EDGE_LOOP('',(#22751,#22752,#22753,#22754));
#6434=EDGE_LOOP('',(#22755,#22756,#22757,#22758));
#6435=EDGE_LOOP('',(#22759,#22760,#22761,#22762));
#6436=EDGE_LOOP('',(#22763,#22764,#22765,#22766));
#6437=EDGE_LOOP('',(#22767,#22768,#22769,#22770));
#6438=EDGE_LOOP('',(#22771,#22772,#22773,#22774));
#6439=EDGE_LOOP('',(#22775,#22776,#22777,#22778));
#6440=EDGE_LOOP('',(#22779,#22780,#22781,#22782,#22783,#22784,#22785,#22786,
#22787,#22788,#22789,#22790));
#6441=EDGE_LOOP('',(#22791));
#6442=EDGE_LOOP('',(#22792,#22793,#22794,#22795,#22796,#22797,#22798,#22799,
#22800,#22801,#22802,#22803));
#6443=EDGE_LOOP('',(#22804,#22805));
#6444=EDGE_LOOP('',(#22806,#22807,#22808,#22809));
#6445=EDGE_LOOP('',(#22810,#22811,#22812,#22813));
#6446=EDGE_LOOP('',(#22814,#22815,#22816,#22817));
#6447=EDGE_LOOP('',(#22818,#22819,#22820,#22821));
#6448=EDGE_LOOP('',(#22822,#22823,#22824,#22825));
#6449=EDGE_LOOP('',(#22826,#22827,#22828,#22829));
#6450=EDGE_LOOP('',(#22830,#22831,#22832,#22833));
#6451=EDGE_LOOP('',(#22834,#22835,#22836,#22837));
#6452=EDGE_LOOP('',(#22838,#22839,#22840,#22841));
#6453=EDGE_LOOP('',(#22842,#22843,#22844,#22845,#22846,#22847,#22848,#22849));
#6454=EDGE_LOOP('',(#22850,#22851,#22852,#22853));
#6455=EDGE_LOOP('',(#22854,#22855,#22856,#22857,#22858,#22859,#22860,#22861));
#6456=EDGE_LOOP('',(#22862));
#6457=EDGE_LOOP('',(#22863));
#6458=EDGE_LOOP('',(#22864,#22865,#22866,#22867,#22868,#22869,#22870,#22871));
#6459=EDGE_LOOP('',(#22872,#22873,#22874,#22875));
#6460=EDGE_LOOP('',(#22876,#22877,#22878,#22879));
#6461=EDGE_LOOP('',(#22880,#22881,#22882,#22883));
#6462=EDGE_LOOP('',(#22884,#22885,#22886,#22887));
#6463=EDGE_LOOP('',(#22888,#22889,#22890,#22891));
#6464=EDGE_LOOP('',(#22892,#22893,#22894,#22895));
#6465=EDGE_LOOP('',(#22896,#22897,#22898,#22899));
#6466=EDGE_LOOP('',(#22900,#22901,#22902,#22903));
#6467=EDGE_LOOP('',(#22904,#22905,#22906,#22907,#22908,#22909,#22910,#22911));
#6468=EDGE_LOOP('',(#22912));
#6469=EDGE_LOOP('',(#22913,#22914,#22915,#22916,#22917,#22918,#22919,#22920,
#22921,#22922,#22923,#22924));
#6470=EDGE_LOOP('',(#22925,#22926,#22927,#22928));
#6471=EDGE_LOOP('',(#22929));
#6472=EDGE_LOOP('',(#22930,#22931,#22932,#22933,#22934,#22935,#22936,#22937,
#22938,#22939,#22940,#22941));
#6473=EDGE_LOOP('',(#22942,#22943,#22944,#22945));
#6474=EDGE_LOOP('',(#22946,#22947,#22948,#22949));
#6475=EDGE_LOOP('',(#22950,#22951,#22952,#22953));
#6476=EDGE_LOOP('',(#22954,#22955,#22956,#22957));
#6477=EDGE_LOOP('',(#22958,#22959,#22960,#22961));
#6478=EDGE_LOOP('',(#22962,#22963,#22964,#22965));
#6479=EDGE_LOOP('',(#22966,#22967,#22968,#22969));
#6480=EDGE_LOOP('',(#22970,#22971,#22972,#22973));
#6481=EDGE_LOOP('',(#22974,#22975,#22976,#22977));
#6482=EDGE_LOOP('',(#22978,#22979,#22980,#22981));
#6483=EDGE_LOOP('',(#22982,#22983,#22984,#22985));
#6484=EDGE_LOOP('',(#22986,#22987,#22988,#22989));
#6485=EDGE_LOOP('',(#22990,#22991,#22992,#22993));
#6486=EDGE_LOOP('',(#22994,#22995,#22996,#22997,#22998,#22999,#23000,#23001,
#23002,#23003,#23004,#23005));
#6487=EDGE_LOOP('',(#23006,#23007,#23008,#23009));
#6488=EDGE_LOOP('',(#23010,#23011,#23012,#23013));
#6489=EDGE_LOOP('',(#23014,#23015,#23016,#23017));
#6490=EDGE_LOOP('',(#23018,#23019,#23020,#23021));
#6491=EDGE_LOOP('',(#23022,#23023,#23024,#23025));
#6492=EDGE_LOOP('',(#23026,#23027,#23028,#23029));
#6493=EDGE_LOOP('',(#23030,#23031,#23032,#23033));
#6494=EDGE_LOOP('',(#23034,#23035,#23036,#23037));
#6495=EDGE_LOOP('',(#23038,#23039,#23040,#23041));
#6496=EDGE_LOOP('',(#23042,#23043,#23044,#23045));
#6497=EDGE_LOOP('',(#23046,#23047,#23048,#23049));
#6498=EDGE_LOOP('',(#23050,#23051,#23052,#23053));
#6499=EDGE_LOOP('',(#23054,#23055,#23056,#23057,#23058,#23059,#23060,#23061,
#23062,#23063,#23064,#23065));
#6500=EDGE_LOOP('',(#23066,#23067,#23068,#23069,#23070,#23071,#23072,#23073,
#23074,#23075,#23076,#23077));
#6501=EDGE_LOOP('',(#23078,#23079,#23080,#23081));
#6502=EDGE_LOOP('',(#23082,#23083,#23084,#23085));
#6503=EDGE_LOOP('',(#23086,#23087,#23088,#23089));
#6504=EDGE_LOOP('',(#23090,#23091,#23092,#23093));
#6505=EDGE_LOOP('',(#23094,#23095,#23096,#23097));
#6506=EDGE_LOOP('',(#23098,#23099,#23100,#23101));
#6507=EDGE_LOOP('',(#23102,#23103,#23104,#23105));
#6508=EDGE_LOOP('',(#23106,#23107,#23108,#23109,#23110));
#6509=EDGE_LOOP('',(#23111,#23112,#23113,#23114));
#6510=EDGE_LOOP('',(#23115,#23116,#23117,#23118));
#6511=EDGE_LOOP('',(#23119,#23120,#23121,#23122));
#6512=EDGE_LOOP('',(#23123,#23124,#23125,#23126));
#6513=EDGE_LOOP('',(#23127,#23128,#23129,#23130));
#6514=EDGE_LOOP('',(#23131,#23132,#23133,#23134));
#6515=EDGE_LOOP('',(#23135,#23136,#23137,#23138,#23139,#23140,#23141,#23142));
#6516=EDGE_LOOP('',(#23143,#23144,#23145,#23146,#23147,#23148,#23149,#23150));
#6517=EDGE_LOOP('',(#23151,#23152,#23153,#23154));
#6518=EDGE_LOOP('',(#23155,#23156,#23157,#23158));
#6519=EDGE_LOOP('',(#23159,#23160,#23161,#23162));
#6520=EDGE_LOOP('',(#23163,#23164,#23165,#23166));
#6521=EDGE_LOOP('',(#23167));
#6522=EDGE_LOOP('',(#23168,#23169,#23170,#23171));
#6523=EDGE_LOOP('',(#23172,#23173,#23174,#23175));
#6524=EDGE_LOOP('',(#23176,#23177,#23178,#23179));
#6525=EDGE_LOOP('',(#23180,#23181,#23182,#23183));
#6526=EDGE_LOOP('',(#23184,#23185,#23186,#23187));
#6527=EDGE_LOOP('',(#23188,#23189,#23190,#23191));
#6528=EDGE_LOOP('',(#23192,#23193,#23194,#23195));
#6529=EDGE_LOOP('',(#23196,#23197,#23198,#23199));
#6530=EDGE_LOOP('',(#23200,#23201,#23202,#23203));
#6531=EDGE_LOOP('',(#23204,#23205,#23206,#23207));
#6532=EDGE_LOOP('',(#23208,#23209,#23210,#23211));
#6533=EDGE_LOOP('',(#23212,#23213,#23214,#23215));
#6534=EDGE_LOOP('',(#23216,#23217,#23218,#23219));
#6535=EDGE_LOOP('',(#23220));
#6536=EDGE_LOOP('',(#23221,#23222,#23223,#23224,#23225,#23226,#23227,#23228,
#23229,#23230,#23231,#23232));
#6537=EDGE_LOOP('',(#23233,#23234,#23235,#23236));
#6538=EDGE_LOOP('',(#23237));
#6539=EDGE_LOOP('',(#23238,#23239,#23240,#23241,#23242,#23243,#23244,#23245,
#23246,#23247,#23248,#23249));
#6540=EDGE_LOOP('',(#23250,#23251,#23252,#23253,#23254,#23255,#23256,#23257,
#23258,#23259,#23260,#23261));
#6541=EDGE_LOOP('',(#23262,#23263,#23264,#23265));
#6542=EDGE_LOOP('',(#23266,#23267,#23268,#23269));
#6543=EDGE_LOOP('',(#23270,#23271,#23272,#23273));
#6544=EDGE_LOOP('',(#23274,#23275,#23276,#23277));
#6545=EDGE_LOOP('',(#23278,#23279,#23280,#23281));
#6546=EDGE_LOOP('',(#23282,#23283,#23284,#23285));
#6547=EDGE_LOOP('',(#23286,#23287,#23288,#23289));
#6548=EDGE_LOOP('',(#23290,#23291,#23292,#23293));
#6549=EDGE_LOOP('',(#23294,#23295,#23296,#23297));
#6550=EDGE_LOOP('',(#23298,#23299,#23300,#23301));
#6551=EDGE_LOOP('',(#23302));
#6552=EDGE_LOOP('',(#23303));
#6553=EDGE_LOOP('',(#23304,#23305,#23306,#23307,#23308,#23309));
#6554=EDGE_LOOP('',(#23310,#23311));
#6555=EDGE_LOOP('',(#23312,#23313,#23314,#23315,#23316,#23317));
#6556=EDGE_LOOP('',(#23318,#23319,#23320));
#6557=EDGE_LOOP('',(#23321,#23322,#23323,#23324,#23325));
#6558=EDGE_LOOP('',(#23326,#23327,#23328,#23329,#23330,#23331));
#6559=EDGE_LOOP('',(#23332,#23333));
#6560=EDGE_LOOP('',(#23334,#23335,#23336,#23337,#23338,#23339));
#6561=EDGE_LOOP('',(#23340,#23341,#23342,#23343,#23344,#23345));
#6562=EDGE_LOOP('',(#23346,#23347,#23348,#23349,#23350));
#6563=EDGE_LOOP('',(#23351,#23352,#23353,#23354,#23355));
#6564=EDGE_LOOP('',(#23356,#23357));
#6565=EDGE_LOOP('',(#23358,#23359));
#6566=EDGE_LOOP('',(#23360,#23361));
#6567=EDGE_LOOP('',(#23362));
#6568=EDGE_LOOP('',(#23363));
#6569=EDGE_LOOP('',(#23364,#23365,#23366,#23367,#23368));
#6570=EDGE_LOOP('',(#23369,#23370,#23371,#23372,#23373,#23374,#23375,#23376,
#23377,#23378,#23379,#23380,#23381,#23382,#23383,#23384));
#6571=EDGE_LOOP('',(#23385,#23386,#23387,#23388));
#6572=EDGE_LOOP('',(#23389,#23390,#23391,#23392,#23393,#23394,#23395,#23396,
#23397,#23398,#23399,#23400,#23401,#23402,#23403,#23404));
#6573=EDGE_LOOP('',(#23405,#23406,#23407,#23408));
#6574=EDGE_LOOP('',(#23409,#23410,#23411,#23412,#23413,#23414));
#6575=EDGE_LOOP('',(#23415,#23416,#23417,#23418,#23419,#23420));
#6576=EDGE_LOOP('',(#23421,#23422,#23423,#23424));
#6577=EDGE_LOOP('',(#23425,#23426,#23427,#23428));
#6578=EDGE_LOOP('',(#23429,#23430,#23431,#23432));
#6579=EDGE_LOOP('',(#23433,#23434,#23435,#23436));
#6580=EDGE_LOOP('',(#23437,#23438,#23439,#23440));
#6581=EDGE_LOOP('',(#23441,#23442,#23443,#23444));
#6582=EDGE_LOOP('',(#23445,#23446,#23447,#23448));
#6583=EDGE_LOOP('',(#23449,#23450,#23451,#23452));
#6584=EDGE_LOOP('',(#23453,#23454,#23455,#23456));
#6585=EDGE_LOOP('',(#23457,#23458,#23459,#23460));
#6586=EDGE_LOOP('',(#23461,#23462,#23463,#23464));
#6587=EDGE_LOOP('',(#23465,#23466,#23467,#23468));
#6588=EDGE_LOOP('',(#23469));
#6589=EDGE_LOOP('',(#23470,#23471,#23472,#23473,#23474));
#6590=EDGE_LOOP('',(#23475,#23476,#23477,#23478,#23479));
#6591=EDGE_LOOP('',(#23480));
#6592=EDGE_LOOP('',(#23481,#23482,#23483,#23484,#23485));
#6593=EDGE_LOOP('',(#23486,#23487,#23488,#23489,#23490));
#6594=EDGE_LOOP('',(#23491));
#6595=EDGE_LOOP('',(#23492,#23493,#23494,#23495,#23496));
#6596=EDGE_LOOP('',(#23497,#23498,#23499,#23500,#23501));
#6597=EDGE_LOOP('',(#23502));
#6598=EDGE_LOOP('',(#23503,#23504,#23505,#23506,#23507));
#6599=EDGE_LOOP('',(#23508,#23509,#23510,#23511,#23512));
#6600=EDGE_LOOP('',(#23513,#23514,#23515,#23516,#23517));
#6601=EDGE_LOOP('',(#23518));
#6602=EDGE_LOOP('',(#23519));
#6603=EDGE_LOOP('',(#23520));
#6604=EDGE_LOOP('',(#23521));
#6605=EDGE_LOOP('',(#23522));
#6606=EDGE_LOOP('',(#23523));
#6607=EDGE_LOOP('',(#23524));
#6608=EDGE_LOOP('',(#23525));
#6609=EDGE_LOOP('',(#23526));
#6610=EDGE_LOOP('',(#23527));
#6611=EDGE_LOOP('',(#23528,#23529,#23530,#23531));
#6612=EDGE_LOOP('',(#23532));
#6613=EDGE_LOOP('',(#23533));
#6614=EDGE_LOOP('',(#23534,#23535,#23536,#23537));
#6615=EDGE_LOOP('',(#23538));
#6616=EDGE_LOOP('',(#23539,#23540,#23541,#23542));
#6617=EDGE_LOOP('',(#23543,#23544,#23545,#23546));
#6618=EDGE_LOOP('',(#23547));
#6619=EDGE_LOOP('',(#23548,#23549,#23550,#23551));
#6620=EDGE_LOOP('',(#23552));
#6621=EDGE_LOOP('',(#23553));
#6622=EDGE_LOOP('',(#23554,#23555,#23556,#23557));
#6623=EDGE_LOOP('',(#23558));
#6624=EDGE_LOOP('',(#23559));
#6625=EDGE_LOOP('',(#23560,#23561,#23562,#23563));
#6626=EDGE_LOOP('',(#23564,#23565,#23566,#23567));
#6627=EDGE_LOOP('',(#23568));
#6628=EDGE_LOOP('',(#23569,#23570,#23571,#23572));
#6629=EDGE_LOOP('',(#23573));
#6630=EDGE_LOOP('',(#23574));
#6631=EDGE_LOOP('',(#23575,#23576,#23577,#23578));
#6632=EDGE_LOOP('',(#23579));
#6633=EDGE_LOOP('',(#23580));
#6634=EDGE_LOOP('',(#23581,#23582,#23583,#23584));
#6635=EDGE_LOOP('',(#23585));
#6636=EDGE_LOOP('',(#23586));
#6637=EDGE_LOOP('',(#23587,#23588,#23589,#23590));
#6638=EDGE_LOOP('',(#23591,#23592,#23593,#23594));
#6639=EDGE_LOOP('',(#23595));
#6640=EDGE_LOOP('',(#23596));
#6641=EDGE_LOOP('',(#23597,#23598,#23599,#23600));
#6642=EDGE_LOOP('',(#23601));
#6643=EDGE_LOOP('',(#23602,#23603,#23604,#23605,#23606,#23607));
#6644=EDGE_LOOP('',(#23608,#23609,#23610,#23611));
#6645=EDGE_LOOP('',(#23612,#23613,#23614,#23615,#23616,#23617));
#6646=EDGE_LOOP('',(#23618,#23619,#23620,#23621));
#6647=EDGE_LOOP('',(#23622));
#6648=EDGE_LOOP('',(#23623,#23624,#23625,#23626));
#6649=EDGE_LOOP('',(#23627,#23628,#23629,#23630));
#6650=EDGE_LOOP('',(#23631,#23632,#23633,#23634));
#6651=EDGE_LOOP('',(#23635,#23636,#23637,#23638));
#6652=EDGE_LOOP('',(#23639));
#6653=EDGE_LOOP('',(#23640,#23641,#23642,#23643));
#6654=EDGE_LOOP('',(#23644,#23645,#23646,#23647));
#6655=EDGE_LOOP('',(#23648,#23649,#23650,#23651));
#6656=EDGE_LOOP('',(#23652));
#6657=EDGE_LOOP('',(#23653,#23654));
#6658=EDGE_LOOP('',(#23655,#23656,#23657,#23658,#23659,#23660,#23661,#23662,
#23663,#23664,#23665,#23666,#23667,#23668,#23669,#23670));
#6659=EDGE_LOOP('',(#23671,#23672,#23673,#23674));
#6660=EDGE_LOOP('',(#23675));
#6661=EDGE_LOOP('',(#23676,#23677,#23678,#23679));
#6662=EDGE_LOOP('',(#23680,#23681,#23682,#23683));
#6663=EDGE_LOOP('',(#23684,#23685));
#6664=EDGE_LOOP('',(#23686,#23687,#23688,#23689,#23690,#23691,#23692,#23693,
#23694,#23695,#23696,#23697,#23698,#23699,#23700,#23701));
#6665=EDGE_LOOP('',(#23702,#23703,#23704,#23705));
#6666=EDGE_LOOP('',(#23706,#23707,#23708,#23709));
#6667=EDGE_LOOP('',(#23710,#23711,#23712,#23713));
#6668=EDGE_LOOP('',(#23714,#23715,#23716,#23717));
#6669=EDGE_LOOP('',(#23718,#23719,#23720,#23721));
#6670=EDGE_LOOP('',(#23722,#23723,#23724,#23725));
#6671=EDGE_LOOP('',(#23726,#23727,#23728,#23729));
#6672=EDGE_LOOP('',(#23730,#23731,#23732,#23733));
#6673=EDGE_LOOP('',(#23734,#23735,#23736,#23737));
#6674=EDGE_LOOP('',(#23738,#23739,#23740,#23741));
#6675=EDGE_LOOP('',(#23742,#23743,#23744,#23745));
#6676=EDGE_LOOP('',(#23746,#23747,#23748,#23749));
#6677=EDGE_LOOP('',(#23750,#23751,#23752,#23753));
#6678=EDGE_LOOP('',(#23754,#23755,#23756,#23757));
#6679=EDGE_LOOP('',(#23758,#23759,#23760,#23761));
#6680=EDGE_LOOP('',(#23762,#23763,#23764,#23765));
#6681=EDGE_LOOP('',(#23766,#23767,#23768,#23769,#23770,#23771,#23772,#23773,
#23774,#23775,#23776,#23777,#23778,#23779,#23780,#23781));
#6682=EDGE_LOOP('',(#23782,#23783,#23784,#23785));
#6683=EDGE_LOOP('',(#23786,#23787,#23788,#23789));
#6684=EDGE_LOOP('',(#23790,#23791,#23792,#23793));
#6685=EDGE_LOOP('',(#23794,#23795,#23796,#23797));
#6686=EDGE_LOOP('',(#23798,#23799,#23800,#23801));
#6687=EDGE_LOOP('',(#23802,#23803,#23804,#23805));
#6688=EDGE_LOOP('',(#23806,#23807,#23808,#23809));
#6689=EDGE_LOOP('',(#23810,#23811,#23812,#23813));
#6690=EDGE_LOOP('',(#23814,#23815,#23816,#23817));
#6691=EDGE_LOOP('',(#23818,#23819,#23820,#23821));
#6692=EDGE_LOOP('',(#23822,#23823,#23824,#23825));
#6693=EDGE_LOOP('',(#23826,#23827,#23828,#23829));
#6694=EDGE_LOOP('',(#23830,#23831,#23832,#23833));
#6695=EDGE_LOOP('',(#23834,#23835,#23836,#23837));
#6696=EDGE_LOOP('',(#23838,#23839,#23840,#23841));
#6697=EDGE_LOOP('',(#23842,#23843,#23844,#23845,#23846,#23847,#23848,#23849,
#23850,#23851,#23852,#23853));
#6698=EDGE_LOOP('',(#23854));
#6699=EDGE_LOOP('',(#23855));
#6700=EDGE_LOOP('',(#23856,#23857,#23858,#23859));
#6701=EDGE_LOOP('',(#23860));
#6702=EDGE_LOOP('',(#23861));
#6703=EDGE_LOOP('',(#23862,#23863,#23864,#23865));
#6704=EDGE_LOOP('',(#23866,#23867,#23868,#23869,#23870,#23871,#23872,#23873,
#23874,#23875,#23876,#23877,#23878,#23879));
#6705=EDGE_LOOP('',(#23880,#23881,#23882,#23883,#23884,#23885));
#6706=EDGE_LOOP('',(#23886,#23887,#23888));
#6707=EDGE_LOOP('',(#23889,#23890,#23891));
#6708=EDGE_LOOP('',(#23892,#23893,#23894,#23895,#23896));
#6709=EDGE_LOOP('',(#23897,#23898,#23899,#23900,#23901,#23902));
#6710=EDGE_LOOP('',(#23903,#23904,#23905,#23906,#23907,#23908,#23909,#23910));
#6711=EDGE_LOOP('',(#23911,#23912,#23913,#23914));
#6712=EDGE_LOOP('',(#23915,#23916,#23917));
#6713=EDGE_LOOP('',(#23918,#23919,#23920));
#6714=EDGE_LOOP('',(#23921,#23922,#23923));
#6715=EDGE_LOOP('',(#23924,#23925,#23926));
#6716=EDGE_LOOP('',(#23927,#23928,#23929));
#6717=EDGE_LOOP('',(#23930,#23931,#23932));
#6718=EDGE_LOOP('',(#23933,#23934,#23935,#23936));
#6719=EDGE_LOOP('',(#23937,#23938,#23939,#23940));
#6720=EDGE_LOOP('',(#23941,#23942,#23943));
#6721=EDGE_LOOP('',(#23944,#23945,#23946));
#6722=EDGE_LOOP('',(#23947,#23948,#23949,#23950));
#6723=EDGE_LOOP('',(#23951,#23952,#23953,#23954));
#6724=EDGE_LOOP('',(#23955,#23956,#23957));
#6725=EDGE_LOOP('',(#23958,#23959,#23960,#23961));
#6726=EDGE_LOOP('',(#23962,#23963,#23964,#23965));
#6727=EDGE_LOOP('',(#23966,#23967,#23968));
#6728=EDGE_LOOP('',(#23969,#23970,#23971,#23972));
#6729=EDGE_LOOP('',(#23973,#23974,#23975,#23976));
#6730=EDGE_LOOP('',(#23977,#23978,#23979,#23980));
#6731=EDGE_LOOP('',(#23981,#23982,#23983,#23984));
#6732=EDGE_LOOP('',(#23985,#23986,#23987,#23988));
#6733=EDGE_LOOP('',(#23989,#23990,#23991,#23992));
#6734=EDGE_LOOP('',(#23993,#23994,#23995,#23996));
#6735=EDGE_LOOP('',(#23997,#23998,#23999,#24000));
#6736=EDGE_LOOP('',(#24001,#24002,#24003,#24004));
#6737=EDGE_LOOP('',(#24005,#24006,#24007,#24008));
#6738=EDGE_LOOP('',(#24009,#24010,#24011,#24012));
#6739=EDGE_LOOP('',(#24013,#24014,#24015,#24016));
#6740=EDGE_LOOP('',(#24017,#24018,#24019,#24020));
#6741=EDGE_LOOP('',(#24021,#24022,#24023,#24024));
#6742=EDGE_LOOP('',(#24025,#24026,#24027,#24028));
#6743=EDGE_LOOP('',(#24029,#24030,#24031,#24032));
#6744=EDGE_LOOP('',(#24033,#24034,#24035,#24036,#24037,#24038,#24039,#24040));
#6745=EDGE_LOOP('',(#24041,#24042,#24043,#24044,#24045));
#6746=EDGE_LOOP('',(#24046,#24047,#24048,#24049,#24050,#24051,#24052,#24053,
#24054,#24055,#24056,#24057,#24058,#24059));
#6747=EDGE_LOOP('',(#24060,#24061,#24062,#24063));
#6748=EDGE_LOOP('',(#24064));
#6749=EDGE_LOOP('',(#24065));
#6750=EDGE_LOOP('',(#24066,#24067,#24068,#24069));
#6751=EDGE_LOOP('',(#24070));
#6752=EDGE_LOOP('',(#24071));
#6753=EDGE_LOOP('',(#24072,#24073,#24074,#24075));
#6754=EDGE_LOOP('',(#24076,#24077,#24078,#24079));
#6755=EDGE_LOOP('',(#24080,#24081,#24082,#24083));
#6756=EDGE_LOOP('',(#24084,#24085,#24086,#24087));
#6757=EDGE_LOOP('',(#24088,#24089,#24090,#24091));
#6758=EDGE_LOOP('',(#24092,#24093,#24094,#24095,#24096));
#6759=EDGE_LOOP('',(#24097,#24098,#24099,#24100));
#6760=EDGE_LOOP('',(#24101,#24102,#24103,#24104,#24105));
#6761=EDGE_LOOP('',(#24106,#24107,#24108,#24109));
#6762=EDGE_LOOP('',(#24110,#24111,#24112,#24113,#24114));
#6763=EDGE_LOOP('',(#24115,#24116,#24117,#24118));
#6764=EDGE_LOOP('',(#24119,#24120,#24121,#24122,#24123));
#6765=EDGE_LOOP('',(#24124,#24125,#24126,#24127,#24128));
#6766=EDGE_LOOP('',(#24129,#24130,#24131,#24132,#24133));
#6767=EDGE_LOOP('',(#24134,#24135,#24136,#24137,#24138));
#6768=EDGE_LOOP('',(#24139,#24140,#24141,#24142,#24143));
#6769=EDGE_LOOP('',(#24144,#24145,#24146,#24147,#24148));
#6770=EDGE_LOOP('',(#24149,#24150,#24151,#24152,#24153));
#6771=EDGE_LOOP('',(#24154,#24155,#24156,#24157));
#6772=EDGE_LOOP('',(#24158,#24159,#24160,#24161,#24162));
#6773=EDGE_LOOP('',(#24163,#24164,#24165,#24166,#24167,#24168));
#6774=EDGE_LOOP('',(#24169,#24170,#24171,#24172,#24173));
#6775=EDGE_LOOP('',(#24174,#24175,#24176,#24177,#24178));
#6776=EDGE_LOOP('',(#24179,#24180,#24181,#24182,#24183));
#6777=EDGE_LOOP('',(#24184,#24185,#24186,#24187,#24188));
#6778=EDGE_LOOP('',(#24189,#24190,#24191,#24192));
#6779=EDGE_LOOP('',(#24193,#24194,#24195,#24196,#24197));
#6780=EDGE_LOOP('',(#24198,#24199,#24200,#24201));
#6781=EDGE_LOOP('',(#24202,#24203,#24204,#24205));
#6782=EDGE_LOOP('',(#24206,#24207,#24208,#24209));
#6783=EDGE_LOOP('',(#24210,#24211,#24212,#24213));
#6784=EDGE_LOOP('',(#24214,#24215,#24216,#24217));
#6785=EDGE_LOOP('',(#24218,#24219,#24220,#24221));
#6786=EDGE_LOOP('',(#24222,#24223,#24224,#24225));
#6787=EDGE_LOOP('',(#24226,#24227,#24228,#24229));
#6788=EDGE_LOOP('',(#24230,#24231,#24232,#24233));
#6789=EDGE_LOOP('',(#24234,#24235,#24236,#24237));
#6790=EDGE_LOOP('',(#24238,#24239,#24240,#24241));
#6791=EDGE_LOOP('',(#24242,#24243,#24244,#24245));
#6792=EDGE_LOOP('',(#24246,#24247,#24248,#24249));
#6793=EDGE_LOOP('',(#24250,#24251,#24252,#24253));
#6794=EDGE_LOOP('',(#24254,#24255,#24256,#24257));
#6795=EDGE_LOOP('',(#24258,#24259,#24260,#24261));
#6796=EDGE_LOOP('',(#24262,#24263,#24264,#24265));
#6797=EDGE_LOOP('',(#24266,#24267,#24268,#24269));
#6798=EDGE_LOOP('',(#24270,#24271,#24272,#24273));
#6799=EDGE_LOOP('',(#24274,#24275,#24276,#24277));
#6800=EDGE_LOOP('',(#24278,#24279,#24280,#24281,#24282,#24283,#24284,#24285));
#6801=EDGE_LOOP('',(#24286,#24287,#24288,#24289,#24290,#24291,#24292,#24293));
#6802=EDGE_LOOP('',(#24294,#24295,#24296,#24297,#24298,#24299,#24300,#24301));
#6803=EDGE_LOOP('',(#24302,#24303,#24304,#24305,#24306,#24307,#24308,#24309));
#6804=EDGE_LOOP('',(#24310,#24311,#24312,#24313));
#6805=EDGE_LOOP('',(#24314,#24315,#24316,#24317));
#6806=EDGE_LOOP('',(#24318,#24319,#24320,#24321));
#6807=EDGE_LOOP('',(#24322,#24323,#24324,#24325));
#6808=EDGE_LOOP('',(#24326,#24327,#24328,#24329));
#6809=EDGE_LOOP('',(#24330,#24331,#24332,#24333));
#6810=EDGE_LOOP('',(#24334,#24335,#24336,#24337));
#6811=EDGE_LOOP('',(#24338,#24339,#24340,#24341));
#6812=EDGE_LOOP('',(#24342,#24343,#24344,#24345));
#6813=EDGE_LOOP('',(#24346,#24347,#24348,#24349));
#6814=EDGE_LOOP('',(#24350,#24351,#24352,#24353));
#6815=EDGE_LOOP('',(#24354,#24355,#24356,#24357));
#6816=EDGE_LOOP('',(#24358,#24359,#24360,#24361));
#6817=EDGE_LOOP('',(#24362,#24363,#24364,#24365));
#6818=EDGE_LOOP('',(#24366,#24367,#24368,#24369));
#6819=EDGE_LOOP('',(#24370,#24371,#24372,#24373));
#6820=EDGE_LOOP('',(#24374,#24375,#24376,#24377,#24378,#24379,#24380,#24381));
#6821=EDGE_LOOP('',(#24382,#24383,#24384,#24385,#24386,#24387,#24388,#24389));
#6822=EDGE_LOOP('',(#24390,#24391,#24392,#24393,#24394,#24395,#24396,#24397));
#6823=EDGE_LOOP('',(#24398,#24399,#24400,#24401,#24402,#24403,#24404,#24405));
#6824=EDGE_LOOP('',(#24406,#24407,#24408,#24409));
#6825=EDGE_LOOP('',(#24410,#24411,#24412,#24413));
#6826=EDGE_LOOP('',(#24414,#24415,#24416,#24417));
#6827=EDGE_LOOP('',(#24418,#24419,#24420,#24421));
#6828=EDGE_LOOP('',(#24422,#24423,#24424,#24425));
#6829=EDGE_LOOP('',(#24426,#24427,#24428,#24429));
#6830=EDGE_LOOP('',(#24430,#24431,#24432,#24433));
#6831=EDGE_LOOP('',(#24434,#24435,#24436,#24437));
#6832=EDGE_LOOP('',(#24438,#24439,#24440,#24441));
#6833=EDGE_LOOP('',(#24442,#24443,#24444,#24445));
#6834=EDGE_LOOP('',(#24446,#24447,#24448,#24449));
#6835=EDGE_LOOP('',(#24450,#24451,#24452,#24453));
#6836=EDGE_LOOP('',(#24454,#24455,#24456,#24457));
#6837=EDGE_LOOP('',(#24458,#24459,#24460,#24461));
#6838=EDGE_LOOP('',(#24462,#24463,#24464,#24465));
#6839=EDGE_LOOP('',(#24466,#24467,#24468,#24469));
#6840=EDGE_LOOP('',(#24470,#24471,#24472,#24473,#24474,#24475,#24476,#24477));
#6841=EDGE_LOOP('',(#24478,#24479,#24480,#24481,#24482,#24483,#24484,#24485));
#6842=EDGE_LOOP('',(#24486,#24487,#24488,#24489,#24490,#24491,#24492,#24493));
#6843=EDGE_LOOP('',(#24494,#24495,#24496,#24497,#24498,#24499,#24500,#24501));
#6844=EDGE_LOOP('',(#24502,#24503,#24504,#24505));
#6845=EDGE_LOOP('',(#24506,#24507,#24508,#24509));
#6846=EDGE_LOOP('',(#24510,#24511,#24512,#24513));
#6847=EDGE_LOOP('',(#24514,#24515,#24516,#24517));
#6848=EDGE_LOOP('',(#24518,#24519,#24520,#24521));
#6849=EDGE_LOOP('',(#24522,#24523,#24524,#24525));
#6850=EDGE_LOOP('',(#24526,#24527,#24528,#24529));
#6851=EDGE_LOOP('',(#24530,#24531,#24532,#24533));
#6852=EDGE_LOOP('',(#24534,#24535,#24536,#24537));
#6853=EDGE_LOOP('',(#24538,#24539,#24540,#24541));
#6854=EDGE_LOOP('',(#24542,#24543,#24544,#24545));
#6855=EDGE_LOOP('',(#24546,#24547,#24548,#24549));
#6856=EDGE_LOOP('',(#24550,#24551,#24552,#24553));
#6857=EDGE_LOOP('',(#24554,#24555,#24556,#24557));
#6858=EDGE_LOOP('',(#24558,#24559,#24560,#24561));
#6859=EDGE_LOOP('',(#24562,#24563,#24564,#24565));
#6860=EDGE_LOOP('',(#24566,#24567,#24568,#24569,#24570,#24571,#24572,#24573));
#6861=EDGE_LOOP('',(#24574,#24575,#24576,#24577,#24578,#24579,#24580,#24581));
#6862=EDGE_LOOP('',(#24582,#24583,#24584,#24585,#24586,#24587,#24588,#24589));
#6863=EDGE_LOOP('',(#24590,#24591,#24592,#24593,#24594,#24595,#24596,#24597));
#6864=EDGE_LOOP('',(#24598,#24599,#24600,#24601,#24602,#24603,#24604,#24605));
#6865=EDGE_LOOP('',(#24606,#24607,#24608,#24609,#24610,#24611,#24612,#24613));
#6866=EDGE_LOOP('',(#24614,#24615,#24616,#24617));
#6867=EDGE_LOOP('',(#24618,#24619,#24620,#24621));
#6868=EDGE_LOOP('',(#24622,#24623,#24624,#24625));
#6869=EDGE_LOOP('',(#24626,#24627,#24628,#24629));
#6870=EDGE_LOOP('',(#24630,#24631,#24632,#24633));
#6871=EDGE_LOOP('',(#24634,#24635,#24636,#24637));
#6872=EDGE_LOOP('',(#24638,#24639,#24640,#24641));
#6873=EDGE_LOOP('',(#24642,#24643,#24644,#24645,#24646,#24647,#24648,#24649));
#6874=EDGE_LOOP('',(#24650,#24651,#24652,#24653,#24654,#24655,#24656,#24657));
#6875=EDGE_LOOP('',(#24658,#24659,#24660,#24661));
#6876=EDGE_LOOP('',(#24662,#24663,#24664,#24665));
#6877=EDGE_LOOP('',(#24666,#24667,#24668,#24669));
#6878=EDGE_LOOP('',(#24670,#24671,#24672,#24673));
#6879=EDGE_LOOP('',(#24674,#24675,#24676,#24677));
#6880=EDGE_LOOP('',(#24678,#24679,#24680,#24681));
#6881=EDGE_LOOP('',(#24682,#24683,#24684,#24685));
#6882=EDGE_LOOP('',(#24686,#24687,#24688,#24689));
#6883=EDGE_LOOP('',(#24690,#24691,#24692,#24693));
#6884=EDGE_LOOP('',(#24694,#24695,#24696,#24697,#24698,#24699,#24700,#24701));
#6885=EDGE_LOOP('',(#24702,#24703,#24704,#24705,#24706,#24707,#24708,#24709));
#6886=EDGE_LOOP('',(#24710,#24711,#24712,#24713));
#6887=EDGE_LOOP('',(#24714,#24715,#24716,#24717));
#6888=EDGE_LOOP('',(#24718,#24719,#24720,#24721));
#6889=EDGE_LOOP('',(#24722,#24723,#24724,#24725));
#6890=EDGE_LOOP('',(#24726,#24727,#24728,#24729));
#6891=EDGE_LOOP('',(#24730,#24731,#24732,#24733));
#6892=EDGE_LOOP('',(#24734,#24735,#24736,#24737));
#6893=EDGE_LOOP('',(#24738,#24739,#24740,#24741));
#6894=EDGE_LOOP('',(#24742,#24743,#24744,#24745,#24746,#24747,#24748,#24749));
#6895=EDGE_LOOP('',(#24750,#24751,#24752,#24753,#24754,#24755,#24756,#24757));
#6896=EDGE_LOOP('',(#24758,#24759,#24760,#24761));
#6897=EDGE_LOOP('',(#24762,#24763,#24764,#24765));
#6898=EDGE_LOOP('',(#24766,#24767,#24768,#24769));
#6899=EDGE_LOOP('',(#24770,#24771,#24772,#24773));
#6900=EDGE_LOOP('',(#24774,#24775,#24776,#24777));
#6901=EDGE_LOOP('',(#24778,#24779,#24780,#24781));
#6902=EDGE_LOOP('',(#24782,#24783,#24784,#24785));
#6903=EDGE_LOOP('',(#24786,#24787,#24788,#24789));
#6904=EDGE_LOOP('',(#24790,#24791,#24792,#24793,#24794,#24795,#24796,#24797));
#6905=EDGE_LOOP('',(#24798,#24799,#24800,#24801,#24802,#24803,#24804,#24805));
#6906=EDGE_LOOP('',(#24806,#24807,#24808,#24809));
#6907=EDGE_LOOP('',(#24810,#24811,#24812,#24813));
#6908=EDGE_LOOP('',(#24814,#24815,#24816,#24817));
#6909=EDGE_LOOP('',(#24818,#24819,#24820,#24821));
#6910=EDGE_LOOP('',(#24822,#24823,#24824,#24825));
#6911=EDGE_LOOP('',(#24826,#24827,#24828,#24829));
#6912=EDGE_LOOP('',(#24830,#24831,#24832,#24833));
#6913=EDGE_LOOP('',(#24834,#24835,#24836,#24837));
#6914=EDGE_LOOP('',(#24838,#24839,#24840,#24841,#24842,#24843,#24844,#24845));
#6915=EDGE_LOOP('',(#24846,#24847,#24848,#24849,#24850,#24851,#24852,#24853));
#6916=EDGE_LOOP('',(#24854,#24855,#24856,#24857));
#6917=EDGE_LOOP('',(#24858,#24859,#24860,#24861));
#6918=EDGE_LOOP('',(#24862,#24863,#24864,#24865));
#6919=EDGE_LOOP('',(#24866,#24867,#24868,#24869));
#6920=EDGE_LOOP('',(#24870,#24871,#24872,#24873));
#6921=EDGE_LOOP('',(#24874,#24875,#24876,#24877));
#6922=EDGE_LOOP('',(#24878,#24879,#24880,#24881));
#6923=EDGE_LOOP('',(#24882,#24883,#24884,#24885));
#6924=EDGE_LOOP('',(#24886,#24887,#24888,#24889,#24890,#24891,#24892,#24893));
#6925=EDGE_LOOP('',(#24894,#24895,#24896,#24897,#24898,#24899,#24900,#24901));
#6926=EDGE_LOOP('',(#24902,#24903,#24904,#24905));
#6927=EDGE_LOOP('',(#24906,#24907,#24908,#24909));
#6928=EDGE_LOOP('',(#24910,#24911,#24912,#24913));
#6929=EDGE_LOOP('',(#24914,#24915,#24916,#24917));
#6930=EDGE_LOOP('',(#24918,#24919,#24920,#24921));
#6931=EDGE_LOOP('',(#24922,#24923,#24924,#24925));
#6932=EDGE_LOOP('',(#24926,#24927,#24928,#24929));
#6933=EDGE_LOOP('',(#24930,#24931,#24932,#24933));
#6934=EDGE_LOOP('',(#24934,#24935,#24936,#24937,#24938,#24939,#24940,#24941));
#6935=EDGE_LOOP('',(#24942,#24943,#24944,#24945,#24946,#24947,#24948,#24949));
#6936=EDGE_LOOP('',(#24950,#24951,#24952,#24953));
#6937=EDGE_LOOP('',(#24954,#24955,#24956,#24957));
#6938=EDGE_LOOP('',(#24958,#24959,#24960,#24961));
#6939=EDGE_LOOP('',(#24962,#24963,#24964,#24965));
#6940=EDGE_LOOP('',(#24966,#24967,#24968,#24969));
#6941=EDGE_LOOP('',(#24970,#24971,#24972,#24973));
#6942=EDGE_LOOP('',(#24974,#24975,#24976,#24977));
#6943=EDGE_LOOP('',(#24978,#24979,#24980,#24981));
#6944=EDGE_LOOP('',(#24982,#24983,#24984,#24985));
#6945=EDGE_LOOP('',(#24986,#24987,#24988,#24989));
#6946=EDGE_LOOP('',(#24990,#24991,#24992,#24993));
#6947=EDGE_LOOP('',(#24994,#24995,#24996,#24997));
#6948=EDGE_LOOP('',(#24998,#24999,#25000,#25001));
#6949=EDGE_LOOP('',(#25002,#25003,#25004,#25005));
#6950=EDGE_LOOP('',(#25006,#25007,#25008,#25009));
#6951=EDGE_LOOP('',(#25010,#25011,#25012,#25013));
#6952=EDGE_LOOP('',(#25014,#25015,#25016,#25017));
#6953=EDGE_LOOP('',(#25018,#25019,#25020,#25021));
#6954=EDGE_LOOP('',(#25022,#25023,#25024,#25025));
#6955=EDGE_LOOP('',(#25026,#25027,#25028,#25029));
#6956=EDGE_LOOP('',(#25030,#25031,#25032,#25033));
#6957=EDGE_LOOP('',(#25034,#25035,#25036,#25037));
#6958=EDGE_LOOP('',(#25038,#25039,#25040,#25041));
#6959=EDGE_LOOP('',(#25042,#25043,#25044,#25045));
#6960=EDGE_LOOP('',(#25046,#25047,#25048,#25049,#25050,#25051,#25052,#25053));
#6961=EDGE_LOOP('',(#25054,#25055,#25056,#25057,#25058,#25059,#25060,#25061));
#6962=EDGE_LOOP('',(#25062,#25063,#25064,#25065,#25066,#25067,#25068,#25069));
#6963=EDGE_LOOP('',(#25070,#25071,#25072,#25073,#25074,#25075,#25076,#25077));
#6964=EDGE_LOOP('',(#25078,#25079,#25080,#25081));
#6965=EDGE_LOOP('',(#25082,#25083,#25084,#25085));
#6966=EDGE_LOOP('',(#25086,#25087,#25088,#25089));
#6967=EDGE_LOOP('',(#25090,#25091,#25092,#25093));
#6968=EDGE_LOOP('',(#25094,#25095,#25096,#25097));
#6969=EDGE_LOOP('',(#25098,#25099,#25100,#25101));
#6970=EDGE_LOOP('',(#25102,#25103,#25104,#25105));
#6971=EDGE_LOOP('',(#25106,#25107,#25108,#25109));
#6972=EDGE_LOOP('',(#25110,#25111,#25112,#25113));
#6973=EDGE_LOOP('',(#25114,#25115,#25116,#25117));
#6974=EDGE_LOOP('',(#25118,#25119,#25120,#25121));
#6975=EDGE_LOOP('',(#25122,#25123,#25124,#25125));
#6976=EDGE_LOOP('',(#25126,#25127,#25128,#25129));
#6977=EDGE_LOOP('',(#25130,#25131,#25132,#25133));
#6978=EDGE_LOOP('',(#25134,#25135,#25136,#25137));
#6979=EDGE_LOOP('',(#25138,#25139,#25140,#25141));
#6980=EDGE_LOOP('',(#25142,#25143,#25144,#25145,#25146,#25147,#25148,#25149));
#6981=EDGE_LOOP('',(#25150,#25151,#25152,#25153,#25154,#25155,#25156,#25157));
#6982=EDGE_LOOP('',(#25158,#25159,#25160,#25161,#25162,#25163,#25164,#25165));
#6983=EDGE_LOOP('',(#25166,#25167,#25168,#25169,#25170,#25171,#25172,#25173));
#6984=EDGE_LOOP('',(#25174,#25175,#25176,#25177));
#6985=EDGE_LOOP('',(#25178,#25179,#25180,#25181));
#6986=EDGE_LOOP('',(#25182,#25183,#25184,#25185));
#6987=EDGE_LOOP('',(#25186,#25187,#25188,#25189));
#6988=EDGE_LOOP('',(#25190,#25191,#25192,#25193));
#6989=EDGE_LOOP('',(#25194,#25195,#25196,#25197));
#6990=EDGE_LOOP('',(#25198,#25199,#25200,#25201));
#6991=EDGE_LOOP('',(#25202,#25203,#25204,#25205));
#6992=EDGE_LOOP('',(#25206,#25207,#25208,#25209));
#6993=EDGE_LOOP('',(#25210,#25211,#25212,#25213));
#6994=EDGE_LOOP('',(#25214,#25215,#25216,#25217));
#6995=EDGE_LOOP('',(#25218,#25219,#25220,#25221));
#6996=EDGE_LOOP('',(#25222,#25223,#25224,#25225));
#6997=EDGE_LOOP('',(#25226,#25227,#25228,#25229));
#6998=EDGE_LOOP('',(#25230,#25231,#25232,#25233));
#6999=EDGE_LOOP('',(#25234,#25235,#25236,#25237));
#7000=EDGE_LOOP('',(#25238,#25239,#25240,#25241,#25242,#25243,#25244,#25245));
#7001=EDGE_LOOP('',(#25246,#25247,#25248,#25249,#25250,#25251,#25252,#25253));
#7002=EDGE_LOOP('',(#25254,#25255,#25256,#25257,#25258,#25259,#25260,#25261));
#7003=EDGE_LOOP('',(#25262,#25263,#25264,#25265,#25266,#25267,#25268,#25269));
#7004=EDGE_LOOP('',(#25270,#25271,#25272,#25273));
#7005=EDGE_LOOP('',(#25274,#25275,#25276,#25277));
#7006=EDGE_LOOP('',(#25278,#25279,#25280,#25281));
#7007=EDGE_LOOP('',(#25282,#25283,#25284,#25285));
#7008=EDGE_LOOP('',(#25286,#25287,#25288,#25289));
#7009=EDGE_LOOP('',(#25290,#25291,#25292,#25293));
#7010=EDGE_LOOP('',(#25294,#25295,#25296,#25297));
#7011=EDGE_LOOP('',(#25298,#25299,#25300,#25301));
#7012=EDGE_LOOP('',(#25302,#25303,#25304,#25305));
#7013=EDGE_LOOP('',(#25306,#25307,#25308,#25309));
#7014=EDGE_LOOP('',(#25310,#25311,#25312,#25313));
#7015=EDGE_LOOP('',(#25314,#25315,#25316,#25317));
#7016=EDGE_LOOP('',(#25318,#25319,#25320,#25321));
#7017=EDGE_LOOP('',(#25322,#25323,#25324,#25325));
#7018=EDGE_LOOP('',(#25326,#25327,#25328,#25329));
#7019=EDGE_LOOP('',(#25330,#25331,#25332,#25333));
#7020=EDGE_LOOP('',(#25334,#25335,#25336,#25337,#25338,#25339,#25340,#25341));
#7021=EDGE_LOOP('',(#25342,#25343,#25344,#25345,#25346,#25347,#25348,#25349));
#7022=EDGE_LOOP('',(#25350,#25351,#25352,#25353,#25354,#25355,#25356,#25357));
#7023=EDGE_LOOP('',(#25358,#25359,#25360,#25361,#25362,#25363,#25364,#25365));
#7024=EDGE_LOOP('',(#25366,#25367,#25368,#25369));
#7025=EDGE_LOOP('',(#25370,#25371,#25372,#25373));
#7026=EDGE_LOOP('',(#25374,#25375,#25376,#25377));
#7027=EDGE_LOOP('',(#25378,#25379,#25380,#25381));
#7028=EDGE_LOOP('',(#25382,#25383,#25384,#25385));
#7029=EDGE_LOOP('',(#25386,#25387,#25388,#25389));
#7030=EDGE_LOOP('',(#25390,#25391,#25392,#25393));
#7031=EDGE_LOOP('',(#25394,#25395,#25396,#25397));
#7032=EDGE_LOOP('',(#25398,#25399,#25400,#25401));
#7033=EDGE_LOOP('',(#25402,#25403,#25404,#25405));
#7034=EDGE_LOOP('',(#25406,#25407,#25408,#25409));
#7035=EDGE_LOOP('',(#25410,#25411,#25412,#25413));
#7036=EDGE_LOOP('',(#25414,#25415,#25416,#25417));
#7037=EDGE_LOOP('',(#25418,#25419,#25420,#25421));
#7038=EDGE_LOOP('',(#25422,#25423,#25424,#25425));
#7039=EDGE_LOOP('',(#25426,#25427,#25428,#25429));
#7040=EDGE_LOOP('',(#25430,#25431,#25432,#25433,#25434,#25435,#25436,#25437));
#7041=EDGE_LOOP('',(#25438,#25439,#25440,#25441,#25442,#25443,#25444,#25445));
#7042=EDGE_LOOP('',(#25446,#25447,#25448,#25449,#25450,#25451,#25452,#25453));
#7043=EDGE_LOOP('',(#25454,#25455,#25456,#25457,#25458,#25459,#25460,#25461));
#7044=EDGE_LOOP('',(#25462,#25463,#25464,#25465));
#7045=EDGE_LOOP('',(#25466,#25467,#25468,#25469));
#7046=EDGE_LOOP('',(#25470,#25471,#25472,#25473));
#7047=EDGE_LOOP('',(#25474,#25475,#25476,#25477));
#7048=EDGE_LOOP('',(#25478,#25479,#25480,#25481));
#7049=EDGE_LOOP('',(#25482,#25483,#25484,#25485));
#7050=EDGE_LOOP('',(#25486,#25487,#25488,#25489));
#7051=EDGE_LOOP('',(#25490,#25491,#25492,#25493));
#7052=EDGE_LOOP('',(#25494,#25495,#25496,#25497));
#7053=EDGE_LOOP('',(#25498,#25499,#25500,#25501));
#7054=EDGE_LOOP('',(#25502,#25503,#25504,#25505));
#7055=EDGE_LOOP('',(#25506,#25507,#25508,#25509));
#7056=EDGE_LOOP('',(#25510,#25511,#25512,#25513));
#7057=EDGE_LOOP('',(#25514,#25515,#25516,#25517));
#7058=EDGE_LOOP('',(#25518,#25519,#25520,#25521));
#7059=EDGE_LOOP('',(#25522,#25523,#25524,#25525));
#7060=EDGE_LOOP('',(#25526,#25527,#25528,#25529,#25530,#25531,#25532,#25533));
#7061=EDGE_LOOP('',(#25534,#25535,#25536,#25537,#25538,#25539,#25540,#25541));
#7062=EDGE_LOOP('',(#25542,#25543,#25544,#25545,#25546,#25547,#25548,#25549));
#7063=EDGE_LOOP('',(#25550,#25551,#25552,#25553,#25554,#25555,#25556,#25557));
#7064=EDGE_LOOP('',(#25558,#25559,#25560,#25561));
#7065=EDGE_LOOP('',(#25562,#25563,#25564,#25565));
#7066=EDGE_LOOP('',(#25566,#25567,#25568,#25569));
#7067=EDGE_LOOP('',(#25570,#25571,#25572,#25573));
#7068=EDGE_LOOP('',(#25574,#25575,#25576,#25577));
#7069=EDGE_LOOP('',(#25578,#25579,#25580,#25581));
#7070=EDGE_LOOP('',(#25582,#25583,#25584,#25585));
#7071=EDGE_LOOP('',(#25586,#25587,#25588,#25589));
#7072=EDGE_LOOP('',(#25590,#25591,#25592,#25593));
#7073=EDGE_LOOP('',(#25594,#25595,#25596,#25597));
#7074=EDGE_LOOP('',(#25598,#25599,#25600,#25601));
#7075=EDGE_LOOP('',(#25602,#25603,#25604,#25605));
#7076=EDGE_LOOP('',(#25606,#25607,#25608,#25609));
#7077=EDGE_LOOP('',(#25610,#25611,#25612,#25613));
#7078=EDGE_LOOP('',(#25614,#25615,#25616,#25617));
#7079=EDGE_LOOP('',(#25618,#25619,#25620,#25621));
#7080=EDGE_LOOP('',(#25622,#25623,#25624,#25625,#25626,#25627,#25628,#25629));
#7081=EDGE_LOOP('',(#25630,#25631,#25632,#25633,#25634,#25635,#25636,#25637));
#7082=EDGE_LOOP('',(#25638,#25639,#25640,#25641,#25642,#25643,#25644,#25645));
#7083=EDGE_LOOP('',(#25646,#25647,#25648,#25649,#25650,#25651,#25652,#25653));
#7084=EDGE_LOOP('',(#25654,#25655,#25656,#25657));
#7085=EDGE_LOOP('',(#25658,#25659,#25660,#25661));
#7086=EDGE_LOOP('',(#25662,#25663,#25664,#25665));
#7087=EDGE_LOOP('',(#25666,#25667,#25668,#25669));
#7088=EDGE_LOOP('',(#25670,#25671,#25672,#25673));
#7089=EDGE_LOOP('',(#25674,#25675,#25676,#25677));
#7090=EDGE_LOOP('',(#25678,#25679,#25680,#25681));
#7091=EDGE_LOOP('',(#25682,#25683,#25684,#25685));
#7092=EDGE_LOOP('',(#25686,#25687,#25688,#25689));
#7093=EDGE_LOOP('',(#25690,#25691,#25692,#25693));
#7094=EDGE_LOOP('',(#25694,#25695,#25696,#25697));
#7095=EDGE_LOOP('',(#25698,#25699,#25700,#25701));
#7096=EDGE_LOOP('',(#25702,#25703,#25704,#25705));
#7097=EDGE_LOOP('',(#25706,#25707,#25708,#25709));
#7098=EDGE_LOOP('',(#25710,#25711,#25712,#25713));
#7099=EDGE_LOOP('',(#25714,#25715,#25716,#25717));
#7100=EDGE_LOOP('',(#25718,#25719,#25720,#25721));
#7101=EDGE_LOOP('',(#25722));
#7102=EDGE_LOOP('',(#25723));
#7103=EDGE_LOOP('',(#25724));
#7104=EDGE_LOOP('',(#25725));
#7105=EDGE_LOOP('',(#25726));
#7106=EDGE_LOOP('',(#25727));
#7107=EDGE_LOOP('',(#25728));
#7108=EDGE_LOOP('',(#25729));
#7109=EDGE_LOOP('',(#25730,#25731,#25732,#25733));
#7110=EDGE_LOOP('',(#25734,#25735,#25736,#25737));
#7111=EDGE_LOOP('',(#25738));
#7112=EDGE_LOOP('',(#25739));
#7113=EDGE_LOOP('',(#25740));
#7114=EDGE_LOOP('',(#25741));
#7115=EDGE_LOOP('',(#25742));
#7116=EDGE_LOOP('',(#25743));
#7117=EDGE_LOOP('',(#25744));
#7118=EDGE_LOOP('',(#25745));
#7119=EDGE_LOOP('',(#25746,#25747,#25748,#25749));
#7120=EDGE_LOOP('',(#25750,#25751,#25752,#25753));
#7121=EDGE_LOOP('',(#25754,#25755,#25756,#25757));
#7122=EDGE_LOOP('',(#25758,#25759,#25760,#25761));
#7123=EDGE_LOOP('',(#25762));
#7124=EDGE_LOOP('',(#25763));
#7125=EDGE_LOOP('',(#25764));
#7126=EDGE_LOOP('',(#25765));
#7127=EDGE_LOOP('',(#25766));
#7128=EDGE_LOOP('',(#25767));
#7129=EDGE_LOOP('',(#25768));
#7130=EDGE_LOOP('',(#25769));
#7131=EDGE_LOOP('',(#25770,#25771,#25772,#25773));
#7132=EDGE_LOOP('',(#25774,#25775,#25776,#25777));
#7133=EDGE_LOOP('',(#25778));
#7134=EDGE_LOOP('',(#25779));
#7135=EDGE_LOOP('',(#25780));
#7136=EDGE_LOOP('',(#25781));
#7137=EDGE_LOOP('',(#25782));
#7138=EDGE_LOOP('',(#25783));
#7139=EDGE_LOOP('',(#25784));
#7140=EDGE_LOOP('',(#25785));
#7141=EDGE_LOOP('',(#25786,#25787,#25788,#25789));
#7142=EDGE_LOOP('',(#25790,#25791,#25792,#25793));
#7143=EDGE_LOOP('',(#25794,#25795,#25796,#25797));
#7144=EDGE_LOOP('',(#25798,#25799,#25800,#25801));
#7145=EDGE_LOOP('',(#25802));
#7146=EDGE_LOOP('',(#25803));
#7147=EDGE_LOOP('',(#25804));
#7148=EDGE_LOOP('',(#25805,#25806,#25807,#25808));
#7149=EDGE_LOOP('',(#25809));
#7150=EDGE_LOOP('',(#25810));
#7151=EDGE_LOOP('',(#25811));
#7152=EDGE_LOOP('',(#25812,#25813,#25814,#25815));
#7153=EDGE_LOOP('',(#25816,#25817,#25818));
#7154=EDGE_LOOP('',(#25819,#25820,#25821,#25822));
#7155=EDGE_LOOP('',(#25823,#25824,#25825));
#7156=EDGE_LOOP('',(#25826,#25827,#25828,#25829));
#7157=EDGE_LOOP('',(#25830,#25831,#25832));
#7158=EDGE_LOOP('',(#25833,#25834,#25835,#25836));
#7159=EDGE_LOOP('',(#25837,#25838,#25839));
#7160=EDGE_LOOP('',(#25840,#25841,#25842,#25843));
#7161=EDGE_LOOP('',(#25844,#25845,#25846));
#7162=EDGE_LOOP('',(#25847,#25848,#25849,#25850));
#7163=EDGE_LOOP('',(#25851,#25852,#25853));
#7164=EDGE_LOOP('',(#25854,#25855,#25856,#25857));
#7165=EDGE_LOOP('',(#25858,#25859,#25860,#25861));
#7166=EDGE_LOOP('',(#25862,#25863,#25864,#25865));
#7167=EDGE_LOOP('',(#25866,#25867,#25868,#25869));
#7168=EDGE_LOOP('',(#25870,#25871,#25872,#25873));
#7169=EDGE_LOOP('',(#25874,#25875,#25876,#25877));
#7170=EDGE_LOOP('',(#25878,#25879,#25880,#25881));
#7171=EDGE_LOOP('',(#25882,#25883,#25884,#25885));
#7172=EDGE_LOOP('',(#25886,#25887,#25888,#25889));
#7173=EDGE_LOOP('',(#25890,#25891,#25892,#25893));
#7174=EDGE_LOOP('',(#25894,#25895,#25896,#25897));
#7175=EDGE_LOOP('',(#25898,#25899,#25900,#25901));
#7176=EDGE_LOOP('',(#25902));
#7177=EDGE_LOOP('',(#25903));
#7178=EDGE_LOOP('',(#25904));
#7179=EDGE_LOOP('',(#25905));
#7180=EDGE_LOOP('',(#25906));
#7181=EDGE_LOOP('',(#25907));
#7182=EDGE_LOOP('',(#25908));
#7183=EDGE_LOOP('',(#25909));
#7184=EDGE_LOOP('',(#25910));
#7185=EDGE_LOOP('',(#25911));
#7186=EDGE_LOOP('',(#25912,#25913,#25914,#25915));
#7187=EDGE_LOOP('',(#25916,#25917,#25918,#25919));
#7188=EDGE_LOOP('',(#25920));
#7189=EDGE_LOOP('',(#25921));
#7190=EDGE_LOOP('',(#25922));
#7191=EDGE_LOOP('',(#25923));
#7192=EDGE_LOOP('',(#25924));
#7193=EDGE_LOOP('',(#25925));
#7194=EDGE_LOOP('',(#25926));
#7195=EDGE_LOOP('',(#25927));
#7196=EDGE_LOOP('',(#25928));
#7197=EDGE_LOOP('',(#25929));
#7198=EDGE_LOOP('',(#25930,#25931,#25932,#25933));
#7199=EDGE_LOOP('',(#25934));
#7200=EDGE_LOOP('',(#25935));
#7201=EDGE_LOOP('',(#25936));
#7202=EDGE_LOOP('',(#25937,#25938,#25939,#25940));
#7203=EDGE_LOOP('',(#25941));
#7204=EDGE_LOOP('',(#25942));
#7205=EDGE_LOOP('',(#25943));
#7206=EDGE_LOOP('',(#25944,#25945,#25946,#25947));
#7207=EDGE_LOOP('',(#25948,#25949,#25950));
#7208=EDGE_LOOP('',(#25951,#25952,#25953,#25954));
#7209=EDGE_LOOP('',(#25955,#25956,#25957));
#7210=EDGE_LOOP('',(#25958,#25959,#25960,#25961));
#7211=EDGE_LOOP('',(#25962,#25963,#25964));
#7212=EDGE_LOOP('',(#25965,#25966,#25967,#25968));
#7213=EDGE_LOOP('',(#25969,#25970,#25971));
#7214=EDGE_LOOP('',(#25972,#25973,#25974,#25975));
#7215=EDGE_LOOP('',(#25976,#25977,#25978));
#7216=EDGE_LOOP('',(#25979,#25980,#25981,#25982));
#7217=EDGE_LOOP('',(#25983,#25984,#25985));
#7218=EDGE_LOOP('',(#25986,#25987,#25988,#25989));
#7219=EDGE_LOOP('',(#25990,#25991,#25992,#25993));
#7220=EDGE_LOOP('',(#25994,#25995,#25996,#25997));
#7221=EDGE_LOOP('',(#25998,#25999,#26000,#26001));
#7222=EDGE_LOOP('',(#26002,#26003,#26004,#26005));
#7223=EDGE_LOOP('',(#26006,#26007,#26008,#26009));
#7224=EDGE_LOOP('',(#26010,#26011,#26012,#26013));
#7225=EDGE_LOOP('',(#26014,#26015,#26016,#26017));
#7226=EDGE_LOOP('',(#26018,#26019,#26020,#26021));
#7227=EDGE_LOOP('',(#26022,#26023,#26024,#26025));
#7228=EDGE_LOOP('',(#26026,#26027,#26028,#26029));
#7229=EDGE_LOOP('',(#26030,#26031,#26032,#26033));
#7230=EDGE_LOOP('',(#26034));
#7231=EDGE_LOOP('',(#26035));
#7232=EDGE_LOOP('',(#26036));
#7233=EDGE_LOOP('',(#26037));
#7234=EDGE_LOOP('',(#26038));
#7235=EDGE_LOOP('',(#26039));
#7236=EDGE_LOOP('',(#26040));
#7237=EDGE_LOOP('',(#26041));
#7238=EDGE_LOOP('',(#26042));
#7239=EDGE_LOOP('',(#26043));
#7240=EDGE_LOOP('',(#26044,#26045,#26046,#26047));
#7241=EDGE_LOOP('',(#26048,#26049,#26050,#26051));
#7242=EDGE_LOOP('',(#26052));
#7243=EDGE_LOOP('',(#26053));
#7244=EDGE_LOOP('',(#26054));
#7245=EDGE_LOOP('',(#26055));
#7246=EDGE_LOOP('',(#26056));
#7247=EDGE_LOOP('',(#26057));
#7248=EDGE_LOOP('',(#26058));
#7249=EDGE_LOOP('',(#26059));
#7250=EDGE_LOOP('',(#26060));
#7251=EDGE_LOOP('',(#26061));
#7252=EDGE_LOOP('',(#26062,#26063,#26064,#26065));
#7253=EDGE_LOOP('',(#26066,#26067,#26068,#26069));
#7254=EDGE_LOOP('',(#26070,#26071,#26072,#26073));
#7255=EDGE_LOOP('',(#26074,#26075,#26076,#26077));
#7256=EDGE_LOOP('',(#26078,#26079,#26080,#26081));
#7257=EDGE_LOOP('',(#26082,#26083,#26084,#26085));
#7258=EDGE_LOOP('',(#26086,#26087,#26088,#26089));
#7259=EDGE_LOOP('',(#26090,#26091,#26092,#26093));
#7260=EDGE_LOOP('',(#26094,#26095,#26096,#26097));
#7261=EDGE_LOOP('',(#26098,#26099,#26100,#26101));
#7262=EDGE_LOOP('',(#26102,#26103,#26104,#26105));
#7263=EDGE_LOOP('',(#26106));
#7264=EDGE_LOOP('',(#26107));
#7265=EDGE_LOOP('',(#26108));
#7266=EDGE_LOOP('',(#26109));
#7267=EDGE_LOOP('',(#26110));
#7268=EDGE_LOOP('',(#26111));
#7269=EDGE_LOOP('',(#26112,#26113,#26114,#26115));
#7270=EDGE_LOOP('',(#26116));
#7271=EDGE_LOOP('',(#26117));
#7272=EDGE_LOOP('',(#26118));
#7273=EDGE_LOOP('',(#26119));
#7274=EDGE_LOOP('',(#26120));
#7275=EDGE_LOOP('',(#26121));
#7276=EDGE_LOOP('',(#26122,#26123,#26124,#26125));
#7277=EDGE_LOOP('',(#26126,#26127,#26128,#26129));
#7278=EDGE_LOOP('',(#26130,#26131,#26132,#26133,#26134,#26135,#26136,#26137));
#7279=EDGE_LOOP('',(#26138,#26139,#26140,#26141));
#7280=EDGE_LOOP('',(#26142,#26143,#26144,#26145,#26146,#26147,#26148,#26149));
#7281=EDGE_LOOP('',(#26150,#26151,#26152,#26153));
#7282=EDGE_LOOP('',(#26154,#26155,#26156,#26157));
#7283=EDGE_LOOP('',(#26158,#26159,#26160,#26161));
#7284=EDGE_LOOP('',(#26162,#26163,#26164,#26165));
#7285=EDGE_LOOP('',(#26166,#26167,#26168,#26169));
#7286=EDGE_LOOP('',(#26170,#26171,#26172,#26173));
#7287=EDGE_LOOP('',(#26174,#26175,#26176,#26177));
#7288=EDGE_LOOP('',(#26178,#26179,#26180,#26181));
#7289=EDGE_LOOP('',(#26182,#26183,#26184,#26185));
#7290=EDGE_LOOP('',(#26186,#26187,#26188,#26189));
#7291=EDGE_LOOP('',(#26190,#26191,#26192,#26193));
#7292=EDGE_LOOP('',(#26194,#26195,#26196,#26197));
#7293=EDGE_LOOP('',(#26198,#26199,#26200,#26201));
#7294=EDGE_LOOP('',(#26202,#26203,#26204,#26205));
#7295=EDGE_LOOP('',(#26206,#26207,#26208,#26209));
#7296=EDGE_LOOP('',(#26210,#26211,#26212,#26213));
#7297=EDGE_LOOP('',(#26214,#26215,#26216,#26217));
#7298=EDGE_LOOP('',(#26218,#26219,#26220,#26221));
#7299=EDGE_LOOP('',(#26222));
#7300=EDGE_LOOP('',(#26223));
#7301=EDGE_LOOP('',(#26224));
#7302=EDGE_LOOP('',(#26225));
#7303=EDGE_LOOP('',(#26226,#26227,#26228,#26229));
#7304=EDGE_LOOP('',(#26230,#26231,#26232,#26233));
#7305=EDGE_LOOP('',(#26234));
#7306=EDGE_LOOP('',(#26235));
#7307=EDGE_LOOP('',(#26236));
#7308=EDGE_LOOP('',(#26237));
#7309=EDGE_LOOP('',(#26238,#26239,#26240,#26241));
#7310=EDGE_LOOP('',(#26242,#26243,#26244,#26245,#26246,#26247));
#7311=EDGE_LOOP('',(#26248,#26249,#26250,#26251));
#7312=EDGE_LOOP('',(#26252,#26253,#26254,#26255));
#7313=EDGE_LOOP('',(#26256,#26257,#26258,#26259));
#7314=EDGE_LOOP('',(#26260,#26261,#26262,#26263));
#7315=EDGE_LOOP('',(#26264,#26265,#26266,#26267));
#7316=EDGE_LOOP('',(#26268,#26269,#26270,#26271,#26272));
#7317=EDGE_LOOP('',(#26273));
#7318=EDGE_LOOP('',(#26274));
#7319=EDGE_LOOP('',(#26275,#26276,#26277,#26278,#26279));
#7320=EDGE_LOOP('',(#26280,#26281,#26282,#26283));
#7321=EDGE_LOOP('',(#26284,#26285,#26286,#26287,#26288));
#7322=EDGE_LOOP('',(#26289));
#7323=EDGE_LOOP('',(#26290));
#7324=EDGE_LOOP('',(#26291,#26292,#26293,#26294,#26295,#26296));
#7325=EDGE_LOOP('',(#26297,#26298,#26299,#26300,#26301));
#7326=EDGE_LOOP('',(#26302,#26303,#26304,#26305,#26306,#26307));
#7327=EDGE_LOOP('',(#26308,#26309,#26310,#26311,#26312));
#7328=EDGE_LOOP('',(#26313,#26314,#26315,#26316,#26317,#26318));
#7329=EDGE_LOOP('',(#26319,#26320,#26321,#26322,#26323));
#7330=EDGE_LOOP('',(#26324));
#7331=EDGE_LOOP('',(#26325,#26326,#26327,#26328,#26329));
#7332=EDGE_LOOP('',(#26330,#26331,#26332,#26333));
#7333=EDGE_LOOP('',(#26334,#26335,#26336,#26337));
#7334=EDGE_LOOP('',(#26338,#26339,#26340,#26341,#26342));
#7335=EDGE_LOOP('',(#26343,#26344,#26345,#26346));
#7336=EDGE_LOOP('',(#26347,#26348,#26349,#26350,#26351,#26352));
#7337=EDGE_LOOP('',(#26353,#26354,#26355,#26356));
#7338=EDGE_LOOP('',(#26357));
#7339=EDGE_LOOP('',(#26358,#26359,#26360,#26361,#26362));
#7340=EDGE_LOOP('',(#26363));
#7341=EDGE_LOOP('',(#26364));
#7342=EDGE_LOOP('',(#26365,#26366,#26367,#26368,#26369));
#7343=EDGE_LOOP('',(#26370,#26371,#26372,#26373,#26374));
#7344=EDGE_LOOP('',(#26375));
#7345=EDGE_LOOP('',(#26376));
#7346=EDGE_LOOP('',(#26377,#26378,#26379,#26380,#26381));
#7347=EDGE_LOOP('',(#26382,#26383,#26384,#26385,#26386,#26387));
#7348=EDGE_LOOP('',(#26388,#26389,#26390,#26391,#26392));
#7349=EDGE_LOOP('',(#26393,#26394,#26395,#26396,#26397));
#7350=EDGE_LOOP('',(#26398,#26399,#26400,#26401));
#7351=EDGE_LOOP('',(#26402));
#7352=EDGE_LOOP('',(#26403,#26404,#26405,#26406,#26407));
#7353=EDGE_LOOP('',(#26408,#26409,#26410,#26411,#26412,#26413));
#7354=EDGE_LOOP('',(#26414));
#7355=EDGE_LOOP('',(#26415));
#7356=EDGE_LOOP('',(#26416,#26417,#26418,#26419));
#7357=EDGE_LOOP('',(#26420,#26421,#26422,#26423));
#7358=EDGE_LOOP('',(#26424,#26425,#26426,#26427));
#7359=EDGE_LOOP('',(#26428,#26429,#26430,#26431));
#7360=EDGE_LOOP('',(#26432,#26433,#26434,#26435));
#7361=EDGE_LOOP('',(#26436,#26437,#26438,#26439,#26440));
#7362=EDGE_LOOP('',(#26441));
#7363=EDGE_LOOP('',(#26442));
#7364=EDGE_LOOP('',(#26443,#26444,#26445,#26446,#26447,#26448));
#7365=EDGE_LOOP('',(#26449,#26450,#26451,#26452,#26453));
#7366=EDGE_LOOP('',(#26454,#26455,#26456,#26457,#26458,#26459));
#7367=EDGE_LOOP('',(#26460,#26461,#26462,#26463,#26464));
#7368=EDGE_LOOP('',(#26465));
#7369=EDGE_LOOP('',(#26466));
#7370=EDGE_LOOP('',(#26467,#26468,#26469,#26470,#26471));
#7371=EDGE_LOOP('',(#26472,#26473,#26474,#26475,#26476,#26477));
#7372=EDGE_LOOP('',(#26478,#26479,#26480,#26481,#26482));
#7373=EDGE_LOOP('',(#26483));
#7374=EDGE_LOOP('',(#26484,#26485,#26486,#26487,#26488));
#7375=EDGE_LOOP('',(#26489,#26490,#26491,#26492));
#7376=EDGE_LOOP('',(#26493,#26494,#26495,#26496));
#7377=EDGE_LOOP('',(#26497,#26498,#26499,#26500,#26501));
#7378=EDGE_LOOP('',(#26502,#26503,#26504,#26505));
#7379=EDGE_LOOP('',(#26506,#26507,#26508,#26509,#26510,#26511));
#7380=EDGE_LOOP('',(#26512,#26513,#26514,#26515,#26516));
#7381=EDGE_LOOP('',(#26517));
#7382=EDGE_LOOP('',(#26518));
#7383=EDGE_LOOP('',(#26519,#26520,#26521,#26522,#26523));
#7384=EDGE_LOOP('',(#26524,#26525,#26526,#26527,#26528));
#7385=EDGE_LOOP('',(#26529));
#7386=EDGE_LOOP('',(#26530));
#7387=EDGE_LOOP('',(#26531,#26532,#26533,#26534,#26535));
#7388=EDGE_LOOP('',(#26536,#26537,#26538,#26539));
#7389=EDGE_LOOP('',(#26540,#26541,#26542,#26543));
#7390=EDGE_LOOP('',(#26544,#26545,#26546,#26547));
#7391=EDGE_LOOP('',(#26548));
#7392=EDGE_LOOP('',(#26549,#26550,#26551,#26552));
#7393=EDGE_LOOP('',(#26553,#26554,#26555,#26556));
#7394=EDGE_LOOP('',(#26557,#26558,#26559,#26560));
#7395=EDGE_LOOP('',(#26561));
#7396=EDGE_LOOP('',(#26562,#26563,#26564,#26565));
#7397=EDGE_LOOP('',(#26566,#26567,#26568,#26569));
#7398=EDGE_LOOP('',(#26570,#26571,#26572,#26573));
#7399=EDGE_LOOP('',(#26574));
#7400=EDGE_LOOP('',(#26575));
#7401=EDGE_LOOP('',(#26576));
#7402=EDGE_LOOP('',(#26577));
#7403=EDGE_LOOP('',(#26578,#26579,#26580,#26581,#26582));
#7404=EDGE_LOOP('',(#26583,#26584,#26585,#26586,#26587));
#7405=EDGE_LOOP('',(#26588));
#7406=EDGE_LOOP('',(#26589,#26590,#26591,#26592));
#7407=EDGE_LOOP('',(#26593,#26594,#26595,#26596));
#7408=EDGE_LOOP('',(#26597,#26598,#26599,#26600,#26601,#26602,#26603,#26604,
#26605,#26606,#26607,#26608,#26609,#26610,#26611,#26612,#26613,#26614,#26615,
#26616,#26617,#26618,#26619,#26620,#26621,#26622,#26623,#26624,#26625,#26626,
#26627,#26628,#26629,#26630,#26631,#26632,#26633,#26634,#26635,#26636,#26637,
#26638,#26639,#26640,#26641,#26642,#26643,#26644,#26645,#26646,#26647,#26648,
#26649,#26650,#26651,#26652,#26653,#26654,#26655,#26656,#26657,#26658,#26659,
#26660,#26661,#26662,#26663,#26664,#26665,#26666,#26667,#26668,#26669,#26670,
#26671,#26672,#26673,#26674,#26675,#26676,#26677,#26678,#26679,#26680,#26681,
#26682,#26683,#26684,#26685,#26686,#26687,#26688,#26689,#26690,#26691,#26692,
#26693,#26694,#26695,#26696,#26697,#26698,#26699,#26700,#26701,#26702,#26703,
#26704,#26705,#26706,#26707,#26708,#26709,#26710,#26711,#26712,#26713,#26714,
#26715,#26716,#26717,#26718,#26719,#26720,#26721,#26722,#26723,#26724,#26725,
#26726,#26727,#26728,#26729,#26730,#26731,#26732,#26733,#26734,#26735,#26736,
#26737,#26738,#26739,#26740,#26741,#26742,#26743,#26744,#26745,#26746,#26747,
#26748,#26749,#26750,#26751,#26752,#26753,#26754,#26755,#26756,#26757,#26758,
#26759,#26760,#26761,#26762,#26763,#26764,#26765,#26766,#26767,#26768,#26769,
#26770,#26771,#26772,#26773,#26774,#26775,#26776,#26777,#26778,#26779,#26780,
#26781,#26782,#26783,#26784,#26785,#26786,#26787,#26788));
#7409=EDGE_LOOP('',(#26789));
#7410=EDGE_LOOP('',(#26790,#26791,#26792,#26793));
#7411=EDGE_LOOP('',(#26794,#26795,#26796,#26797));
#7412=EDGE_LOOP('',(#26798,#26799,#26800,#26801));
#7413=EDGE_LOOP('',(#26802,#26803,#26804,#26805));
#7414=EDGE_LOOP('',(#26806,#26807,#26808,#26809));
#7415=EDGE_LOOP('',(#26810,#26811,#26812,#26813));
#7416=EDGE_LOOP('',(#26814,#26815,#26816,#26817));
#7417=EDGE_LOOP('',(#26818,#26819,#26820,#26821));
#7418=EDGE_LOOP('',(#26822,#26823,#26824,#26825));
#7419=EDGE_LOOP('',(#26826,#26827,#26828,#26829));
#7420=EDGE_LOOP('',(#26830,#26831,#26832,#26833));
#7421=EDGE_LOOP('',(#26834,#26835,#26836,#26837));
#7422=EDGE_LOOP('',(#26838,#26839,#26840,#26841));
#7423=EDGE_LOOP('',(#26842,#26843,#26844,#26845));
#7424=EDGE_LOOP('',(#26846,#26847,#26848,#26849));
#7425=EDGE_LOOP('',(#26850,#26851,#26852,#26853));
#7426=EDGE_LOOP('',(#26854,#26855,#26856,#26857));
#7427=EDGE_LOOP('',(#26858,#26859,#26860,#26861));
#7428=EDGE_LOOP('',(#26862,#26863,#26864,#26865));
#7429=EDGE_LOOP('',(#26866,#26867,#26868,#26869));
#7430=EDGE_LOOP('',(#26870,#26871,#26872,#26873));
#7431=EDGE_LOOP('',(#26874,#26875,#26876,#26877));
#7432=EDGE_LOOP('',(#26878,#26879,#26880,#26881));
#7433=EDGE_LOOP('',(#26882,#26883,#26884,#26885));
#7434=EDGE_LOOP('',(#26886,#26887,#26888,#26889));
#7435=EDGE_LOOP('',(#26890,#26891,#26892,#26893));
#7436=EDGE_LOOP('',(#26894,#26895,#26896,#26897));
#7437=EDGE_LOOP('',(#26898,#26899,#26900,#26901));
#7438=EDGE_LOOP('',(#26902,#26903,#26904,#26905));
#7439=EDGE_LOOP('',(#26906,#26907,#26908,#26909));
#7440=EDGE_LOOP('',(#26910,#26911,#26912,#26913));
#7441=EDGE_LOOP('',(#26914,#26915,#26916,#26917));
#7442=EDGE_LOOP('',(#26918,#26919,#26920,#26921));
#7443=EDGE_LOOP('',(#26922,#26923,#26924,#26925));
#7444=EDGE_LOOP('',(#26926,#26927,#26928,#26929));
#7445=EDGE_LOOP('',(#26930,#26931,#26932,#26933));
#7446=EDGE_LOOP('',(#26934,#26935,#26936,#26937));
#7447=EDGE_LOOP('',(#26938,#26939,#26940,#26941));
#7448=EDGE_LOOP('',(#26942,#26943,#26944,#26945));
#7449=EDGE_LOOP('',(#26946,#26947,#26948,#26949));
#7450=EDGE_LOOP('',(#26950,#26951,#26952,#26953));
#7451=EDGE_LOOP('',(#26954,#26955,#26956,#26957));
#7452=EDGE_LOOP('',(#26958,#26959,#26960,#26961));
#7453=EDGE_LOOP('',(#26962,#26963,#26964,#26965));
#7454=EDGE_LOOP('',(#26966,#26967,#26968,#26969));
#7455=EDGE_LOOP('',(#26970,#26971,#26972,#26973));
#7456=EDGE_LOOP('',(#26974,#26975,#26976,#26977));
#7457=EDGE_LOOP('',(#26978,#26979,#26980,#26981));
#7458=EDGE_LOOP('',(#26982,#26983,#26984,#26985));
#7459=EDGE_LOOP('',(#26986,#26987,#26988,#26989));
#7460=EDGE_LOOP('',(#26990,#26991,#26992,#26993));
#7461=EDGE_LOOP('',(#26994,#26995,#26996,#26997));
#7462=EDGE_LOOP('',(#26998,#26999,#27000,#27001));
#7463=EDGE_LOOP('',(#27002,#27003,#27004,#27005));
#7464=EDGE_LOOP('',(#27006,#27007,#27008,#27009));
#7465=EDGE_LOOP('',(#27010,#27011,#27012,#27013));
#7466=EDGE_LOOP('',(#27014,#27015,#27016,#27017));
#7467=EDGE_LOOP('',(#27018,#27019,#27020,#27021));
#7468=EDGE_LOOP('',(#27022,#27023,#27024,#27025));
#7469=EDGE_LOOP('',(#27026,#27027,#27028,#27029));
#7470=EDGE_LOOP('',(#27030,#27031,#27032,#27033));
#7471=EDGE_LOOP('',(#27034,#27035,#27036,#27037));
#7472=EDGE_LOOP('',(#27038,#27039,#27040,#27041));
#7473=EDGE_LOOP('',(#27042,#27043,#27044,#27045));
#7474=EDGE_LOOP('',(#27046,#27047,#27048,#27049));
#7475=EDGE_LOOP('',(#27050,#27051,#27052,#27053));
#7476=EDGE_LOOP('',(#27054,#27055,#27056,#27057));
#7477=EDGE_LOOP('',(#27058,#27059,#27060,#27061));
#7478=EDGE_LOOP('',(#27062,#27063,#27064,#27065));
#7479=EDGE_LOOP('',(#27066,#27067,#27068,#27069));
#7480=EDGE_LOOP('',(#27070,#27071,#27072,#27073));
#7481=EDGE_LOOP('',(#27074,#27075,#27076,#27077));
#7482=EDGE_LOOP('',(#27078,#27079,#27080,#27081));
#7483=EDGE_LOOP('',(#27082,#27083,#27084,#27085));
#7484=EDGE_LOOP('',(#27086,#27087,#27088,#27089));
#7485=EDGE_LOOP('',(#27090,#27091,#27092,#27093));
#7486=EDGE_LOOP('',(#27094,#27095,#27096,#27097));
#7487=EDGE_LOOP('',(#27098,#27099,#27100,#27101));
#7488=EDGE_LOOP('',(#27102,#27103,#27104,#27105));
#7489=EDGE_LOOP('',(#27106,#27107,#27108,#27109));
#7490=EDGE_LOOP('',(#27110,#27111,#27112,#27113));
#7491=EDGE_LOOP('',(#27114,#27115,#27116,#27117));
#7492=EDGE_LOOP('',(#27118,#27119,#27120,#27121));
#7493=EDGE_LOOP('',(#27122,#27123,#27124,#27125));
#7494=EDGE_LOOP('',(#27126,#27127,#27128,#27129));
#7495=EDGE_LOOP('',(#27130,#27131,#27132,#27133));
#7496=EDGE_LOOP('',(#27134,#27135,#27136,#27137));
#7497=EDGE_LOOP('',(#27138,#27139,#27140,#27141));
#7498=EDGE_LOOP('',(#27142,#27143,#27144,#27145));
#7499=EDGE_LOOP('',(#27146,#27147,#27148,#27149));
#7500=EDGE_LOOP('',(#27150,#27151,#27152,#27153));
#7501=EDGE_LOOP('',(#27154,#27155,#27156,#27157));
#7502=EDGE_LOOP('',(#27158,#27159,#27160,#27161));
#7503=EDGE_LOOP('',(#27162,#27163,#27164,#27165));
#7504=EDGE_LOOP('',(#27166,#27167,#27168,#27169));
#7505=EDGE_LOOP('',(#27170,#27171,#27172,#27173));
#7506=EDGE_LOOP('',(#27174,#27175,#27176,#27177));
#7507=EDGE_LOOP('',(#27178,#27179,#27180,#27181));
#7508=EDGE_LOOP('',(#27182,#27183,#27184,#27185));
#7509=EDGE_LOOP('',(#27186,#27187,#27188,#27189));
#7510=EDGE_LOOP('',(#27190,#27191,#27192,#27193));
#7511=EDGE_LOOP('',(#27194,#27195,#27196,#27197));
#7512=EDGE_LOOP('',(#27198,#27199,#27200,#27201));
#7513=EDGE_LOOP('',(#27202,#27203,#27204,#27205));
#7514=EDGE_LOOP('',(#27206,#27207,#27208,#27209));
#7515=EDGE_LOOP('',(#27210,#27211,#27212,#27213));
#7516=EDGE_LOOP('',(#27214,#27215,#27216,#27217));
#7517=EDGE_LOOP('',(#27218,#27219,#27220,#27221));
#7518=EDGE_LOOP('',(#27222,#27223,#27224,#27225));
#7519=EDGE_LOOP('',(#27226,#27227,#27228,#27229));
#7520=EDGE_LOOP('',(#27230,#27231,#27232,#27233));
#7521=EDGE_LOOP('',(#27234,#27235,#27236,#27237));
#7522=EDGE_LOOP('',(#27238,#27239,#27240,#27241));
#7523=EDGE_LOOP('',(#27242,#27243,#27244,#27245));
#7524=EDGE_LOOP('',(#27246,#27247,#27248,#27249));
#7525=EDGE_LOOP('',(#27250,#27251,#27252,#27253));
#7526=EDGE_LOOP('',(#27254,#27255,#27256,#27257));
#7527=EDGE_LOOP('',(#27258,#27259,#27260,#27261));
#7528=EDGE_LOOP('',(#27262,#27263,#27264,#27265));
#7529=EDGE_LOOP('',(#27266,#27267,#27268,#27269));
#7530=EDGE_LOOP('',(#27270,#27271,#27272,#27273));
#7531=EDGE_LOOP('',(#27274,#27275,#27276,#27277));
#7532=EDGE_LOOP('',(#27278,#27279,#27280,#27281));
#7533=EDGE_LOOP('',(#27282,#27283,#27284,#27285));
#7534=EDGE_LOOP('',(#27286,#27287,#27288,#27289));
#7535=EDGE_LOOP('',(#27290,#27291,#27292,#27293));
#7536=EDGE_LOOP('',(#27294,#27295,#27296,#27297));
#7537=EDGE_LOOP('',(#27298,#27299,#27300,#27301));
#7538=EDGE_LOOP('',(#27302,#27303,#27304,#27305));
#7539=EDGE_LOOP('',(#27306,#27307,#27308,#27309));
#7540=EDGE_LOOP('',(#27310,#27311,#27312,#27313));
#7541=EDGE_LOOP('',(#27314,#27315,#27316,#27317));
#7542=EDGE_LOOP('',(#27318,#27319,#27320,#27321));
#7543=EDGE_LOOP('',(#27322,#27323,#27324,#27325));
#7544=EDGE_LOOP('',(#27326,#27327,#27328,#27329));
#7545=EDGE_LOOP('',(#27330,#27331,#27332,#27333));
#7546=EDGE_LOOP('',(#27334,#27335,#27336,#27337));
#7547=EDGE_LOOP('',(#27338,#27339,#27340,#27341));
#7548=EDGE_LOOP('',(#27342,#27343,#27344,#27345));
#7549=EDGE_LOOP('',(#27346,#27347,#27348,#27349));
#7550=EDGE_LOOP('',(#27350,#27351,#27352,#27353));
#7551=EDGE_LOOP('',(#27354,#27355,#27356,#27357));
#7552=EDGE_LOOP('',(#27358,#27359,#27360,#27361));
#7553=EDGE_LOOP('',(#27362,#27363,#27364,#27365));
#7554=EDGE_LOOP('',(#27366,#27367,#27368,#27369));
#7555=EDGE_LOOP('',(#27370,#27371,#27372,#27373));
#7556=EDGE_LOOP('',(#27374,#27375,#27376,#27377));
#7557=EDGE_LOOP('',(#27378,#27379,#27380,#27381));
#7558=EDGE_LOOP('',(#27382,#27383,#27384,#27385));
#7559=EDGE_LOOP('',(#27386,#27387,#27388,#27389));
#7560=EDGE_LOOP('',(#27390,#27391,#27392,#27393));
#7561=EDGE_LOOP('',(#27394,#27395,#27396,#27397));
#7562=EDGE_LOOP('',(#27398,#27399,#27400,#27401));
#7563=EDGE_LOOP('',(#27402,#27403,#27404,#27405));
#7564=EDGE_LOOP('',(#27406,#27407,#27408,#27409));
#7565=EDGE_LOOP('',(#27410,#27411,#27412,#27413));
#7566=EDGE_LOOP('',(#27414,#27415,#27416,#27417));
#7567=EDGE_LOOP('',(#27418,#27419,#27420,#27421));
#7568=EDGE_LOOP('',(#27422,#27423,#27424,#27425));
#7569=EDGE_LOOP('',(#27426,#27427,#27428,#27429));
#7570=EDGE_LOOP('',(#27430,#27431,#27432,#27433));
#7571=EDGE_LOOP('',(#27434,#27435,#27436,#27437));
#7572=EDGE_LOOP('',(#27438,#27439,#27440,#27441));
#7573=EDGE_LOOP('',(#27442,#27443,#27444,#27445));
#7574=EDGE_LOOP('',(#27446,#27447,#27448,#27449));
#7575=EDGE_LOOP('',(#27450,#27451,#27452,#27453));
#7576=EDGE_LOOP('',(#27454,#27455,#27456,#27457));
#7577=EDGE_LOOP('',(#27458,#27459,#27460,#27461));
#7578=EDGE_LOOP('',(#27462,#27463,#27464,#27465));
#7579=EDGE_LOOP('',(#27466,#27467,#27468,#27469));
#7580=EDGE_LOOP('',(#27470,#27471,#27472,#27473));
#7581=EDGE_LOOP('',(#27474,#27475,#27476,#27477));
#7582=EDGE_LOOP('',(#27478,#27479,#27480,#27481));
#7583=EDGE_LOOP('',(#27482,#27483,#27484,#27485));
#7584=EDGE_LOOP('',(#27486,#27487,#27488,#27489));
#7585=EDGE_LOOP('',(#27490,#27491,#27492,#27493));
#7586=EDGE_LOOP('',(#27494,#27495,#27496,#27497));
#7587=EDGE_LOOP('',(#27498,#27499,#27500,#27501));
#7588=EDGE_LOOP('',(#27502,#27503,#27504,#27505));
#7589=EDGE_LOOP('',(#27506,#27507,#27508,#27509));
#7590=EDGE_LOOP('',(#27510,#27511,#27512,#27513));
#7591=EDGE_LOOP('',(#27514,#27515,#27516,#27517));
#7592=EDGE_LOOP('',(#27518,#27519,#27520,#27521));
#7593=EDGE_LOOP('',(#27522,#27523,#27524,#27525));
#7594=EDGE_LOOP('',(#27526,#27527,#27528,#27529));
#7595=EDGE_LOOP('',(#27530,#27531,#27532,#27533));
#7596=EDGE_LOOP('',(#27534,#27535,#27536,#27537));
#7597=EDGE_LOOP('',(#27538,#27539,#27540,#27541));
#7598=EDGE_LOOP('',(#27542,#27543,#27544,#27545));
#7599=EDGE_LOOP('',(#27546,#27547,#27548,#27549));
#7600=EDGE_LOOP('',(#27550,#27551,#27552,#27553));
#7601=EDGE_LOOP('',(#27554,#27555,#27556,#27557));
#7602=EDGE_LOOP('',(#27558,#27559,#27560,#27561));
#7603=EDGE_LOOP('',(#27562,#27563,#27564,#27565));
#7604=EDGE_LOOP('',(#27566,#27567,#27568,#27569));
#7605=EDGE_LOOP('',(#27570,#27571,#27572,#27573));
#7606=EDGE_LOOP('',(#27574,#27575,#27576,#27577,#27578,#27579,#27580,#27581,
#27582,#27583,#27584,#27585,#27586,#27587,#27588,#27589,#27590,#27591,#27592,
#27593,#27594,#27595,#27596,#27597,#27598,#27599,#27600,#27601,#27602,#27603,
#27604,#27605,#27606,#27607,#27608,#27609,#27610,#27611,#27612,#27613,#27614,
#27615,#27616,#27617,#27618,#27619,#27620,#27621,#27622,#27623,#27624,#27625,
#27626,#27627,#27628,#27629,#27630,#27631,#27632,#27633,#27634,#27635,#27636,
#27637,#27638,#27639,#27640,#27641,#27642,#27643,#27644,#27645,#27646,#27647,
#27648,#27649,#27650,#27651,#27652,#27653,#27654,#27655,#27656,#27657,#27658,
#27659,#27660,#27661,#27662,#27663,#27664,#27665,#27666,#27667,#27668,#27669,
#27670,#27671,#27672,#27673,#27674,#27675,#27676,#27677,#27678,#27679,#27680,
#27681,#27682,#27683,#27684,#27685,#27686,#27687,#27688,#27689,#27690,#27691,
#27692,#27693,#27694,#27695,#27696,#27697,#27698,#27699,#27700,#27701,#27702,
#27703,#27704,#27705,#27706,#27707,#27708,#27709,#27710,#27711,#27712,#27713,
#27714,#27715,#27716,#27717,#27718,#27719,#27720,#27721,#27722,#27723,#27724,
#27725,#27726,#27727,#27728,#27729,#27730,#27731,#27732,#27733,#27734,#27735,
#27736,#27737,#27738,#27739,#27740,#27741,#27742,#27743,#27744,#27745,#27746,
#27747,#27748,#27749,#27750,#27751,#27752,#27753,#27754,#27755,#27756,#27757,
#27758,#27759,#27760,#27761,#27762,#27763,#27764,#27765));
#7607=EDGE_LOOP('',(#27766,#27767,#27768,#27769));
#7608=EDGE_LOOP('',(#27770,#27771,#27772,#27773,#27774));
#7609=EDGE_LOOP('',(#27775,#27776,#27777,#27778,#27779));
#7610=EDGE_LOOP('',(#27780));
#7611=EDGE_LOOP('',(#27781,#27782,#27783,#27784));
#7612=EDGE_LOOP('',(#27785,#27786,#27787,#27788));
#7613=EDGE_LOOP('',(#27789,#27790,#27791,#27792,#27793,#27794,#27795,#27796,
#27797,#27798,#27799,#27800,#27801,#27802,#27803,#27804,#27805,#27806,#27807,
#27808,#27809,#27810,#27811,#27812,#27813,#27814,#27815,#27816,#27817,#27818,
#27819,#27820,#27821,#27822,#27823,#27824,#27825,#27826,#27827,#27828,#27829,
#27830,#27831,#27832,#27833,#27834,#27835,#27836,#27837,#27838,#27839,#27840,
#27841,#27842,#27843,#27844,#27845,#27846,#27847,#27848,#27849,#27850,#27851,
#27852,#27853,#27854,#27855,#27856,#27857,#27858,#27859,#27860,#27861,#27862,
#27863,#27864,#27865,#27866,#27867,#27868,#27869,#27870,#27871,#27872,#27873,
#27874,#27875,#27876,#27877,#27878,#27879,#27880,#27881,#27882,#27883,#27884,
#27885,#27886,#27887,#27888,#27889,#27890,#27891,#27892,#27893,#27894,#27895,
#27896,#27897,#27898,#27899,#27900,#27901,#27902,#27903,#27904,#27905,#27906,
#27907,#27908,#27909,#27910,#27911,#27912,#27913,#27914,#27915,#27916,#27917,
#27918,#27919,#27920,#27921,#27922,#27923,#27924,#27925,#27926,#27927,#27928,
#27929,#27930,#27931,#27932,#27933,#27934,#27935,#27936,#27937,#27938,#27939,
#27940,#27941,#27942,#27943,#27944,#27945,#27946,#27947,#27948));
#7614=EDGE_LOOP('',(#27949));
#7615=EDGE_LOOP('',(#27950,#27951,#27952,#27953));
#7616=EDGE_LOOP('',(#27954,#27955,#27956,#27957));
#7617=EDGE_LOOP('',(#27958,#27959,#27960,#27961));
#7618=EDGE_LOOP('',(#27962,#27963,#27964,#27965));
#7619=EDGE_LOOP('',(#27966,#27967,#27968,#27969));
#7620=EDGE_LOOP('',(#27970,#27971,#27972,#27973));
#7621=EDGE_LOOP('',(#27974,#27975,#27976,#27977));
#7622=EDGE_LOOP('',(#27978,#27979,#27980,#27981));
#7623=EDGE_LOOP('',(#27982,#27983,#27984,#27985));
#7624=EDGE_LOOP('',(#27986,#27987,#27988,#27989));
#7625=EDGE_LOOP('',(#27990,#27991,#27992,#27993));
#7626=EDGE_LOOP('',(#27994,#27995,#27996,#27997));
#7627=EDGE_LOOP('',(#27998,#27999,#28000,#28001));
#7628=EDGE_LOOP('',(#28002,#28003,#28004,#28005));
#7629=EDGE_LOOP('',(#28006,#28007,#28008,#28009));
#7630=EDGE_LOOP('',(#28010,#28011,#28012,#28013));
#7631=EDGE_LOOP('',(#28014,#28015,#28016,#28017));
#7632=EDGE_LOOP('',(#28018,#28019,#28020,#28021));
#7633=EDGE_LOOP('',(#28022,#28023,#28024,#28025));
#7634=EDGE_LOOP('',(#28026,#28027,#28028,#28029));
#7635=EDGE_LOOP('',(#28030,#28031,#28032,#28033));
#7636=EDGE_LOOP('',(#28034,#28035,#28036,#28037));
#7637=EDGE_LOOP('',(#28038,#28039,#28040,#28041));
#7638=EDGE_LOOP('',(#28042,#28043,#28044,#28045));
#7639=EDGE_LOOP('',(#28046,#28047,#28048,#28049));
#7640=EDGE_LOOP('',(#28050,#28051,#28052,#28053));
#7641=EDGE_LOOP('',(#28054,#28055,#28056,#28057));
#7642=EDGE_LOOP('',(#28058,#28059,#28060,#28061));
#7643=EDGE_LOOP('',(#28062,#28063,#28064,#28065));
#7644=EDGE_LOOP('',(#28066,#28067,#28068,#28069));
#7645=EDGE_LOOP('',(#28070,#28071,#28072,#28073));
#7646=EDGE_LOOP('',(#28074,#28075,#28076,#28077));
#7647=EDGE_LOOP('',(#28078,#28079,#28080,#28081));
#7648=EDGE_LOOP('',(#28082,#28083,#28084,#28085));
#7649=EDGE_LOOP('',(#28086,#28087,#28088,#28089));
#7650=EDGE_LOOP('',(#28090,#28091,#28092,#28093));
#7651=EDGE_LOOP('',(#28094,#28095,#28096,#28097));
#7652=EDGE_LOOP('',(#28098,#28099,#28100,#28101));
#7653=EDGE_LOOP('',(#28102,#28103,#28104,#28105));
#7654=EDGE_LOOP('',(#28106,#28107,#28108,#28109));
#7655=EDGE_LOOP('',(#28110,#28111,#28112,#28113));
#7656=EDGE_LOOP('',(#28114,#28115,#28116,#28117));
#7657=EDGE_LOOP('',(#28118,#28119,#28120,#28121));
#7658=EDGE_LOOP('',(#28122,#28123,#28124,#28125));
#7659=EDGE_LOOP('',(#28126,#28127,#28128,#28129));
#7660=EDGE_LOOP('',(#28130,#28131,#28132,#28133));
#7661=EDGE_LOOP('',(#28134,#28135,#28136,#28137));
#7662=EDGE_LOOP('',(#28138,#28139,#28140,#28141));
#7663=EDGE_LOOP('',(#28142,#28143,#28144,#28145));
#7664=EDGE_LOOP('',(#28146,#28147,#28148,#28149));
#7665=EDGE_LOOP('',(#28150,#28151,#28152,#28153));
#7666=EDGE_LOOP('',(#28154,#28155,#28156,#28157));
#7667=EDGE_LOOP('',(#28158,#28159,#28160,#28161));
#7668=EDGE_LOOP('',(#28162,#28163,#28164,#28165));
#7669=EDGE_LOOP('',(#28166,#28167,#28168,#28169));
#7670=EDGE_LOOP('',(#28170,#28171,#28172,#28173));
#7671=EDGE_LOOP('',(#28174,#28175,#28176,#28177));
#7672=EDGE_LOOP('',(#28178,#28179,#28180,#28181));
#7673=EDGE_LOOP('',(#28182,#28183,#28184,#28185));
#7674=EDGE_LOOP('',(#28186,#28187,#28188,#28189));
#7675=EDGE_LOOP('',(#28190,#28191,#28192,#28193));
#7676=EDGE_LOOP('',(#28194,#28195,#28196,#28197));
#7677=EDGE_LOOP('',(#28198,#28199,#28200,#28201));
#7678=EDGE_LOOP('',(#28202,#28203,#28204,#28205));
#7679=EDGE_LOOP('',(#28206,#28207,#28208,#28209));
#7680=EDGE_LOOP('',(#28210,#28211,#28212,#28213));
#7681=EDGE_LOOP('',(#28214,#28215,#28216,#28217));
#7682=EDGE_LOOP('',(#28218,#28219,#28220,#28221));
#7683=EDGE_LOOP('',(#28222,#28223,#28224,#28225));
#7684=EDGE_LOOP('',(#28226,#28227,#28228,#28229));
#7685=EDGE_LOOP('',(#28230,#28231,#28232,#28233));
#7686=EDGE_LOOP('',(#28234,#28235,#28236,#28237));
#7687=EDGE_LOOP('',(#28238,#28239,#28240,#28241));
#7688=EDGE_LOOP('',(#28242,#28243,#28244,#28245));
#7689=EDGE_LOOP('',(#28246,#28247,#28248,#28249));
#7690=EDGE_LOOP('',(#28250,#28251,#28252,#28253));
#7691=EDGE_LOOP('',(#28254,#28255,#28256,#28257));
#7692=EDGE_LOOP('',(#28258,#28259,#28260,#28261));
#7693=EDGE_LOOP('',(#28262,#28263,#28264,#28265));
#7694=EDGE_LOOP('',(#28266,#28267,#28268,#28269));
#7695=EDGE_LOOP('',(#28270,#28271,#28272,#28273));
#7696=EDGE_LOOP('',(#28274,#28275,#28276,#28277));
#7697=EDGE_LOOP('',(#28278,#28279,#28280,#28281));
#7698=EDGE_LOOP('',(#28282,#28283,#28284,#28285));
#7699=EDGE_LOOP('',(#28286,#28287,#28288,#28289));
#7700=EDGE_LOOP('',(#28290,#28291,#28292,#28293));
#7701=EDGE_LOOP('',(#28294,#28295,#28296,#28297));
#7702=EDGE_LOOP('',(#28298,#28299,#28300,#28301));
#7703=EDGE_LOOP('',(#28302,#28303,#28304,#28305));
#7704=EDGE_LOOP('',(#28306,#28307,#28308,#28309));
#7705=EDGE_LOOP('',(#28310,#28311,#28312,#28313));
#7706=EDGE_LOOP('',(#28314,#28315,#28316,#28317));
#7707=EDGE_LOOP('',(#28318,#28319,#28320,#28321));
#7708=EDGE_LOOP('',(#28322,#28323,#28324,#28325));
#7709=EDGE_LOOP('',(#28326,#28327,#28328,#28329));
#7710=EDGE_LOOP('',(#28330,#28331,#28332,#28333));
#7711=EDGE_LOOP('',(#28334,#28335,#28336,#28337));
#7712=EDGE_LOOP('',(#28338,#28339,#28340,#28341));
#7713=EDGE_LOOP('',(#28342,#28343,#28344,#28345));
#7714=EDGE_LOOP('',(#28346,#28347,#28348,#28349));
#7715=EDGE_LOOP('',(#28350,#28351,#28352,#28353));
#7716=EDGE_LOOP('',(#28354,#28355,#28356,#28357));
#7717=EDGE_LOOP('',(#28358,#28359,#28360,#28361));
#7718=EDGE_LOOP('',(#28362,#28363,#28364,#28365));
#7719=EDGE_LOOP('',(#28366,#28367,#28368,#28369));
#7720=EDGE_LOOP('',(#28370,#28371,#28372,#28373));
#7721=EDGE_LOOP('',(#28374,#28375,#28376,#28377));
#7722=EDGE_LOOP('',(#28378,#28379,#28380,#28381));
#7723=EDGE_LOOP('',(#28382,#28383,#28384,#28385));
#7724=EDGE_LOOP('',(#28386,#28387,#28388,#28389));
#7725=EDGE_LOOP('',(#28390,#28391,#28392,#28393));
#7726=EDGE_LOOP('',(#28394,#28395,#28396,#28397));
#7727=EDGE_LOOP('',(#28398,#28399,#28400,#28401));
#7728=EDGE_LOOP('',(#28402,#28403,#28404,#28405));
#7729=EDGE_LOOP('',(#28406,#28407,#28408,#28409));
#7730=EDGE_LOOP('',(#28410,#28411,#28412,#28413));
#7731=EDGE_LOOP('',(#28414,#28415,#28416,#28417));
#7732=EDGE_LOOP('',(#28418,#28419,#28420,#28421));
#7733=EDGE_LOOP('',(#28422,#28423,#28424,#28425));
#7734=EDGE_LOOP('',(#28426,#28427,#28428,#28429));
#7735=EDGE_LOOP('',(#28430,#28431,#28432,#28433));
#7736=EDGE_LOOP('',(#28434,#28435,#28436,#28437));
#7737=EDGE_LOOP('',(#28438,#28439,#28440,#28441));
#7738=EDGE_LOOP('',(#28442,#28443,#28444,#28445));
#7739=EDGE_LOOP('',(#28446,#28447,#28448,#28449));
#7740=EDGE_LOOP('',(#28450,#28451,#28452,#28453));
#7741=EDGE_LOOP('',(#28454,#28455,#28456,#28457));
#7742=EDGE_LOOP('',(#28458,#28459,#28460,#28461));
#7743=EDGE_LOOP('',(#28462,#28463,#28464,#28465));
#7744=EDGE_LOOP('',(#28466,#28467,#28468,#28469));
#7745=EDGE_LOOP('',(#28470,#28471,#28472,#28473));
#7746=EDGE_LOOP('',(#28474,#28475,#28476,#28477));
#7747=EDGE_LOOP('',(#28478,#28479,#28480,#28481));
#7748=EDGE_LOOP('',(#28482,#28483,#28484,#28485));
#7749=EDGE_LOOP('',(#28486,#28487,#28488,#28489));
#7750=EDGE_LOOP('',(#28490,#28491,#28492,#28493));
#7751=EDGE_LOOP('',(#28494,#28495,#28496,#28497));
#7752=EDGE_LOOP('',(#28498,#28499,#28500,#28501));
#7753=EDGE_LOOP('',(#28502,#28503,#28504,#28505));
#7754=EDGE_LOOP('',(#28506,#28507,#28508,#28509));
#7755=EDGE_LOOP('',(#28510,#28511,#28512,#28513));
#7756=EDGE_LOOP('',(#28514,#28515,#28516,#28517));
#7757=EDGE_LOOP('',(#28518,#28519,#28520,#28521));
#7758=EDGE_LOOP('',(#28522,#28523,#28524,#28525));
#7759=EDGE_LOOP('',(#28526,#28527,#28528,#28529));
#7760=EDGE_LOOP('',(#28530,#28531,#28532,#28533));
#7761=EDGE_LOOP('',(#28534,#28535,#28536,#28537));
#7762=EDGE_LOOP('',(#28538,#28539,#28540,#28541));
#7763=EDGE_LOOP('',(#28542,#28543,#28544,#28545));
#7764=EDGE_LOOP('',(#28546,#28547,#28548,#28549));
#7765=EDGE_LOOP('',(#28550,#28551,#28552,#28553));
#7766=EDGE_LOOP('',(#28554,#28555,#28556,#28557));
#7767=EDGE_LOOP('',(#28558,#28559,#28560,#28561));
#7768=EDGE_LOOP('',(#28562,#28563,#28564,#28565));
#7769=EDGE_LOOP('',(#28566,#28567,#28568,#28569));
#7770=EDGE_LOOP('',(#28570,#28571,#28572,#28573));
#7771=EDGE_LOOP('',(#28574,#28575,#28576,#28577));
#7772=EDGE_LOOP('',(#28578,#28579,#28580,#28581));
#7773=EDGE_LOOP('',(#28582,#28583,#28584,#28585));
#7774=EDGE_LOOP('',(#28586,#28587,#28588,#28589));
#7775=EDGE_LOOP('',(#28590,#28591,#28592,#28593));
#7776=EDGE_LOOP('',(#28594,#28595,#28596,#28597));
#7777=EDGE_LOOP('',(#28598,#28599,#28600,#28601));
#7778=EDGE_LOOP('',(#28602,#28603,#28604,#28605));
#7779=EDGE_LOOP('',(#28606,#28607,#28608,#28609,#28610,#28611,#28612,#28613,
#28614,#28615,#28616,#28617,#28618,#28619,#28620,#28621,#28622,#28623,#28624,
#28625,#28626,#28627,#28628,#28629,#28630,#28631,#28632,#28633,#28634,#28635,
#28636,#28637,#28638,#28639,#28640,#28641,#28642,#28643,#28644,#28645,#28646,
#28647,#28648,#28649,#28650,#28651,#28652,#28653,#28654,#28655,#28656,#28657,
#28658,#28659,#28660,#28661,#28662,#28663,#28664,#28665,#28666,#28667,#28668,
#28669,#28670,#28671,#28672,#28673,#28674,#28675,#28676,#28677,#28678,#28679,
#28680,#28681,#28682,#28683,#28684,#28685,#28686,#28687,#28688,#28689,#28690,
#28691,#28692,#28693,#28694,#28695,#28696,#28697,#28698,#28699,#28700,#28701,
#28702,#28703,#28704,#28705,#28706,#28707,#28708,#28709,#28710,#28711,#28712,
#28713,#28714,#28715,#28716,#28717,#28718,#28719,#28720,#28721,#28722,#28723,
#28724,#28725,#28726,#28727,#28728,#28729,#28730,#28731,#28732,#28733,#28734,
#28735,#28736,#28737,#28738,#28739,#28740,#28741,#28742,#28743,#28744,#28745,
#28746,#28747,#28748,#28749,#28750,#28751,#28752,#28753,#28754,#28755,#28756,
#28757,#28758,#28759,#28760,#28761,#28762,#28763,#28764,#28765));
#7780=EDGE_LOOP('',(#28766,#28767,#28768,#28769));
#7781=EDGE_LOOP('',(#28770,#28771,#28772,#28773,#28774));
#7782=EDGE_LOOP('',(#28775));
#7783=EDGE_LOOP('',(#28776,#28777,#28778,#28779));
#7784=EDGE_LOOP('',(#28780,#28781,#28782,#28783,#28784,#28785));
#7785=EDGE_LOOP('',(#28786,#28787,#28788,#28789));
#7786=EDGE_LOOP('',(#28790));
#7787=EDGE_LOOP('',(#28791));
#7788=EDGE_LOOP('',(#28792));
#7789=EDGE_LOOP('',(#28793));
#7790=EDGE_LOOP('',(#28794,#28795,#28796,#28797));
#7791=EDGE_LOOP('',(#28798,#28799,#28800,#28801,#28802));
#7792=EDGE_LOOP('',(#28803));
#7793=EDGE_LOOP('',(#28804,#28805,#28806,#28807));
#7794=EDGE_LOOP('',(#28808,#28809,#28810,#28811,#28812,#28813));
#7795=EDGE_LOOP('',(#28814,#28815,#28816,#28817));
#7796=EDGE_LOOP('',(#28818));
#7797=EDGE_LOOP('',(#28819));
#7798=EDGE_LOOP('',(#28820));
#7799=EDGE_LOOP('',(#28821));
#7800=EDGE_LOOP('',(#28822,#28823,#28824,#28825));
#7801=EDGE_LOOP('',(#28826,#28827,#28828,#28829,#28830));
#7802=EDGE_LOOP('',(#28831));
#7803=EDGE_LOOP('',(#28832,#28833,#28834,#28835,#28836,#28837));
#7804=EDGE_LOOP('',(#28838,#28839,#28840,#28841));
#7805=EDGE_LOOP('',(#28842,#28843,#28844,#28845));
#7806=EDGE_LOOP('',(#28846));
#7807=EDGE_LOOP('',(#28847));
#7808=EDGE_LOOP('',(#28848,#28849,#28850,#28851));
#7809=EDGE_LOOP('',(#28852));
#7810=EDGE_LOOP('',(#28853));
#7811=EDGE_LOOP('',(#28854,#28855,#28856,#28857));
#7812=EDGE_LOOP('',(#28858));
#7813=EDGE_LOOP('',(#28859));
#7814=EDGE_LOOP('',(#28860,#28861,#28862,#28863));
#7815=EDGE_LOOP('',(#28864));
#7816=EDGE_LOOP('',(#28865));
#7817=EDGE_LOOP('',(#28866,#28867,#28868,#28869,#28870));
#7818=EDGE_LOOP('',(#28871));
#7819=EDGE_LOOP('',(#28872,#28873,#28874,#28875,#28876,#28877));
#7820=EDGE_LOOP('',(#28878,#28879,#28880,#28881));
#7821=EDGE_LOOP('',(#28882,#28883,#28884,#28885));
#7822=EDGE_LOOP('',(#28886));
#7823=EDGE_LOOP('',(#28887));
#7824=EDGE_LOOP('',(#28888,#28889,#28890,#28891));
#7825=EDGE_LOOP('',(#28892));
#7826=EDGE_LOOP('',(#28893));
#7827=EDGE_LOOP('',(#28894,#28895,#28896,#28897,#28898));
#7828=EDGE_LOOP('',(#28899));
#7829=EDGE_LOOP('',(#28900,#28901,#28902,#28903,#28904,#28905));
#7830=EDGE_LOOP('',(#28906,#28907,#28908,#28909));
#7831=EDGE_LOOP('',(#28910,#28911,#28912,#28913,#28914,#28915,#28916,#28917,
#28918,#28919,#28920,#28921,#28922,#28923,#28924,#28925));
#7832=EDGE_LOOP('',(#28926,#28927,#28928,#28929));
#7833=EDGE_LOOP('',(#28930,#28931,#28932,#28933));
#7834=EDGE_LOOP('',(#28934,#28935,#28936,#28937));
#7835=EDGE_LOOP('',(#28938,#28939,#28940,#28941,#28942,#28943));
#7836=EDGE_LOOP('',(#28944,#28945,#28946,#28947,#28948,#28949));
#7837=EDGE_LOOP('',(#28950,#28951,#28952,#28953,#28954,#28955,#28956,#28957));
#7838=EDGE_LOOP('',(#28958,#28959,#28960,#28961,#28962,#28963,#28964,#28965));
#7839=EDGE_LOOP('',(#28966,#28967,#28968,#28969));
#7840=EDGE_LOOP('',(#28970,#28971,#28972,#28973,#28974,#28975,#28976,#28977,
#28978,#28979,#28980,#28981,#28982,#28983,#28984,#28985));
#7841=EDGE_LOOP('',(#28986));
#7842=EDGE_LOOP('',(#28987,#28988,#28989,#28990,#28991));
#7843=EDGE_LOOP('',(#28992,#28993,#28994,#28995));
#7844=EDGE_LOOP('',(#28996,#28997,#28998,#28999,#29000,#29001,#29002,#29003,
#29004));
#7845=EDGE_LOOP('',(#29005));
#7846=EDGE_LOOP('',(#29006));
#7847=EDGE_LOOP('',(#29007));
#7848=EDGE_LOOP('',(#29008));
#7849=EDGE_LOOP('',(#29009,#29010,#29011,#29012,#29013));
#7850=EDGE_LOOP('',(#29014,#29015,#29016,#29017));
#7851=EDGE_LOOP('',(#29018,#29019,#29020,#29021,#29022,#29023,#29024,#29025,
#29026,#29027,#29028));
#7852=EDGE_LOOP('',(#29029,#29030,#29031,#29032,#29033));
#7853=EDGE_LOOP('',(#29034,#29035,#29036,#29037));
#7854=EDGE_LOOP('',(#29038,#29039,#29040,#29041));
#7855=EDGE_LOOP('',(#29042,#29043,#29044,#29045,#29046));
#7856=EDGE_LOOP('',(#29047,#29048,#29049,#29050,#29051,#29052,#29053,#29054,
#29055,#29056,#29057));
#7857=EDGE_LOOP('',(#29058,#29059,#29060,#29061,#29062,#29063,#29064,#29065,
#29066,#29067,#29068,#29069,#29070,#29071,#29072,#29073,#29074,#29075));
#7858=EDGE_LOOP('',(#29076,#29077,#29078,#29079,#29080,#29081,#29082,#29083,
#29084,#29085));
#7859=EDGE_LOOP('',(#29086,#29087,#29088,#29089,#29090,#29091,#29092,#29093,
#29094));
#7860=EDGE_LOOP('',(#29095,#29096,#29097));
#7861=EDGE_LOOP('',(#29098,#29099,#29100));
#7862=EDGE_LOOP('',(#29101,#29102,#29103,#29104));
#7863=EDGE_LOOP('',(#29105,#29106,#29107,#29108));
#7864=EDGE_LOOP('',(#29109,#29110,#29111,#29112));
#7865=EDGE_LOOP('',(#29113,#29114,#29115));
#7866=EDGE_LOOP('',(#29116,#29117,#29118,#29119,#29120));
#7867=EDGE_LOOP('',(#29121,#29122));
#7868=EDGE_LOOP('',(#29123));
#7869=EDGE_LOOP('',(#29124,#29125,#29126,#29127,#29128));
#7870=EDGE_LOOP('',(#29129,#29130,#29131,#29132,#29133));
#7871=EDGE_LOOP('',(#29134,#29135,#29136,#29137,#29138));
#7872=EDGE_LOOP('',(#29139,#29140,#29141,#29142,#29143));
#7873=EDGE_LOOP('',(#29144,#29145,#29146,#29147,#29148,#29149,#29150));
#7874=EDGE_LOOP('',(#29151,#29152,#29153,#29154,#29155,#29156));
#7875=EDGE_LOOP('',(#29157,#29158,#29159,#29160,#29161,#29162));
#7876=EDGE_LOOP('',(#29163,#29164,#29165));
#7877=EDGE_LOOP('',(#29166,#29167,#29168,#29169,#29170,#29171));
#7878=EDGE_LOOP('',(#29172,#29173,#29174,#29175));
#7879=EDGE_LOOP('',(#29176,#29177,#29178,#29179));
#7880=EDGE_LOOP('',(#29180));
#7881=EDGE_LOOP('',(#29181,#29182,#29183,#29184,#29185,#29186));
#7882=EDGE_LOOP('',(#29187,#29188,#29189,#29190,#29191,#29192));
#7883=EDGE_LOOP('',(#29193,#29194,#29195,#29196,#29197,#29198));
#7884=EDGE_LOOP('',(#29199,#29200,#29201,#29202,#29203,#29204));
#7885=EDGE_LOOP('',(#29205,#29206,#29207));
#7886=EDGE_LOOP('',(#29208,#29209,#29210));
#7887=EDGE_LOOP('',(#29211,#29212,#29213));
#7888=EDGE_LOOP('',(#29214,#29215,#29216));
#7889=EDGE_LOOP('',(#29217,#29218,#29219));
#7890=EDGE_LOOP('',(#29220,#29221,#29222,#29223,#29224,#29225));
#7891=EDGE_LOOP('',(#29226,#29227,#29228,#29229,#29230,#29231));
#7892=EDGE_LOOP('',(#29232,#29233,#29234));
#7893=EDGE_LOOP('',(#29235,#29236,#29237,#29238,#29239,#29240,#29241,#29242,
#29243,#29244,#29245,#29246));
#7894=EDGE_LOOP('',(#29247,#29248,#29249,#29250,#29251,#29252));
#7895=EDGE_LOOP('',(#29253,#29254,#29255,#29256,#29257,#29258));
#7896=EDGE_LOOP('',(#29259,#29260,#29261,#29262,#29263,#29264));
#7897=EDGE_LOOP('',(#29265,#29266,#29267,#29268,#29269,#29270));
#7898=EDGE_LOOP('',(#29271,#29272,#29273));
#7899=EDGE_LOOP('',(#29274,#29275,#29276));
#7900=EDGE_LOOP('',(#29277,#29278,#29279));
#7901=EDGE_LOOP('',(#29280,#29281,#29282));
#7902=EDGE_LOOP('',(#29283,#29284,#29285));
#7903=EDGE_LOOP('',(#29286,#29287,#29288,#29289,#29290,#29291));
#7904=EDGE_LOOP('',(#29292,#29293,#29294,#29295,#29296,#29297));
#7905=EDGE_LOOP('',(#29298,#29299,#29300));
#7906=EDGE_LOOP('',(#29301,#29302,#29303,#29304,#29305,#29306,#29307,#29308,
#29309,#29310,#29311,#29312));
#7907=EDGE_LOOP('',(#29313,#29314,#29315,#29316,#29317));
#7908=EDGE_LOOP('',(#29318,#29319,#29320,#29321));
#7909=EDGE_LOOP('',(#29322,#29323,#29324,#29325));
#7910=EDGE_LOOP('',(#29326,#29327,#29328,#29329));
#7911=EDGE_LOOP('',(#29330,#29331,#29332,#29333));
#7912=EDGE_LOOP('',(#29334,#29335,#29336,#29337));
#7913=EDGE_LOOP('',(#29338,#29339,#29340,#29341));
#7914=EDGE_LOOP('',(#29342,#29343,#29344,#29345));
#7915=EDGE_LOOP('',(#29346,#29347,#29348,#29349));
#7916=EDGE_LOOP('',(#29350,#29351,#29352,#29353));
#7917=EDGE_LOOP('',(#29354,#29355));
#7918=EDGE_LOOP('',(#29356,#29357));
#7919=EDGE_LOOP('',(#29358,#29359,#29360,#29361,#29362,#29363));
#7920=EDGE_LOOP('',(#29364,#29365,#29366,#29367));
#7921=EDGE_LOOP('',(#29368,#29369,#29370,#29371));
#7922=EDGE_LOOP('',(#29372,#29373,#29374,#29375));
#7923=EDGE_LOOP('',(#29376,#29377,#29378,#29379));
#7924=EDGE_LOOP('',(#29380,#29381,#29382,#29383));
#7925=EDGE_LOOP('',(#29384,#29385,#29386,#29387));
#7926=EDGE_LOOP('',(#29388,#29389));
#7927=EDGE_LOOP('',(#29390,#29391));
#7928=EDGE_LOOP('',(#29392,#29393,#29394,#29395,#29396,#29397));
#7929=EDGE_LOOP('',(#29398,#29399,#29400,#29401,#29402,#29403));
#7930=EDGE_LOOP('',(#29404,#29405,#29406,#29407));
#7931=EDGE_LOOP('',(#29408,#29409,#29410,#29411));
#7932=EDGE_LOOP('',(#29412,#29413,#29414,#29415));
#7933=EDGE_LOOP('',(#29416,#29417,#29418,#29419));
#7934=EDGE_LOOP('',(#29420,#29421,#29422,#29423));
#7935=EDGE_LOOP('',(#29424,#29425,#29426,#29427));
#7936=EDGE_LOOP('',(#29428,#29429));
#7937=EDGE_LOOP('',(#29430,#29431));
#7938=EDGE_LOOP('',(#29432,#29433,#29434,#29435,#29436,#29437));
#7939=EDGE_LOOP('',(#29438,#29439,#29440,#29441));
#7940=EDGE_LOOP('',(#29442,#29443,#29444,#29445));
#7941=EDGE_LOOP('',(#29446,#29447,#29448,#29449));
#7942=EDGE_LOOP('',(#29450));
#7943=EDGE_LOOP('',(#29451,#29452,#29453,#29454,#29455,#29456));
#7944=EDGE_LOOP('',(#29457,#29458,#29459,#29460,#29461,#29462));
#7945=EDGE_LOOP('',(#29463,#29464,#29465,#29466));
#7946=EDGE_LOOP('',(#29467,#29468,#29469,#29470,#29471,#29472));
#7947=EDGE_LOOP('',(#29473,#29474,#29475,#29476,#29477));
#7948=EDGE_LOOP('',(#29478,#29479,#29480,#29481));
#7949=EDGE_LOOP('',(#29482,#29483,#29484,#29485,#29486,#29487));
#7950=EDGE_LOOP('',(#29488,#29489,#29490,#29491,#29492));
#7951=EDGE_LOOP('',(#29493,#29494,#29495,#29496));
#7952=EDGE_LOOP('',(#29497,#29498,#29499,#29500,#29501,#29502));
#7953=EDGE_LOOP('',(#29503,#29504,#29505,#29506,#29507));
#7954=EDGE_LOOP('',(#29508,#29509,#29510,#29511,#29512));
#7955=EDGE_LOOP('',(#29513,#29514,#29515,#29516,#29517,#29518));
#7956=EDGE_LOOP('',(#29519,#29520,#29521,#29522));
#7957=EDGE_LOOP('',(#29523,#29524,#29525,#29526,#29527));
#7958=EDGE_LOOP('',(#29528,#29529,#29530,#29531,#29532,#29533));
#7959=EDGE_LOOP('',(#29534,#29535,#29536,#29537));
#7960=EDGE_LOOP('',(#29538,#29539,#29540,#29541,#29542));
#7961=EDGE_LOOP('',(#29543,#29544,#29545,#29546,#29547,#29548));
#7962=EDGE_LOOP('',(#29549,#29550,#29551,#29552));
#7963=EDGE_LOOP('',(#29553,#29554,#29555,#29556,#29557));
#7964=EDGE_LOOP('',(#29558,#29559,#29560,#29561,#29562,#29563));
#7965=EDGE_LOOP('',(#29564,#29565,#29566,#29567));
#7966=EDGE_LOOP('',(#29568,#29569,#29570,#29571));
#7967=EDGE_LOOP('',(#29572,#29573,#29574,#29575));
#7968=EDGE_LOOP('',(#29576,#29577,#29578,#29579));
#7969=EDGE_LOOP('',(#29580,#29581,#29582,#29583));
#7970=EDGE_LOOP('',(#29584,#29585,#29586,#29587));
#7971=EDGE_LOOP('',(#29588,#29589,#29590,#29591));
#7972=EDGE_LOOP('',(#29592,#29593,#29594,#29595));
#7973=EDGE_LOOP('',(#29596,#29597,#29598,#29599));
#7974=EDGE_LOOP('',(#29600,#29601,#29602,#29603));
#7975=EDGE_LOOP('',(#29604,#29605,#29606,#29607));
#7976=EDGE_LOOP('',(#29608,#29609,#29610,#29611));
#7977=EDGE_LOOP('',(#29612,#29613,#29614,#29615));
#7978=EDGE_LOOP('',(#29616,#29617,#29618,#29619));
#7979=EDGE_LOOP('',(#29620,#29621,#29622,#29623,#29624));
#7980=EDGE_LOOP('',(#29625,#29626,#29627,#29628));
#7981=EDGE_LOOP('',(#29629,#29630,#29631,#29632));
#7982=EDGE_LOOP('',(#29633,#29634,#29635,#29636,#29637,#29638,#29639,#29640,
#29641,#29642));
#7983=EDGE_LOOP('',(#29643,#29644,#29645,#29646,#29647,#29648,#29649,#29650));
#7984=EDGE_LOOP('',(#29651));
#7985=EDGE_LOOP('',(#29652));
#7986=EDGE_LOOP('',(#29653,#29654,#29655,#29656));
#7987=EDGE_LOOP('',(#29657,#29658,#29659,#29660,#29661));
#7988=EDGE_LOOP('',(#29662,#29663,#29664,#29665,#29666,#29667,#29668,#29669,
#29670,#29671,#29672,#29673,#29674,#29675,#29676,#29677));
#7989=EDGE_LOOP('',(#29678));
#7990=EDGE_LOOP('',(#29679));
#7991=EDGE_LOOP('',(#29680));
#7992=EDGE_LOOP('',(#29681));
#7993=EDGE_LOOP('',(#29682,#29683,#29684,#29685,#29686));
#7994=EDGE_LOOP('',(#29687,#29688,#29689,#29690));
#7995=EDGE_LOOP('',(#29691,#29692,#29693,#29694));
#7996=EDGE_LOOP('',(#29695,#29696,#29697,#29698));
#7997=EDGE_LOOP('',(#29699,#29700,#29701,#29702));
#7998=EDGE_LOOP('',(#29703,#29704,#29705,#29706));
#7999=EDGE_LOOP('',(#29707,#29708,#29709,#29710));
#8000=EDGE_LOOP('',(#29711,#29712,#29713,#29714,#29715,#29716,#29717,#29718));
#8001=EDGE_LOOP('',(#29719));
#8002=EDGE_LOOP('',(#29720));
#8003=EDGE_LOOP('',(#29721));
#8004=EDGE_LOOP('',(#29722));
#8005=EDGE_LOOP('',(#29723));
#8006=EDGE_LOOP('',(#29724,#29725,#29726,#29727,#29728));
#8007=EDGE_LOOP('',(#29729,#29730,#29731,#29732));
#8008=EDGE_LOOP('',(#29733,#29734,#29735,#29736));
#8009=EDGE_LOOP('',(#29737,#29738,#29739,#29740,#29741));
#8010=EDGE_LOOP('',(#29742,#29743,#29744,#29745,#29746,#29747));
#8011=EDGE_LOOP('',(#29748,#29749,#29750,#29751,#29752));
#8012=EDGE_LOOP('',(#29753,#29754,#29755,#29756,#29757,#29758,#29759,#29760,
#29761,#29762));
#8013=EDGE_LOOP('',(#29763,#29764,#29765,#29766,#29767));
#8014=EDGE_LOOP('',(#29768,#29769,#29770,#29771,#29772));
#8015=EDGE_LOOP('',(#29773,#29774,#29775,#29776));
#8016=EDGE_LOOP('',(#29777,#29778,#29779,#29780,#29781));
#8017=EDGE_LOOP('',(#29782,#29783,#29784,#29785,#29786,#29787,#29788,#29789));
#8018=EDGE_LOOP('',(#29790,#29791,#29792,#29793,#29794,#29795));
#8019=EDGE_LOOP('',(#29796,#29797,#29798,#29799,#29800,#29801));
#8020=EDGE_LOOP('',(#29802,#29803,#29804,#29805,#29806,#29807));
#8021=EDGE_LOOP('',(#29808,#29809,#29810,#29811,#29812,#29813));
#8022=EDGE_LOOP('',(#29814));
#8023=EDGE_LOOP('',(#29815));
#8024=EDGE_LOOP('',(#29816));
#8025=EDGE_LOOP('',(#29817,#29818,#29819,#29820));
#8026=EDGE_LOOP('',(#29821));
#8027=EDGE_LOOP('',(#29822));
#8028=EDGE_LOOP('',(#29823,#29824,#29825,#29826,#29827));
#8029=EDGE_LOOP('',(#29828,#29829,#29830,#29831,#29832));
#8030=EDGE_LOOP('',(#29833));
#8031=EDGE_LOOP('',(#29834,#29835,#29836,#29837));
#8032=EDGE_LOOP('',(#29838,#29839,#29840,#29841));
#8033=EDGE_LOOP('',(#29842));
#8034=EDGE_LOOP('',(#29843));
#8035=EDGE_LOOP('',(#29844,#29845,#29846,#29847));
#8036=EDGE_LOOP('',(#29848));
#8037=EDGE_LOOP('',(#29849));
#8038=EDGE_LOOP('',(#29850,#29851,#29852,#29853,#29854));
#8039=EDGE_LOOP('',(#29855,#29856,#29857,#29858));
#8040=EDGE_LOOP('',(#29859));
#8041=EDGE_LOOP('',(#29860));
#8042=EDGE_LOOP('',(#29861,#29862,#29863,#29864,#29865,#29866));
#8043=EDGE_LOOP('',(#29867,#29868,#29869,#29870));
#8044=EDGE_LOOP('',(#29871,#29872,#29873,#29874));
#8045=EDGE_LOOP('',(#29875,#29876,#29877,#29878));
#8046=EDGE_LOOP('',(#29879,#29880,#29881,#29882));
#8047=EDGE_LOOP('',(#29883,#29884,#29885,#29886));
#8048=EDGE_LOOP('',(#29887,#29888,#29889,#29890));
#8049=EDGE_LOOP('',(#29891,#29892,#29893,#29894,#29895,#29896));
#8050=EDGE_LOOP('',(#29897,#29898,#29899,#29900));
#8051=EDGE_LOOP('',(#29901,#29902,#29903,#29904));
#8052=EDGE_LOOP('',(#29905,#29906,#29907,#29908));
#8053=EDGE_LOOP('',(#29909,#29910,#29911,#29912));
#8054=EDGE_LOOP('',(#29913,#29914,#29915,#29916));
#8055=EDGE_LOOP('',(#29917,#29918,#29919,#29920));
#8056=EDGE_LOOP('',(#29921));
#8057=EDGE_LOOP('',(#29922,#29923,#29924,#29925,#29926,#29927));
#8058=EDGE_LOOP('',(#29928,#29929,#29930,#29931,#29932));
#8059=EDGE_LOOP('',(#29933,#29934,#29935,#29936,#29937));
#8060=EDGE_LOOP('',(#29938,#29939,#29940,#29941,#29942));
#8061=EDGE_LOOP('',(#29943));
#8062=EDGE_LOOP('',(#29944));
#8063=EDGE_LOOP('',(#29945,#29946,#29947,#29948,#29949,#29950));
#8064=EDGE_LOOP('',(#29951,#29952,#29953,#29954,#29955));
#8065=EDGE_LOOP('',(#29956,#29957,#29958,#29959,#29960,#29961));
#8066=EDGE_LOOP('',(#29962,#29963,#29964,#29965));
#8067=EDGE_LOOP('',(#29966,#29967,#29968,#29969));
#8068=EDGE_LOOP('',(#29970,#29971,#29972,#29973));
#8069=EDGE_LOOP('',(#29974,#29975,#29976,#29977));
#8070=EDGE_LOOP('',(#29978,#29979,#29980,#29981));
#8071=EDGE_LOOP('',(#29982,#29983,#29984,#29985));
#8072=EDGE_LOOP('',(#29986,#29987,#29988,#29989,#29990,#29991));
#8073=EDGE_LOOP('',(#29992,#29993,#29994,#29995));
#8074=EDGE_LOOP('',(#29996,#29997,#29998,#29999));
#8075=EDGE_LOOP('',(#30000,#30001,#30002,#30003));
#8076=EDGE_LOOP('',(#30004,#30005,#30006,#30007));
#8077=EDGE_LOOP('',(#30008,#30009,#30010,#30011));
#8078=EDGE_LOOP('',(#30012,#30013,#30014,#30015));
#8079=EDGE_LOOP('',(#30016));
#8080=EDGE_LOOP('',(#30017,#30018,#30019,#30020,#30021,#30022));
#8081=EDGE_LOOP('',(#30023,#30024,#30025,#30026,#30027));
#8082=EDGE_LOOP('',(#30028,#30029,#30030,#30031,#30032));
#8083=EDGE_LOOP('',(#30033,#30034,#30035,#30036,#30037));
#8084=EDGE_LOOP('',(#30038));
#8085=EDGE_LOOP('',(#30039));
#8086=EDGE_LOOP('',(#30040,#30041,#30042,#30043,#30044,#30045));
#8087=EDGE_LOOP('',(#30046,#30047,#30048,#30049,#30050));
#8088=EDGE_LOOP('',(#30051,#30052,#30053,#30054,#30055));
#8089=EDGE_LOOP('',(#30056,#30057,#30058,#30059,#30060));
#8090=EDGE_LOOP('',(#30061));
#8091=EDGE_LOOP('',(#30062,#30063,#30064,#30065,#30066));
#8092=EDGE_LOOP('',(#30067,#30068,#30069,#30070,#30071));
#8093=EDGE_LOOP('',(#30072));
#8094=EDGE_LOOP('',(#30073,#30074,#30075,#30076,#30077));
#8095=EDGE_LOOP('',(#30078,#30079,#30080,#30081,#30082));
#8096=EDGE_LOOP('',(#30083,#30084,#30085,#30086,#30087));
#8097=EDGE_LOOP('',(#30088));
#8098=EDGE_LOOP('',(#30089));
#8099=EDGE_LOOP('',(#30090,#30091,#30092,#30093,#30094));
#8100=EDGE_LOOP('',(#30095,#30096,#30097,#30098,#30099,#30100));
#8101=EDGE_LOOP('',(#30101,#30102,#30103,#30104));
#8102=EDGE_LOOP('',(#30105,#30106,#30107,#30108,#30109,#30110));
#8103=EDGE_LOOP('',(#30111,#30112,#30113,#30114,#30115));
#8104=EDGE_LOOP('',(#30116));
#8105=EDGE_LOOP('',(#30117));
#8106=EDGE_LOOP('',(#30118));
#8107=EDGE_LOOP('',(#30119));
#8108=EDGE_LOOP('',(#30120));
#8109=EDGE_LOOP('',(#30121));
#8110=EDGE_LOOP('',(#30122,#30123,#30124,#30125,#30126));
#8111=EDGE_LOOP('',(#30127,#30128,#30129,#30130));
#8112=EDGE_LOOP('',(#30131));
#8113=EDGE_LOOP('',(#30132));
#8114=EDGE_LOOP('',(#30133));
#8115=EDGE_LOOP('',(#30134));
#8116=EDGE_LOOP('',(#30135,#30136,#30137,#30138,#30139));
#8117=EDGE_LOOP('',(#30140,#30141,#30142,#30143,#30144,#30145,#30146,#30147,
#30148,#30149,#30150,#30151));
#8118=EDGE_LOOP('',(#30152,#30153,#30154));
#8119=EDGE_LOOP('',(#30155,#30156,#30157,#30158,#30159,#30160));
#8120=EDGE_LOOP('',(#30161,#30162,#30163,#30164,#30165,#30166));
#8121=EDGE_LOOP('',(#30167,#30168,#30169));
#8122=EDGE_LOOP('',(#30170,#30171,#30172));
#8123=EDGE_LOOP('',(#30173,#30174,#30175));
#8124=EDGE_LOOP('',(#30176,#30177,#30178));
#8125=EDGE_LOOP('',(#30179,#30180,#30181));
#8126=EDGE_LOOP('',(#30182,#30183,#30184,#30185,#30186,#30187));
#8127=EDGE_LOOP('',(#30188,#30189,#30190,#30191,#30192,#30193));
#8128=EDGE_LOOP('',(#30194,#30195,#30196,#30197,#30198,#30199));
#8129=EDGE_LOOP('',(#30200,#30201,#30202,#30203,#30204,#30205));
#8130=EDGE_LOOP('',(#30206,#30207,#30208,#30209,#30210,#30211,#30212,#30213,
#30214,#30215,#30216,#30217));
#8131=EDGE_LOOP('',(#30218,#30219,#30220));
#8132=EDGE_LOOP('',(#30221,#30222,#30223,#30224,#30225,#30226));
#8133=EDGE_LOOP('',(#30227,#30228,#30229,#30230,#30231,#30232));
#8134=EDGE_LOOP('',(#30233,#30234,#30235));
#8135=EDGE_LOOP('',(#30236,#30237,#30238));
#8136=EDGE_LOOP('',(#30239,#30240,#30241));
#8137=EDGE_LOOP('',(#30242,#30243,#30244));
#8138=EDGE_LOOP('',(#30245,#30246,#30247));
#8139=EDGE_LOOP('',(#30248,#30249,#30250,#30251,#30252,#30253));
#8140=EDGE_LOOP('',(#30254,#30255,#30256,#30257,#30258,#30259));
#8141=EDGE_LOOP('',(#30260,#30261,#30262,#30263,#30264,#30265));
#8142=EDGE_LOOP('',(#30266,#30267,#30268,#30269,#30270,#30271));
#8143=EDGE_LOOP('',(#30272));
#8144=EDGE_LOOP('',(#30273));
#8145=EDGE_LOOP('',(#30274));
#8146=EDGE_LOOP('',(#30275));
#8147=EDGE_LOOP('',(#30276));
#8148=EDGE_LOOP('',(#30277));
#8149=EDGE_LOOP('',(#30278,#30279,#30280,#30281));
#8150=EDGE_LOOP('',(#30282,#30283,#30284,#30285));
#8151=EDGE_LOOP('',(#30286,#30287,#30288,#30289));
#8152=EDGE_LOOP('',(#30290,#30291,#30292,#30293));
#8153=EDGE_LOOP('',(#30294,#30295,#30296,#30297));
#8154=EDGE_LOOP('',(#30298,#30299,#30300,#30301));
#8155=EDGE_LOOP('',(#30302,#30303,#30304,#30305));
#8156=EDGE_LOOP('',(#30306,#30307,#30308,#30309,#30310,#30311,#30312,#30313));
#8157=EDGE_LOOP('',(#30314,#30315,#30316,#30317));
#8158=EDGE_LOOP('',(#30318,#30319,#30320,#30321));
#8159=EDGE_LOOP('',(#30322,#30323,#30324,#30325));
#8160=EDGE_LOOP('',(#30326,#30327,#30328,#30329));
#8161=EDGE_LOOP('',(#30330,#30331,#30332,#30333));
#8162=EDGE_LOOP('',(#30334,#30335,#30336,#30337));
#8163=EDGE_LOOP('',(#30338,#30339,#30340,#30341));
#8164=EDGE_LOOP('',(#30342,#30343,#30344,#30345));
#8165=EDGE_LOOP('',(#30346,#30347,#30348,#30349,#30350,#30351,#30352,#30353));
#8166=EDGE_LOOP('',(#30354,#30355,#30356,#30357));
#8167=EDGE_LOOP('',(#30358,#30359,#30360,#30361));
#8168=EDGE_LOOP('',(#30362,#30363,#30364,#30365));
#8169=EDGE_LOOP('',(#30366,#30367,#30368,#30369));
#8170=EDGE_LOOP('',(#30370,#30371,#30372,#30373));
#8171=EDGE_LOOP('',(#30374,#30375,#30376,#30377));
#8172=EDGE_LOOP('',(#30378,#30379,#30380,#30381));
#8173=EDGE_LOOP('',(#30382,#30383,#30384,#30385));
#8174=EDGE_LOOP('',(#30386,#30387,#30388,#30389,#30390,#30391,#30392,#30393));
#8175=EDGE_LOOP('',(#30394,#30395,#30396,#30397));
#8176=EDGE_LOOP('',(#30398,#30399,#30400,#30401));
#8177=EDGE_LOOP('',(#30402,#30403,#30404,#30405));
#8178=EDGE_LOOP('',(#30406,#30407,#30408,#30409));
#8179=EDGE_LOOP('',(#30410,#30411,#30412,#30413));
#8180=EDGE_LOOP('',(#30414,#30415,#30416,#30417));
#8181=EDGE_LOOP('',(#30418,#30419,#30420,#30421));
#8182=EDGE_LOOP('',(#30422,#30423,#30424,#30425));
#8183=EDGE_LOOP('',(#30426,#30427,#30428,#30429,#30430,#30431,#30432,#30433));
#8184=EDGE_LOOP('',(#30434,#30435,#30436,#30437));
#8185=EDGE_LOOP('',(#30438,#30439,#30440,#30441));
#8186=EDGE_LOOP('',(#30442,#30443,#30444,#30445));
#8187=EDGE_LOOP('',(#30446,#30447,#30448,#30449));
#8188=EDGE_LOOP('',(#30450,#30451));
#8189=EDGE_LOOP('',(#30452,#30453,#30454,#30455));
#8190=EDGE_LOOP('',(#30456,#30457));
#8191=EDGE_LOOP('',(#30458,#30459,#30460,#30461));
#8192=EDGE_LOOP('',(#30462,#30463));
#8193=EDGE_LOOP('',(#30464,#30465,#30466,#30467,#30468,#30469));
#8194=EDGE_LOOP('',(#30470));
#8195=EDGE_LOOP('',(#30471,#30472,#30473,#30474,#30475,#30476));
#8196=EDGE_LOOP('',(#30477));
#8197=EDGE_LOOP('',(#30478,#30479,#30480,#30481,#30482,#30483));
#8198=EDGE_LOOP('',(#30484));
#8199=EDGE_LOOP('',(#30485,#30486,#30487,#30488,#30489));
#8200=EDGE_LOOP('',(#30490,#30491,#30492,#30493));
#8201=EDGE_LOOP('',(#30494,#30495,#30496,#30497));
#8202=EDGE_LOOP('',(#30498,#30499,#30500,#30501));
#8203=EDGE_LOOP('',(#30502,#30503,#30504,#30505));
#8204=EDGE_LOOP('',(#30506,#30507,#30508,#30509,#30510,#30511,#30512,#30513,
#30514,#30515,#30516,#30517));
#8205=EDGE_LOOP('',(#30518,#30519,#30520,#30521));
#8206=EDGE_LOOP('',(#30522,#30523,#30524,#30525,#30526,#30527,#30528,#30529,
#30530,#30531,#30532,#30533));
#8207=EDGE_LOOP('',(#30534,#30535,#30536,#30537));
#8208=EDGE_LOOP('',(#30538,#30539,#30540,#30541,#30542,#30543,#30544,#30545,
#30546,#30547,#30548,#30549));
#8209=EDGE_LOOP('',(#30550,#30551,#30552,#30553));
#8210=EDGE_LOOP('',(#30554,#30555,#30556,#30557,#30558,#30559,#30560,#30561,
#30562,#30563,#30564,#30565));
#8211=EDGE_LOOP('',(#30566,#30567,#30568,#30569));
#8212=EDGE_LOOP('',(#30570,#30571,#30572,#30573,#30574,#30575,#30576,#30577,
#30578,#30579,#30580,#30581,#30582,#30583,#30584,#30585));
#8213=EDGE_LOOP('',(#30586));
#8214=EDGE_LOOP('',(#30587,#30588,#30589,#30590));
#8215=EDGE_LOOP('',(#30591,#30592,#30593,#30594));
#8216=EDGE_LOOP('',(#30595,#30596,#30597,#30598));
#8217=EDGE_LOOP('',(#30599,#30600,#30601,#30602));
#8218=EDGE_LOOP('',(#30603,#30604,#30605,#30606));
#8219=EDGE_LOOP('',(#30607,#30608,#30609,#30610));
#8220=EDGE_LOOP('',(#30611,#30612,#30613,#30614));
#8221=EDGE_LOOP('',(#30615,#30616,#30617,#30618));
#8222=EDGE_LOOP('',(#30619,#30620,#30621,#30622));
#8223=EDGE_LOOP('',(#30623,#30624,#30625,#30626));
#8224=EDGE_LOOP('',(#30627,#30628,#30629,#30630));
#8225=EDGE_LOOP('',(#30631,#30632,#30633,#30634));
#8226=EDGE_LOOP('',(#30635,#30636,#30637,#30638,#30639,#30640));
#8227=EDGE_LOOP('',(#30641));
#8228=EDGE_LOOP('',(#30642,#30643,#30644,#30645));
#8229=EDGE_LOOP('',(#30646,#30647));
#8230=EDGE_LOOP('',(#30648,#30649,#30650,#30651));
#8231=EDGE_LOOP('',(#30652,#30653,#30654,#30655));
#8232=EDGE_LOOP('',(#30656,#30657,#30658,#30659));
#8233=EDGE_LOOP('',(#30660,#30661,#30662,#30663));
#8234=EDGE_LOOP('',(#30664,#30665,#30666,#30667));
#8235=EDGE_LOOP('',(#30668,#30669,#30670,#30671));
#8236=EDGE_LOOP('',(#30672,#30673,#30674,#30675));
#8237=EDGE_LOOP('',(#30676,#30677,#30678,#30679));
#8238=EDGE_LOOP('',(#30680,#30681,#30682,#30683,#30684,#30685,#30686,#30687));
#8239=EDGE_LOOP('',(#30688,#30689,#30690,#30691));
#8240=EDGE_LOOP('',(#30692,#30693,#30694,#30695));
#8241=EDGE_LOOP('',(#30696,#30697,#30698,#30699));
#8242=EDGE_LOOP('',(#30700,#30701,#30702,#30703));
#8243=EDGE_LOOP('',(#30704,#30705,#30706,#30707));
#8244=EDGE_LOOP('',(#30708,#30709,#30710,#30711));
#8245=EDGE_LOOP('',(#30712,#30713,#30714,#30715));
#8246=EDGE_LOOP('',(#30716,#30717,#30718,#30719));
#8247=EDGE_LOOP('',(#30720,#30721,#30722,#30723,#30724,#30725,#30726,#30727));
#8248=EDGE_LOOP('',(#30728,#30729,#30730,#30731));
#8249=EDGE_LOOP('',(#30732,#30733,#30734,#30735));
#8250=EDGE_LOOP('',(#30736,#30737,#30738,#30739));
#8251=EDGE_LOOP('',(#30740,#30741,#30742,#30743));
#8252=EDGE_LOOP('',(#30744,#30745,#30746,#30747));
#8253=EDGE_LOOP('',(#30748,#30749,#30750,#30751));
#8254=EDGE_LOOP('',(#30752,#30753,#30754,#30755));
#8255=EDGE_LOOP('',(#30756,#30757,#30758,#30759));
#8256=EDGE_LOOP('',(#30760,#30761,#30762,#30763,#30764,#30765,#30766,#30767));
#8257=EDGE_LOOP('',(#30768,#30769,#30770,#30771));
#8258=EDGE_LOOP('',(#30772,#30773,#30774,#30775));
#8259=EDGE_LOOP('',(#30776,#30777,#30778,#30779));
#8260=EDGE_LOOP('',(#30780,#30781,#30782,#30783));
#8261=EDGE_LOOP('',(#30784,#30785,#30786,#30787));
#8262=EDGE_LOOP('',(#30788,#30789,#30790,#30791));
#8263=EDGE_LOOP('',(#30792,#30793,#30794,#30795));
#8264=EDGE_LOOP('',(#30796,#30797,#30798,#30799));
#8265=EDGE_LOOP('',(#30800,#30801,#30802,#30803,#30804,#30805,#30806,#30807));
#8266=EDGE_LOOP('',(#30808,#30809,#30810,#30811));
#8267=EDGE_LOOP('',(#30812,#30813,#30814,#30815));
#8268=EDGE_LOOP('',(#30816,#30817,#30818,#30819));
#8269=EDGE_LOOP('',(#30820,#30821,#30822,#30823));
#8270=EDGE_LOOP('',(#30824,#30825,#30826,#30827));
#8271=EDGE_LOOP('',(#30828,#30829,#30830,#30831));
#8272=EDGE_LOOP('',(#30832,#30833,#30834,#30835));
#8273=EDGE_LOOP('',(#30836,#30837,#30838,#30839));
#8274=EDGE_LOOP('',(#30840,#30841,#30842,#30843,#30844));
#8275=EDGE_LOOP('',(#30845));
#8276=EDGE_LOOP('',(#30846));
#8277=EDGE_LOOP('',(#30847));
#8278=EDGE_LOOP('',(#30848));
#8279=EDGE_LOOP('',(#30849));
#8280=EDGE_LOOP('',(#30850));
#8281=EDGE_LOOP('',(#30851));
#8282=EDGE_LOOP('',(#30852,#30853,#30854,#30855,#30856,#30857,#30858,#30859));
#8283=EDGE_LOOP('',(#30860,#30861,#30862,#30863));
#8284=EDGE_LOOP('',(#30864,#30865,#30866,#30867));
#8285=EDGE_LOOP('',(#30868,#30869,#30870,#30871,#30872,#30873));
#8286=EDGE_LOOP('',(#30874,#30875,#30876,#30877,#30878,#30879));
#8287=EDGE_LOOP('',(#30880,#30881,#30882,#30883));
#8288=EDGE_LOOP('',(#30884));
#8289=EDGE_LOOP('',(#30885,#30886,#30887,#30888,#30889,#30890,#30891,#30892));
#8290=EDGE_LOOP('',(#30893,#30894,#30895,#30896,#30897,#30898,#30899,#30900,
#30901,#30902,#30903,#30904,#30905,#30906,#30907,#30908));
#8291=EDGE_LOOP('',(#30909));
#8292=EDGE_LOOP('',(#30910));
#8293=EDGE_LOOP('',(#30911));
#8294=EDGE_LOOP('',(#30912));
#8295=EDGE_LOOP('',(#30913));
#8296=EDGE_LOOP('',(#30914));
#8297=EDGE_LOOP('',(#30915,#30916,#30917,#30918,#30919,#30920,#30921,#30922));
#8298=EDGE_LOOP('',(#30923,#30924,#30925,#30926,#30927,#30928,#30929,#30930));
#8299=EDGE_LOOP('',(#30931,#30932,#30933,#30934,#30935,#30936,#30937,#30938));
#8300=EDGE_LOOP('',(#30939,#30940,#30941,#30942,#30943,#30944,#30945,#30946));
#8301=EDGE_LOOP('',(#30947,#30948,#30949,#30950,#30951,#30952,#30953,#30954));
#8302=EDGE_LOOP('',(#30955,#30956,#30957,#30958,#30959,#30960,#30961,#30962));
#8303=EDGE_LOOP('',(#30963,#30964,#30965,#30966,#30967,#30968,#30969,#30970));
#8304=EDGE_LOOP('',(#30971,#30972,#30973,#30974,#30975,#30976));
#8305=EDGE_LOOP('',(#30977,#30978,#30979,#30980,#30981,#30982));
#8306=EDGE_LOOP('',(#30983,#30984,#30985,#30986));
#8307=EDGE_LOOP('',(#30987));
#8308=EDGE_LOOP('',(#30988));
#8309=EDGE_LOOP('',(#30989,#30990,#30991,#30992,#30993));
#8310=EDGE_LOOP('',(#30994,#30995,#30996,#30997,#30998,#30999));
#8311=EDGE_LOOP('',(#31000,#31001,#31002,#31003,#31004));
#8312=EDGE_LOOP('',(#31005,#31006,#31007,#31008));
#8313=EDGE_LOOP('',(#31009,#31010,#31011,#31012));
#8314=EDGE_LOOP('',(#31013,#31014,#31015,#31016));
#8315=EDGE_LOOP('',(#31017,#31018,#31019,#31020));
#8316=EDGE_LOOP('',(#31021,#31022,#31023,#31024));
#8317=EDGE_LOOP('',(#31025,#31026,#31027,#31028,#31029,#31030));
#8318=EDGE_LOOP('',(#31031,#31032,#31033,#31034));
#8319=EDGE_LOOP('',(#31035));
#8320=EDGE_LOOP('',(#31036,#31037,#31038,#31039,#31040,#31041));
#8321=EDGE_LOOP('',(#31042,#31043,#31044,#31045));
#8322=EDGE_LOOP('',(#31046));
#8323=EDGE_LOOP('',(#31047));
#8324=EDGE_LOOP('',(#31048,#31049,#31050,#31051));
#8325=EDGE_LOOP('',(#31052,#31053,#31054,#31055));
#8326=EDGE_LOOP('',(#31056,#31057,#31058,#31059,#31060));
#8327=EDGE_LOOP('',(#31061,#31062,#31063,#31064,#31065));
#8328=EDGE_LOOP('',(#31066));
#8329=EDGE_LOOP('',(#31067));
#8330=EDGE_LOOP('',(#31068,#31069,#31070,#31071));
#8331=EDGE_LOOP('',(#31072));
#8332=EDGE_LOOP('',(#31073));
#8333=EDGE_LOOP('',(#31074,#31075,#31076,#31077,#31078,#31079));
#8334=EDGE_LOOP('',(#31080,#31081));
#8335=EDGE_LOOP('',(#31082,#31083));
#8336=EDGE_LOOP('',(#31084,#31085,#31086,#31087,#31088));
#8337=EDGE_LOOP('',(#31089));
#8338=EDGE_LOOP('',(#31090));
#8339=EDGE_LOOP('',(#31091,#31092,#31093,#31094,#31095));
#8340=EDGE_LOOP('',(#31096,#31097,#31098,#31099,#31100,#31101));
#8341=EDGE_LOOP('',(#31102));
#8342=EDGE_LOOP('',(#31103));
#8343=EDGE_LOOP('',(#31104));
#8344=EDGE_LOOP('',(#31105));
#8345=EDGE_LOOP('',(#31106,#31107,#31108,#31109,#31110,#31111));
#8346=LINE('',#48842,#10893);
#8347=LINE('',#48844,#10894);
#8348=LINE('',#48846,#10895);
#8349=LINE('',#48847,#10896);
#8350=LINE('',#48851,#10897);
#8351=LINE('',#48853,#10898);
#8352=LINE('',#48855,#10899);
#8353=LINE('',#48856,#10900);
#8354=LINE('',#48858,#10901);
#8355=LINE('',#48859,#10902);
#8356=LINE('',#48863,#10903);
#8357=LINE('',#48865,#10904);
#8358=LINE('',#48869,#10905);
#8359=LINE('',#48873,#10906);
#8360=LINE('',#48875,#10907);
#8361=LINE('',#48879,#10908);
#8362=LINE('',#48883,#10909);
#8363=LINE('',#48885,#10910);
#8364=LINE('',#48889,#10911);
#8365=LINE('',#48896,#10912);
#8366=LINE('',#48898,#10913);
#8367=LINE('',#48899,#10914);
#8368=LINE('',#48902,#10915);
#8369=LINE('',#48906,#10916);
#8370=LINE('',#48907,#10917);
#8371=LINE('',#48910,#10918);
#8372=LINE('',#48911,#10919);
#8373=LINE('',#48914,#10920);
#8374=LINE('',#48916,#10921);
#8375=LINE('',#48917,#10922);
#8376=LINE('',#48920,#10923);
#8377=LINE('',#48924,#10924);
#8378=LINE('',#48925,#10925);
#8379=LINE('',#48928,#10926);
#8380=LINE('',#48929,#10927);
#8381=LINE('',#48933,#10928);
#8382=LINE('',#48938,#10929);
#8383=LINE('',#48941,#10930);
#8384=LINE('',#48944,#10931);
#8385=LINE('',#48945,#10932);
#8386=LINE('',#48947,#10933);
#8387=LINE('',#48950,#10934);
#8388=LINE('',#48951,#10935);
#8389=LINE('',#48961,#10936);
#8390=LINE('',#48965,#10937);
#8391=LINE('',#48969,#10938);
#8392=LINE('',#48972,#10939);
#8393=LINE('',#48985,#10940);
#8394=LINE('',#48989,#10941);
#8395=LINE('',#48993,#10942);
#8396=LINE('',#48996,#10943);
#8397=LINE('',#49001,#10944);
#8398=LINE('',#49002,#10945);
#8399=LINE('',#49011,#10946);
#8400=LINE('',#49014,#10947);
#8401=LINE('',#49020,#10948);
#8402=LINE('',#49022,#10949);
#8403=LINE('',#49026,#10950);
#8404=LINE('',#49027,#10951);
#8405=LINE('',#49035,#10952);
#8406=LINE('',#49037,#10953);
#8407=LINE('',#49041,#10954);
#8408=LINE('',#49042,#10955);
#8409=LINE('',#49049,#10956);
#8410=LINE('',#49051,#10957);
#8411=LINE('',#49052,#10958);
#8412=LINE('',#49060,#10959);
#8413=LINE('',#49062,#10960);
#8414=LINE('',#49066,#10961);
#8415=LINE('',#49067,#10962);
#8416=LINE('',#49071,#10963);
#8417=LINE('',#49073,#10964);
#8418=LINE('',#49075,#10965);
#8419=LINE('',#49077,#10966);
#8420=LINE('',#49159,#10967);
#8421=LINE('',#49253,#10968);
#8422=LINE('',#49255,#10969);
#8423=LINE('',#49256,#10970);
#8424=LINE('',#49262,#10971);
#8425=LINE('',#49264,#10972);
#8426=LINE('',#49265,#10973);
#8427=LINE('',#49271,#10974);
#8428=LINE('',#49273,#10975);
#8429=LINE('',#49274,#10976);
#8430=LINE('',#49280,#10977);
#8431=LINE('',#49282,#10978);
#8432=LINE('',#49283,#10979);
#8433=LINE('',#49342,#10980);
#8434=LINE('',#49352,#10981);
#8435=LINE('',#49359,#10982);
#8436=LINE('',#49360,#10983);
#8437=LINE('',#49364,#10984);
#8438=LINE('',#49377,#10985);
#8439=LINE('',#49389,#10986);
#8440=LINE('',#49390,#10987);
#8441=LINE('',#49399,#10988);
#8442=LINE('',#49413,#10989);
#8443=LINE('',#49425,#10990);
#8444=LINE('',#49582,#10991);
#8445=LINE('',#49701,#10992);
#8446=LINE('',#49971,#10993);
#8447=LINE('',#50096,#10994);
#8448=LINE('',#50257,#10995);
#8449=LINE('',#50271,#10996);
#8450=LINE('',#50272,#10997);
#8451=LINE('',#50276,#10998);
#8452=LINE('',#50283,#10999);
#8453=LINE('',#50297,#11000);
#8454=LINE('',#50309,#11001);
#8455=LINE('',#50327,#11002);
#8456=LINE('',#50430,#11003);
#8457=LINE('',#50766,#11004);
#8458=LINE('',#50884,#11005);
#8459=LINE('',#50891,#11006);
#8460=LINE('',#50898,#11007);
#8461=LINE('',#50905,#11008);
#8462=LINE('',#50912,#11009);
#8463=LINE('',#50919,#11010);
#8464=LINE('',#50926,#11011);
#8465=LINE('',#50932,#11012);
#8466=LINE('',#50936,#11013);
#8467=LINE('',#50940,#11014);
#8468=LINE('',#50943,#11015);
#8469=LINE('',#50945,#11016);
#8470=LINE('',#50946,#11017);
#8471=LINE('',#50948,#11018);
#8472=LINE('',#50950,#11019);
#8473=LINE('',#50952,#11020);
#8474=LINE('',#50954,#11021);
#8475=LINE('',#50956,#11022);
#8476=LINE('',#50958,#11023);
#8477=LINE('',#50974,#11024);
#8478=LINE('',#50980,#11025);
#8479=LINE('',#50994,#11026);
#8480=LINE('',#50996,#11027);
#8481=LINE('',#50998,#11028);
#8482=LINE('',#51000,#11029);
#8483=LINE('',#51002,#11030);
#8484=LINE('',#51003,#11031);
#8485=LINE('',#51005,#11032);
#8486=LINE('',#51012,#11033);
#8487=LINE('',#51013,#11034);
#8488=LINE('',#51019,#11035);
#8489=LINE('',#51025,#11036);
#8490=LINE('',#51031,#11037);
#8491=LINE('',#51038,#11038);
#8492=LINE('',#51048,#11039);
#8493=LINE('',#51063,#11040);
#8494=LINE('',#51069,#11041);
#8495=LINE('',#51083,#11042);
#8496=LINE('',#51085,#11043);
#8497=LINE('',#51087,#11044);
#8498=LINE('',#51089,#11045);
#8499=LINE('',#51091,#11046);
#8500=LINE('',#51092,#11047);
#8501=LINE('',#51094,#11048);
#8502=LINE('',#51101,#11049);
#8503=LINE('',#51102,#11050);
#8504=LINE('',#51108,#11051);
#8505=LINE('',#51114,#11052);
#8506=LINE('',#51120,#11053);
#8507=LINE('',#51127,#11054);
#8508=LINE('',#51137,#11055);
#8509=LINE('',#51152,#11056);
#8510=LINE('',#51158,#11057);
#8511=LINE('',#51172,#11058);
#8512=LINE('',#51174,#11059);
#8513=LINE('',#51176,#11060);
#8514=LINE('',#51178,#11061);
#8515=LINE('',#51180,#11062);
#8516=LINE('',#51181,#11063);
#8517=LINE('',#51183,#11064);
#8518=LINE('',#51190,#11065);
#8519=LINE('',#51191,#11066);
#8520=LINE('',#51197,#11067);
#8521=LINE('',#51203,#11068);
#8522=LINE('',#51209,#11069);
#8523=LINE('',#51216,#11070);
#8524=LINE('',#51226,#11071);
#8525=LINE('',#51241,#11072);
#8526=LINE('',#51247,#11073);
#8527=LINE('',#51312,#11074);
#8528=LINE('',#51314,#11075);
#8529=LINE('',#51315,#11076);
#8530=LINE('',#51318,#11077);
#8531=LINE('',#51319,#11078);
#8532=LINE('',#51322,#11079);
#8533=LINE('',#51323,#11080);
#8534=LINE('',#51326,#11081);
#8535=LINE('',#51328,#11082);
#8536=LINE('',#51329,#11083);
#8537=LINE('',#51333,#11084);
#8538=LINE('',#51335,#11085);
#8539=LINE('',#51339,#11086);
#8540=LINE('',#51344,#11087);
#8541=LINE('',#51346,#11088);
#8542=LINE('',#51348,#11089);
#8543=LINE('',#51349,#11090);
#8544=LINE('',#51352,#11091);
#8545=LINE('',#51354,#11092);
#8546=LINE('',#51355,#11093);
#8547=LINE('',#51358,#11094);
#8548=LINE('',#51360,#11095);
#8549=LINE('',#51361,#11096);
#8550=LINE('',#51363,#11097);
#8551=LINE('',#51364,#11098);
#8552=LINE('',#51368,#11099);
#8553=LINE('',#51370,#11100);
#8554=LINE('',#51372,#11101);
#8555=LINE('',#51373,#11102);
#8556=LINE('',#51376,#11103);
#8557=LINE('',#51378,#11104);
#8558=LINE('',#51379,#11105);
#8559=LINE('',#51382,#11106);
#8560=LINE('',#51384,#11107);
#8561=LINE('',#51385,#11108);
#8562=LINE('',#51387,#11109);
#8563=LINE('',#51388,#11110);
#8564=LINE('',#51393,#11111);
#8565=LINE('',#51395,#11112);
#8566=LINE('',#51397,#11113);
#8567=LINE('',#51398,#11114);
#8568=LINE('',#51401,#11115);
#8569=LINE('',#51403,#11116);
#8570=LINE('',#51404,#11117);
#8571=LINE('',#51407,#11118);
#8572=LINE('',#51409,#11119);
#8573=LINE('',#51410,#11120);
#8574=LINE('',#51412,#11121);
#8575=LINE('',#51413,#11122);
#8576=LINE('',#51421,#11123);
#8577=LINE('',#51427,#11124);
#8578=LINE('',#51433,#11125);
#8579=LINE('',#51439,#11126);
#8580=LINE('',#51445,#11127);
#8581=LINE('',#51451,#11128);
#8582=LINE('',#51456,#11129);
#8583=LINE('',#51458,#11130);
#8584=LINE('',#51460,#11131);
#8585=LINE('',#51461,#11132);
#8586=LINE('',#51464,#11133);
#8587=LINE('',#51466,#11134);
#8588=LINE('',#51468,#11135);
#8589=LINE('',#51469,#11136);
#8590=LINE('',#51473,#11137);
#8591=LINE('',#51474,#11138);
#8592=LINE('',#51475,#11139);
#8593=LINE('',#51478,#11140);
#8594=LINE('',#51479,#11141);
#8595=LINE('',#51482,#11142);
#8596=LINE('',#51483,#11143);
#8597=LINE('',#51485,#11144);
#8598=LINE('',#51488,#11145);
#8599=LINE('',#51490,#11146);
#8600=LINE('',#51491,#11147);
#8601=LINE('',#51494,#11148);
#8602=LINE('',#51496,#11149);
#8603=LINE('',#51498,#11150);
#8604=LINE('',#51499,#11151);
#8605=LINE('',#51503,#11152);
#8606=LINE('',#51505,#11153);
#8607=LINE('',#51507,#11154);
#8608=LINE('',#51508,#11155);
#8609=LINE('',#51511,#11156);
#8610=LINE('',#51513,#11157);
#8611=LINE('',#51514,#11158);
#8612=LINE('',#51518,#11159);
#8613=LINE('',#51520,#11160);
#8614=LINE('',#51522,#11161);
#8615=LINE('',#51523,#11162);
#8616=LINE('',#51526,#11163);
#8617=LINE('',#51528,#11164);
#8618=LINE('',#51529,#11165);
#8619=LINE('',#51532,#11166);
#8620=LINE('',#51534,#11167);
#8621=LINE('',#51535,#11168);
#8622=LINE('',#51538,#11169);
#8623=LINE('',#51540,#11170);
#8624=LINE('',#51541,#11171);
#8625=LINE('',#51543,#11172);
#8626=LINE('',#51544,#11173);
#8627=LINE('',#51546,#11174);
#8628=LINE('',#51547,#11175);
#8629=LINE('',#51551,#11176);
#8630=LINE('',#51552,#11177);
#8631=LINE('',#51555,#11178);
#8632=LINE('',#51556,#11179);
#8633=LINE('',#51559,#11180);
#8634=LINE('',#51560,#11181);
#8635=LINE('',#51562,#11182);
#8636=LINE('',#51707,#11183);
#8637=LINE('',#51709,#11184);
#8638=LINE('',#51710,#11185);
#8639=LINE('',#51713,#11186);
#8640=LINE('',#51714,#11187);
#8641=LINE('',#51717,#11188);
#8642=LINE('',#51718,#11189);
#8643=LINE('',#51723,#11190);
#8644=LINE('',#51726,#11191);
#8645=LINE('',#51763,#11192);
#8646=LINE('',#51788,#11193);
#8647=LINE('',#51802,#11194);
#8648=LINE('',#51816,#11195);
#8649=LINE('',#51829,#11196);
#8650=LINE('',#51831,#11197);
#8651=LINE('',#51874,#11198);
#8652=LINE('',#51894,#11199);
#8653=LINE('',#51898,#11200);
#8654=LINE('',#51911,#11201);
#8655=LINE('',#51924,#11202);
#8656=LINE('',#51926,#11203);
#8657=LINE('',#51927,#11204);
#8658=LINE('',#51930,#11205);
#8659=LINE('',#51932,#11206);
#8660=LINE('',#51933,#11207);
#8661=LINE('',#51950,#11208);
#8662=LINE('',#51969,#11209);
#8663=LINE('',#51983,#11210);
#8664=LINE('',#51984,#11211);
#8665=LINE('',#51987,#11212);
#8666=LINE('',#52040,#11213);
#8667=LINE('',#52042,#11214);
#8668=LINE('',#52043,#11215);
#8669=LINE('',#52048,#11216);
#8670=LINE('',#52049,#11217);
#8671=LINE('',#52055,#11218);
#8672=LINE('',#52059,#11219);
#8673=LINE('',#52066,#11220);
#8674=LINE('',#52068,#11221);
#8675=LINE('',#52069,#11222);
#8676=LINE('',#52074,#11223);
#8677=LINE('',#52075,#11224);
#8678=LINE('',#52080,#11225);
#8679=LINE('',#52081,#11226);
#8680=LINE('',#52086,#11227);
#8681=LINE('',#52087,#11228);
#8682=LINE('',#52092,#11229);
#8683=LINE('',#52093,#11230);
#8684=LINE('',#52098,#11231);
#8685=LINE('',#52099,#11232);
#8686=LINE('',#52104,#11233);
#8687=LINE('',#52105,#11234);
#8688=LINE('',#52110,#11235);
#8689=LINE('',#52111,#11236);
#8690=LINE('',#52116,#11237);
#8691=LINE('',#52117,#11238);
#8692=LINE('',#52122,#11239);
#8693=LINE('',#52123,#11240);
#8694=LINE('',#52128,#11241);
#8695=LINE('',#52129,#11242);
#8696=LINE('',#52132,#11243);
#8697=LINE('',#52148,#11244);
#8698=LINE('',#52154,#11245);
#8699=LINE('',#52157,#11246);
#8700=LINE('',#52160,#11247);
#8701=LINE('',#52162,#11248);
#8702=LINE('',#52163,#11249);
#8703=LINE('',#52169,#11250);
#8704=LINE('',#52172,#11251);
#8705=LINE('',#52174,#11252);
#8706=LINE('',#52175,#11253);
#8707=LINE('',#52181,#11254);
#8708=LINE('',#52184,#11255);
#8709=LINE('',#52186,#11256);
#8710=LINE('',#52187,#11257);
#8711=LINE('',#52193,#11258);
#8712=LINE('',#52195,#11259);
#8713=LINE('',#52196,#11260);
#8714=LINE('',#52200,#11261);
#8715=LINE('',#52202,#11262);
#8716=LINE('',#52204,#11263);
#8717=LINE('',#52205,#11264);
#8718=LINE('',#52213,#11265);
#8719=LINE('',#52217,#11266);
#8720=LINE('',#52221,#11267);
#8721=LINE('',#52225,#11268);
#8722=LINE('',#52229,#11269);
#8723=LINE('',#52232,#11270);
#8724=LINE('',#52235,#11271);
#8725=LINE('',#52236,#11272);
#8726=LINE('',#52240,#11273);
#8727=LINE('',#52243,#11274);
#8728=LINE('',#52244,#11275);
#8729=LINE('',#52248,#11276);
#8730=LINE('',#52251,#11277);
#8731=LINE('',#52252,#11278);
#8732=LINE('',#52256,#11279);
#8733=LINE('',#52258,#11280);
#8734=LINE('',#52288,#11281);
#8735=LINE('',#52317,#11282);
#8736=LINE('',#52320,#11283);
#8737=LINE('',#52322,#11284);
#8738=LINE('',#52323,#11285);
#8739=LINE('',#52326,#11286);
#8740=LINE('',#52327,#11287);
#8741=LINE('',#52330,#11288);
#8742=LINE('',#52331,#11289);
#8743=LINE('',#52334,#11290);
#8744=LINE('',#52335,#11291);
#8745=LINE('',#52338,#11292);
#8746=LINE('',#52339,#11293);
#8747=LINE('',#52342,#11294);
#8748=LINE('',#52343,#11295);
#8749=LINE('',#52346,#11296);
#8750=LINE('',#52347,#11297);
#8751=LINE('',#52350,#11298);
#8752=LINE('',#52351,#11299);
#8753=LINE('',#52354,#11300);
#8754=LINE('',#52355,#11301);
#8755=LINE('',#52358,#11302);
#8756=LINE('',#52359,#11303);
#8757=LINE('',#52362,#11304);
#8758=LINE('',#52363,#11305);
#8759=LINE('',#52365,#11306);
#8760=LINE('',#52369,#11307);
#8761=LINE('',#52371,#11308);
#8762=LINE('',#52372,#11309);
#8763=LINE('',#52375,#11310);
#8764=LINE('',#52376,#11311);
#8765=LINE('',#52379,#11312);
#8766=LINE('',#52380,#11313);
#8767=LINE('',#52383,#11314);
#8768=LINE('',#52384,#11315);
#8769=LINE('',#52387,#11316);
#8770=LINE('',#52388,#11317);
#8771=LINE('',#52391,#11318);
#8772=LINE('',#52392,#11319);
#8773=LINE('',#52395,#11320);
#8774=LINE('',#52396,#11321);
#8775=LINE('',#52399,#11322);
#8776=LINE('',#52400,#11323);
#8777=LINE('',#52403,#11324);
#8778=LINE('',#52404,#11325);
#8779=LINE('',#52407,#11326);
#8780=LINE('',#52408,#11327);
#8781=LINE('',#52411,#11328);
#8782=LINE('',#52412,#11329);
#8783=LINE('',#52414,#11330);
#8784=LINE('',#52418,#11331);
#8785=LINE('',#52420,#11332);
#8786=LINE('',#52422,#11333);
#8787=LINE('',#52424,#11334);
#8788=LINE('',#52426,#11335);
#8789=LINE('',#52428,#11336);
#8790=LINE('',#52430,#11337);
#8791=LINE('',#52432,#11338);
#8792=LINE('',#52433,#11339);
#8793=LINE('',#52435,#11340);
#8794=LINE('',#52437,#11341);
#8795=LINE('',#52439,#11342);
#8796=LINE('',#52441,#11343);
#8797=LINE('',#52443,#11344);
#8798=LINE('',#52445,#11345);
#8799=LINE('',#52447,#11346);
#8800=LINE('',#52449,#11347);
#8801=LINE('',#52464,#11348);
#8802=LINE('',#52465,#11349);
#8803=LINE('',#52468,#11350);
#8804=LINE('',#52469,#11351);
#8805=LINE('',#52476,#11352);
#8806=LINE('',#52488,#11353);
#8807=LINE('',#52490,#11354);
#8808=LINE('',#52491,#11355);
#8809=LINE('',#52495,#11356);
#8810=LINE('',#52496,#11357);
#8811=LINE('',#52502,#11358);
#8812=LINE('',#52504,#11359);
#8813=LINE('',#52511,#11360);
#8814=LINE('',#52513,#11361);
#8815=LINE('',#52514,#11362);
#8816=LINE('',#52517,#11363);
#8817=LINE('',#52518,#11364);
#8818=LINE('',#52521,#11365);
#8819=LINE('',#52522,#11366);
#8820=LINE('',#52525,#11367);
#8821=LINE('',#52526,#11368);
#8822=LINE('',#52529,#11369);
#8823=LINE('',#52530,#11370);
#8824=LINE('',#52533,#11371);
#8825=LINE('',#52534,#11372);
#8826=LINE('',#52537,#11373);
#8827=LINE('',#52538,#11374);
#8828=LINE('',#52541,#11375);
#8829=LINE('',#52542,#11376);
#8830=LINE('',#52545,#11377);
#8831=LINE('',#52546,#11378);
#8832=LINE('',#52549,#11379);
#8833=LINE('',#52550,#11380);
#8834=LINE('',#52553,#11381);
#8835=LINE('',#52554,#11382);
#8836=LINE('',#52557,#11383);
#8837=LINE('',#52561,#11384);
#8838=LINE('',#52585,#11385);
#8839=LINE('',#52587,#11386);
#8840=LINE('',#52589,#11387);
#8841=LINE('',#52591,#11388);
#8842=LINE('',#52593,#11389);
#8843=LINE('',#52595,#11390);
#8844=LINE('',#52597,#11391);
#8845=LINE('',#52599,#11392);
#8846=LINE('',#52601,#11393);
#8847=LINE('',#52602,#11394);
#8848=LINE('',#52604,#11395);
#8849=LINE('',#52606,#11396);
#8850=LINE('',#52608,#11397);
#8851=LINE('',#52610,#11398);
#8852=LINE('',#52612,#11399);
#8853=LINE('',#52614,#11400);
#8854=LINE('',#52616,#11401);
#8855=LINE('',#52618,#11402);
#8856=LINE('',#52620,#11403);
#8857=LINE('',#52649,#11404);
#8858=LINE('',#52698,#11405);
#8859=LINE('',#52753,#11406);
#8860=LINE('',#52871,#11407);
#8861=LINE('',#52878,#11408);
#8862=LINE('',#52887,#11409);
#8863=LINE('',#52889,#11410);
#8864=LINE('',#52890,#11411);
#8865=LINE('',#52893,#11412);
#8866=LINE('',#52895,#11413);
#8867=LINE('',#52897,#11414);
#8868=LINE('',#52899,#11415);
#8869=LINE('',#52901,#11416);
#8870=LINE('',#52903,#11417);
#8871=LINE('',#52905,#11418);
#8872=LINE('',#52907,#11419);
#8873=LINE('',#52909,#11420);
#8874=LINE('',#52911,#11421);
#8875=LINE('',#52913,#11422);
#8876=LINE('',#52915,#11423);
#8877=LINE('',#52917,#11424);
#8878=LINE('',#52919,#11425);
#8879=LINE('',#52920,#11426);
#8880=LINE('',#52924,#11427);
#8881=LINE('',#52928,#11428);
#8882=LINE('',#52930,#11429);
#8883=LINE('',#52932,#11430);
#8884=LINE('',#52934,#11431);
#8885=LINE('',#52936,#11432);
#8886=LINE('',#52937,#11433);
#8887=LINE('',#52941,#11434);
#8888=LINE('',#52943,#11435);
#8889=LINE('',#52945,#11436);
#8890=LINE('',#52947,#11437);
#8891=LINE('',#52949,#11438);
#8892=LINE('',#52950,#11439);
#8893=LINE('',#52954,#11440);
#8894=LINE('',#52958,#11441);
#8895=LINE('',#52964,#11442);
#8896=LINE('',#52967,#11443);
#8897=LINE('',#52972,#11444);
#8898=LINE('',#52973,#11445);
#8899=LINE('',#52976,#11446);
#8900=LINE('',#52977,#11447);
#8901=LINE('',#52981,#11448);
#8902=LINE('',#52983,#11449);
#8903=LINE('',#52987,#11450);
#8904=LINE('',#52991,#11451);
#8905=LINE('',#52999,#11452);
#8906=LINE('',#53000,#11453);
#8907=LINE('',#53003,#11454);
#8908=LINE('',#53004,#11455);
#8909=LINE('',#53008,#11456);
#8910=LINE('',#53010,#11457);
#8911=LINE('',#53016,#11458);
#8912=LINE('',#53022,#11459);
#8913=LINE('',#53029,#11460);
#8914=LINE('',#53035,#11461);
#8915=LINE('',#53042,#11462);
#8916=LINE('',#53048,#11463);
#8917=LINE('',#53055,#11464);
#8918=LINE('',#53061,#11465);
#8919=LINE('',#53065,#11466);
#8920=LINE('',#53080,#11467);
#8921=LINE('',#53087,#11468);
#8922=LINE('',#53094,#11469);
#8923=LINE('',#53100,#11470);
#8924=LINE('',#53107,#11471);
#8925=LINE('',#53110,#11472);
#8926=LINE('',#53116,#11473);
#8927=LINE('',#53123,#11474);
#8928=LINE('',#53131,#11475);
#8929=LINE('',#53136,#11476);
#8930=LINE('',#53140,#11477);
#8931=LINE('',#53147,#11478);
#8932=LINE('',#53152,#11479);
#8933=LINE('',#53154,#11480);
#8934=LINE('',#53155,#11481);
#8935=LINE('',#53157,#11482);
#8936=LINE('',#53158,#11483);
#8937=LINE('',#53162,#11484);
#8938=LINE('',#53167,#11485);
#8939=LINE('',#53168,#11486);
#8940=LINE('',#53170,#11487);
#8941=LINE('',#53171,#11488);
#8942=LINE('',#53190,#11489);
#8943=LINE('',#53226,#11490);
#8944=LINE('',#53264,#11491);
#8945=LINE('',#53266,#11492);
#8946=LINE('',#53267,#11493);
#8947=LINE('',#53270,#11494);
#8948=LINE('',#53271,#11495);
#8949=LINE('',#53274,#11496);
#8950=LINE('',#53275,#11497);
#8951=LINE('',#53278,#11498);
#8952=LINE('',#53279,#11499);
#8953=LINE('',#53282,#11500);
#8954=LINE('',#53283,#11501);
#8955=LINE('',#53286,#11502);
#8956=LINE('',#53287,#11503);
#8957=LINE('',#53290,#11504);
#8958=LINE('',#53291,#11505);
#8959=LINE('',#53294,#11506);
#8960=LINE('',#53295,#11507);
#8961=LINE('',#53298,#11508);
#8962=LINE('',#53299,#11509);
#8963=LINE('',#53302,#11510);
#8964=LINE('',#53303,#11511);
#8965=LINE('',#53306,#11512);
#8966=LINE('',#53307,#11513);
#8967=LINE('',#53310,#11514);
#8968=LINE('',#53311,#11515);
#8969=LINE('',#53314,#11516);
#8970=LINE('',#53315,#11517);
#8971=LINE('',#53318,#11518);
#8972=LINE('',#53319,#11519);
#8973=LINE('',#53322,#11520);
#8974=LINE('',#53323,#11521);
#8975=LINE('',#53325,#11522);
#8976=LINE('',#53328,#11523);
#8977=LINE('',#53330,#11524);
#8978=LINE('',#53332,#11525);
#8979=LINE('',#53334,#11526);
#8980=LINE('',#53336,#11527);
#8981=LINE('',#53338,#11528);
#8982=LINE('',#53340,#11529);
#8983=LINE('',#53342,#11530);
#8984=LINE('',#53344,#11531);
#8985=LINE('',#53346,#11532);
#8986=LINE('',#53348,#11533);
#8987=LINE('',#53350,#11534);
#8988=LINE('',#53352,#11535);
#8989=LINE('',#53360,#11536);
#8990=LINE('',#53363,#11537);
#8991=LINE('',#53366,#11538);
#8992=LINE('',#53368,#11539);
#8993=LINE('',#53370,#11540);
#8994=LINE('',#53372,#11541);
#8995=LINE('',#53374,#11542);
#8996=LINE('',#53376,#11543);
#8997=LINE('',#53378,#11544);
#8998=LINE('',#53380,#11545);
#8999=LINE('',#53382,#11546);
#9000=LINE('',#53384,#11547);
#9001=LINE('',#53385,#11548);
#9002=LINE('',#53392,#11549);
#9003=LINE('',#53394,#11550);
#9004=LINE('',#53396,#11551);
#9005=LINE('',#53397,#11552);
#9006=LINE('',#53406,#11553);
#9007=LINE('',#53410,#11554);
#9008=LINE('',#53412,#11555);
#9009=LINE('',#53414,#11556);
#9010=LINE('',#53416,#11557);
#9011=LINE('',#53418,#11558);
#9012=LINE('',#53420,#11559);
#9013=LINE('',#53422,#11560);
#9014=LINE('',#53424,#11561);
#9015=LINE('',#53428,#11562);
#9016=LINE('',#53430,#11563);
#9017=LINE('',#53432,#11564);
#9018=LINE('',#53433,#11565);
#9019=LINE('',#53442,#11566);
#9020=LINE('',#53502,#11567);
#9021=LINE('',#53504,#11568);
#9022=LINE('',#53505,#11569);
#9023=LINE('',#53508,#11570);
#9024=LINE('',#53510,#11571);
#9025=LINE('',#53513,#11572);
#9026=LINE('',#53515,#11573);
#9027=LINE('',#53517,#11574);
#9028=LINE('',#53518,#11575);
#9029=LINE('',#53524,#11576);
#9030=LINE('',#53592,#11577);
#9031=LINE('',#53593,#11578);
#9032=LINE('',#53598,#11579);
#9033=LINE('',#53599,#11580);
#9034=LINE('',#53607,#11581);
#9035=LINE('',#53609,#11582);
#9036=LINE('',#53610,#11583);
#9037=LINE('',#53620,#11584);
#9038=LINE('',#53622,#11585);
#9039=LINE('',#53624,#11586);
#9040=LINE('',#53625,#11587);
#9041=LINE('',#53627,#11588);
#9042=LINE('',#53628,#11589);
#9043=LINE('',#53630,#11590);
#9044=LINE('',#53632,#11591);
#9045=LINE('',#53633,#11592);
#9046=LINE('',#53635,#11593);
#9047=LINE('',#53636,#11594);
#9048=LINE('',#53638,#11595);
#9049=LINE('',#53640,#11596);
#9050=LINE('',#53641,#11597);
#9051=LINE('',#53643,#11598);
#9052=LINE('',#53644,#11599);
#9053=LINE('',#53646,#11600);
#9054=LINE('',#53648,#11601);
#9055=LINE('',#53649,#11602);
#9056=LINE('',#53651,#11603);
#9057=LINE('',#53652,#11604);
#9058=LINE('',#53655,#11605);
#9059=LINE('',#53659,#11606);
#9060=LINE('',#53662,#11607);
#9061=LINE('',#53663,#11608);
#9062=LINE('',#53665,#11609);
#9063=LINE('',#53666,#11610);
#9064=LINE('',#53669,#11611);
#9065=LINE('',#53671,#11612);
#9066=LINE('',#53672,#11613);
#9067=LINE('',#53674,#11614);
#9068=LINE('',#53676,#11615);
#9069=LINE('',#53678,#11616);
#9070=LINE('',#53679,#11617);
#9071=LINE('',#53687,#11618);
#9072=LINE('',#53689,#11619);
#9073=LINE('',#53691,#11620);
#9074=LINE('',#53692,#11621);
#9075=LINE('',#53704,#11622);
#9076=LINE('',#53707,#11623);
#9077=LINE('',#53714,#11624);
#9078=LINE('',#53717,#11625);
#9079=LINE('',#53724,#11626);
#9080=LINE('',#53727,#11627);
#9081=LINE('',#53734,#11628);
#9082=LINE('',#53737,#11629);
#9083=LINE('',#53742,#11630);
#9084=LINE('',#53744,#11631);
#9085=LINE('',#53746,#11632);
#9086=LINE('',#53748,#11633);
#9087=LINE('',#53750,#11634);
#9088=LINE('',#53754,#11635);
#9089=LINE('',#53756,#11636);
#9090=LINE('',#53757,#11637);
#9091=LINE('',#53759,#11638);
#9092=LINE('',#53761,#11639);
#9093=LINE('',#53765,#11640);
#9094=LINE('',#53766,#11641);
#9095=LINE('',#53768,#11642);
#9096=LINE('',#53771,#11643);
#9097=LINE('',#53774,#11644);
#9098=LINE('',#53775,#11645);
#9099=LINE('',#53777,#11646);
#9100=LINE('',#53779,#11647);
#9101=LINE('',#53785,#11648);
#9102=LINE('',#53787,#11649);
#9103=LINE('',#53789,#11650);
#9104=LINE('',#53790,#11651);
#9105=LINE('',#53795,#11652);
#9106=LINE('',#53799,#11653);
#9107=LINE('',#53801,#11654);
#9108=LINE('',#53802,#11655);
#9109=LINE('',#53807,#11656);
#9110=LINE('',#53812,#11657);
#9111=LINE('',#53814,#11658);
#9112=LINE('',#53816,#11659);
#9113=LINE('',#53817,#11660);
#9114=LINE('',#53822,#11661);
#9115=LINE('',#53826,#11662);
#9116=LINE('',#53828,#11663);
#9117=LINE('',#53829,#11664);
#9118=LINE('',#53834,#11665);
#9119=LINE('',#53838,#11666);
#9120=LINE('',#53840,#11667);
#9121=LINE('',#53841,#11668);
#9122=LINE('',#53847,#11669);
#9123=LINE('',#53850,#11670);
#9124=LINE('',#53852,#11671);
#9125=LINE('',#53853,#11672);
#9126=LINE('',#53859,#11673);
#9127=LINE('',#53861,#11674);
#9128=LINE('',#53862,#11675);
#9129=LINE('',#53867,#11676);
#9130=LINE('',#53871,#11677);
#9131=LINE('',#53873,#11678);
#9132=LINE('',#53874,#11679);
#9133=LINE('',#53883,#11680);
#9134=LINE('',#53885,#11681);
#9135=LINE('',#53887,#11682);
#9136=LINE('',#53888,#11683);
#9137=LINE('',#53893,#11684);
#9138=LINE('',#53897,#11685);
#9139=LINE('',#53899,#11686);
#9140=LINE('',#53900,#11687);
#9141=LINE('',#53905,#11688);
#9142=LINE('',#53910,#11689);
#9143=LINE('',#53912,#11690);
#9144=LINE('',#53914,#11691);
#9145=LINE('',#53915,#11692);
#9146=LINE('',#53920,#11693);
#9147=LINE('',#53924,#11694);
#9148=LINE('',#53926,#11695);
#9149=LINE('',#53927,#11696);
#9150=LINE('',#53932,#11697);
#9151=LINE('',#53936,#11698);
#9152=LINE('',#53938,#11699);
#9153=LINE('',#53939,#11700);
#9154=LINE('',#53945,#11701);
#9155=LINE('',#53948,#11702);
#9156=LINE('',#53950,#11703);
#9157=LINE('',#53951,#11704);
#9158=LINE('',#53957,#11705);
#9159=LINE('',#53959,#11706);
#9160=LINE('',#53960,#11707);
#9161=LINE('',#53965,#11708);
#9162=LINE('',#53969,#11709);
#9163=LINE('',#53971,#11710);
#9164=LINE('',#53972,#11711);
#9165=LINE('',#53981,#11712);
#9166=LINE('',#53983,#11713);
#9167=LINE('',#53985,#11714);
#9168=LINE('',#53986,#11715);
#9169=LINE('',#53991,#11716);
#9170=LINE('',#53995,#11717);
#9171=LINE('',#53997,#11718);
#9172=LINE('',#53998,#11719);
#9173=LINE('',#54003,#11720);
#9174=LINE('',#54008,#11721);
#9175=LINE('',#54010,#11722);
#9176=LINE('',#54012,#11723);
#9177=LINE('',#54013,#11724);
#9178=LINE('',#54018,#11725);
#9179=LINE('',#54022,#11726);
#9180=LINE('',#54024,#11727);
#9181=LINE('',#54025,#11728);
#9182=LINE('',#54030,#11729);
#9183=LINE('',#54034,#11730);
#9184=LINE('',#54036,#11731);
#9185=LINE('',#54037,#11732);
#9186=LINE('',#54043,#11733);
#9187=LINE('',#54046,#11734);
#9188=LINE('',#54048,#11735);
#9189=LINE('',#54049,#11736);
#9190=LINE('',#54055,#11737);
#9191=LINE('',#54057,#11738);
#9192=LINE('',#54058,#11739);
#9193=LINE('',#54063,#11740);
#9194=LINE('',#54067,#11741);
#9195=LINE('',#54069,#11742);
#9196=LINE('',#54070,#11743);
#9197=LINE('',#54079,#11744);
#9198=LINE('',#54081,#11745);
#9199=LINE('',#54083,#11746);
#9200=LINE('',#54084,#11747);
#9201=LINE('',#54089,#11748);
#9202=LINE('',#54093,#11749);
#9203=LINE('',#54095,#11750);
#9204=LINE('',#54096,#11751);
#9205=LINE('',#54101,#11752);
#9206=LINE('',#54106,#11753);
#9207=LINE('',#54108,#11754);
#9208=LINE('',#54110,#11755);
#9209=LINE('',#54111,#11756);
#9210=LINE('',#54116,#11757);
#9211=LINE('',#54120,#11758);
#9212=LINE('',#54122,#11759);
#9213=LINE('',#54123,#11760);
#9214=LINE('',#54128,#11761);
#9215=LINE('',#54132,#11762);
#9216=LINE('',#54134,#11763);
#9217=LINE('',#54135,#11764);
#9218=LINE('',#54141,#11765);
#9219=LINE('',#54144,#11766);
#9220=LINE('',#54146,#11767);
#9221=LINE('',#54147,#11768);
#9222=LINE('',#54153,#11769);
#9223=LINE('',#54155,#11770);
#9224=LINE('',#54156,#11771);
#9225=LINE('',#54161,#11772);
#9226=LINE('',#54165,#11773);
#9227=LINE('',#54167,#11774);
#9228=LINE('',#54168,#11775);
#9229=LINE('',#54179,#11776);
#9230=LINE('',#54183,#11777);
#9231=LINE('',#54187,#11778);
#9232=LINE('',#54190,#11779);
#9233=LINE('',#54193,#11780);
#9234=LINE('',#54197,#11781);
#9235=LINE('',#54201,#11782);
#9236=LINE('',#54205,#11783);
#9237=LINE('',#54209,#11784);
#9238=LINE('',#54211,#11785);
#9239=LINE('',#54212,#11786);
#9240=LINE('',#54215,#11787);
#9241=LINE('',#54219,#11788);
#9242=LINE('',#54220,#11789);
#9243=LINE('',#54223,#11790);
#9244=LINE('',#54227,#11791);
#9245=LINE('',#54230,#11792);
#9246=LINE('',#54233,#11793);
#9247=LINE('',#54236,#11794);
#9248=LINE('',#54239,#11795);
#9249=LINE('',#54240,#11796);
#9250=LINE('',#54242,#11797);
#9251=LINE('',#54246,#11798);
#9252=LINE('',#54249,#11799);
#9253=LINE('',#54251,#11800);
#9254=LINE('',#54255,#11801);
#9255=LINE('',#54258,#11802);
#9256=LINE('',#54260,#11803);
#9257=LINE('',#54262,#11804);
#9258=LINE('',#54264,#11805);
#9259=LINE('',#54268,#11806);
#9260=LINE('',#54270,#11807);
#9261=LINE('',#54277,#11808);
#9262=LINE('',#54281,#11809);
#9263=LINE('',#54285,#11810);
#9264=LINE('',#54288,#11811);
#9265=LINE('',#54291,#11812);
#9266=LINE('',#54295,#11813);
#9267=LINE('',#54299,#11814);
#9268=LINE('',#54303,#11815);
#9269=LINE('',#54307,#11816);
#9270=LINE('',#54309,#11817);
#9271=LINE('',#54310,#11818);
#9272=LINE('',#54313,#11819);
#9273=LINE('',#54317,#11820);
#9274=LINE('',#54318,#11821);
#9275=LINE('',#54321,#11822);
#9276=LINE('',#54325,#11823);
#9277=LINE('',#54328,#11824);
#9278=LINE('',#54331,#11825);
#9279=LINE('',#54332,#11826);
#9280=LINE('',#54335,#11827);
#9281=LINE('',#54339,#11828);
#9282=LINE('',#54340,#11829);
#9283=LINE('',#54345,#11830);
#9284=LINE('',#54348,#11831);
#9285=LINE('',#54350,#11832);
#9286=LINE('',#54354,#11833);
#9287=LINE('',#54357,#11834);
#9288=LINE('',#54359,#11835);
#9289=LINE('',#54361,#11836);
#9290=LINE('',#54363,#11837);
#9291=LINE('',#54366,#11838);
#9292=LINE('',#54368,#11839);
#9293=LINE('',#54373,#11840);
#9294=LINE('',#54377,#11841);
#9295=LINE('',#54381,#11842);
#9296=LINE('',#54385,#11843);
#9297=LINE('',#54389,#11844);
#9298=LINE('',#54393,#11845);
#9299=LINE('',#54397,#11846);
#9300=LINE('',#54401,#11847);
#9301=LINE('',#54405,#11848);
#9302=LINE('',#54407,#11849);
#9303=LINE('',#54408,#11850);
#9304=LINE('',#54411,#11851);
#9305=LINE('',#54415,#11852);
#9306=LINE('',#54416,#11853);
#9307=LINE('',#54419,#11854);
#9308=LINE('',#54423,#11855);
#9309=LINE('',#54425,#11856);
#9310=LINE('',#54426,#11857);
#9311=LINE('',#54429,#11858);
#9312=LINE('',#54433,#11859);
#9313=LINE('',#54434,#11860);
#9314=LINE('',#54437,#11861);
#9315=LINE('',#54441,#11862);
#9316=LINE('',#54445,#11863);
#9317=LINE('',#54448,#11864);
#9318=LINE('',#54452,#11865);
#9319=LINE('',#54455,#11866);
#9320=LINE('',#54457,#11867);
#9321=LINE('',#54459,#11868);
#9322=LINE('',#54461,#11869);
#9323=LINE('',#54464,#11870);
#9324=LINE('',#54466,#11871);
#9325=LINE('',#54471,#11872);
#9326=LINE('',#54475,#11873);
#9327=LINE('',#54479,#11874);
#9328=LINE('',#54483,#11875);
#9329=LINE('',#54487,#11876);
#9330=LINE('',#54491,#11877);
#9331=LINE('',#54495,#11878);
#9332=LINE('',#54499,#11879);
#9333=LINE('',#54503,#11880);
#9334=LINE('',#54505,#11881);
#9335=LINE('',#54506,#11882);
#9336=LINE('',#54509,#11883);
#9337=LINE('',#54513,#11884);
#9338=LINE('',#54514,#11885);
#9339=LINE('',#54517,#11886);
#9340=LINE('',#54521,#11887);
#9341=LINE('',#54523,#11888);
#9342=LINE('',#54524,#11889);
#9343=LINE('',#54527,#11890);
#9344=LINE('',#54531,#11891);
#9345=LINE('',#54532,#11892);
#9346=LINE('',#54535,#11893);
#9347=LINE('',#54539,#11894);
#9348=LINE('',#54543,#11895);
#9349=LINE('',#54546,#11896);
#9350=LINE('',#54550,#11897);
#9351=LINE('',#54553,#11898);
#9352=LINE('',#54555,#11899);
#9353=LINE('',#54557,#11900);
#9354=LINE('',#54559,#11901);
#9355=LINE('',#54562,#11902);
#9356=LINE('',#54564,#11903);
#9357=LINE('',#54569,#11904);
#9358=LINE('',#54571,#11905);
#9359=LINE('',#54573,#11906);
#9360=LINE('',#54574,#11907);
#9361=LINE('',#54579,#11908);
#9362=LINE('',#54583,#11909);
#9363=LINE('',#54585,#11910);
#9364=LINE('',#54586,#11911);
#9365=LINE('',#54591,#11912);
#9366=LINE('',#54596,#11913);
#9367=LINE('',#54598,#11914);
#9368=LINE('',#54600,#11915);
#9369=LINE('',#54601,#11916);
#9370=LINE('',#54606,#11917);
#9371=LINE('',#54610,#11918);
#9372=LINE('',#54612,#11919);
#9373=LINE('',#54613,#11920);
#9374=LINE('',#54618,#11921);
#9375=LINE('',#54622,#11922);
#9376=LINE('',#54624,#11923);
#9377=LINE('',#54625,#11924);
#9378=LINE('',#54631,#11925);
#9379=LINE('',#54634,#11926);
#9380=LINE('',#54636,#11927);
#9381=LINE('',#54637,#11928);
#9382=LINE('',#54643,#11929);
#9383=LINE('',#54645,#11930);
#9384=LINE('',#54646,#11931);
#9385=LINE('',#54651,#11932);
#9386=LINE('',#54655,#11933);
#9387=LINE('',#54657,#11934);
#9388=LINE('',#54658,#11935);
#9389=LINE('',#54667,#11936);
#9390=LINE('',#54669,#11937);
#9391=LINE('',#54671,#11938);
#9392=LINE('',#54672,#11939);
#9393=LINE('',#54677,#11940);
#9394=LINE('',#54681,#11941);
#9395=LINE('',#54683,#11942);
#9396=LINE('',#54684,#11943);
#9397=LINE('',#54689,#11944);
#9398=LINE('',#54694,#11945);
#9399=LINE('',#54696,#11946);
#9400=LINE('',#54698,#11947);
#9401=LINE('',#54699,#11948);
#9402=LINE('',#54704,#11949);
#9403=LINE('',#54708,#11950);
#9404=LINE('',#54710,#11951);
#9405=LINE('',#54711,#11952);
#9406=LINE('',#54716,#11953);
#9407=LINE('',#54720,#11954);
#9408=LINE('',#54722,#11955);
#9409=LINE('',#54723,#11956);
#9410=LINE('',#54729,#11957);
#9411=LINE('',#54732,#11958);
#9412=LINE('',#54734,#11959);
#9413=LINE('',#54735,#11960);
#9414=LINE('',#54741,#11961);
#9415=LINE('',#54743,#11962);
#9416=LINE('',#54744,#11963);
#9417=LINE('',#54749,#11964);
#9418=LINE('',#54753,#11965);
#9419=LINE('',#54755,#11966);
#9420=LINE('',#54756,#11967);
#9421=LINE('',#54765,#11968);
#9422=LINE('',#54767,#11969);
#9423=LINE('',#54769,#11970);
#9424=LINE('',#54770,#11971);
#9425=LINE('',#54775,#11972);
#9426=LINE('',#54779,#11973);
#9427=LINE('',#54781,#11974);
#9428=LINE('',#54782,#11975);
#9429=LINE('',#54787,#11976);
#9430=LINE('',#54792,#11977);
#9431=LINE('',#54794,#11978);
#9432=LINE('',#54796,#11979);
#9433=LINE('',#54797,#11980);
#9434=LINE('',#54802,#11981);
#9435=LINE('',#54806,#11982);
#9436=LINE('',#54808,#11983);
#9437=LINE('',#54809,#11984);
#9438=LINE('',#54814,#11985);
#9439=LINE('',#54818,#11986);
#9440=LINE('',#54820,#11987);
#9441=LINE('',#54821,#11988);
#9442=LINE('',#54827,#11989);
#9443=LINE('',#54830,#11990);
#9444=LINE('',#54832,#11991);
#9445=LINE('',#54833,#11992);
#9446=LINE('',#54839,#11993);
#9447=LINE('',#54841,#11994);
#9448=LINE('',#54842,#11995);
#9449=LINE('',#54847,#11996);
#9450=LINE('',#54851,#11997);
#9451=LINE('',#54853,#11998);
#9452=LINE('',#54854,#11999);
#9453=LINE('',#54865,#12000);
#9454=LINE('',#54868,#12001);
#9455=LINE('',#54871,#12002);
#9456=LINE('',#54873,#12003);
#9457=LINE('',#54874,#12004);
#9458=LINE('',#54879,#12005);
#9459=LINE('',#54883,#12006);
#9460=LINE('',#54885,#12007);
#9461=LINE('',#54886,#12008);
#9462=LINE('',#54891,#12009);
#9463=LINE('',#54895,#12010);
#9464=LINE('',#54897,#12011);
#9465=LINE('',#54898,#12012);
#9466=LINE('',#54903,#12013);
#9467=LINE('',#54906,#12014);
#9468=LINE('',#54907,#12015);
#9469=LINE('',#54913,#12016);
#9470=LINE('',#54916,#12017);
#9471=LINE('',#54919,#12018);
#9472=LINE('',#54921,#12019);
#9473=LINE('',#54922,#12020);
#9474=LINE('',#54928,#12021);
#9475=LINE('',#54931,#12022);
#9476=LINE('',#54933,#12023);
#9477=LINE('',#54934,#12024);
#9478=LINE('',#54940,#12025);
#9479=LINE('',#54943,#12026);
#9480=LINE('',#54945,#12027);
#9481=LINE('',#54946,#12028);
#9482=LINE('',#54952,#12029);
#9483=LINE('',#54954,#12030);
#9484=LINE('',#54955,#12031);
#9485=LINE('',#54963,#12032);
#9486=LINE('',#54966,#12033);
#9487=LINE('',#54969,#12034);
#9488=LINE('',#54971,#12035);
#9489=LINE('',#54972,#12036);
#9490=LINE('',#54977,#12037);
#9491=LINE('',#54981,#12038);
#9492=LINE('',#54983,#12039);
#9493=LINE('',#54984,#12040);
#9494=LINE('',#54989,#12041);
#9495=LINE('',#54993,#12042);
#9496=LINE('',#54995,#12043);
#9497=LINE('',#54996,#12044);
#9498=LINE('',#55001,#12045);
#9499=LINE('',#55004,#12046);
#9500=LINE('',#55005,#12047);
#9501=LINE('',#55011,#12048);
#9502=LINE('',#55014,#12049);
#9503=LINE('',#55017,#12050);
#9504=LINE('',#55019,#12051);
#9505=LINE('',#55020,#12052);
#9506=LINE('',#55026,#12053);
#9507=LINE('',#55029,#12054);
#9508=LINE('',#55031,#12055);
#9509=LINE('',#55032,#12056);
#9510=LINE('',#55038,#12057);
#9511=LINE('',#55041,#12058);
#9512=LINE('',#55043,#12059);
#9513=LINE('',#55044,#12060);
#9514=LINE('',#55050,#12061);
#9515=LINE('',#55052,#12062);
#9516=LINE('',#55053,#12063);
#9517=LINE('',#55061,#12064);
#9518=LINE('',#55064,#12065);
#9519=LINE('',#55067,#12066);
#9520=LINE('',#55069,#12067);
#9521=LINE('',#55070,#12068);
#9522=LINE('',#55075,#12069);
#9523=LINE('',#55079,#12070);
#9524=LINE('',#55081,#12071);
#9525=LINE('',#55082,#12072);
#9526=LINE('',#55087,#12073);
#9527=LINE('',#55091,#12074);
#9528=LINE('',#55093,#12075);
#9529=LINE('',#55094,#12076);
#9530=LINE('',#55099,#12077);
#9531=LINE('',#55102,#12078);
#9532=LINE('',#55103,#12079);
#9533=LINE('',#55109,#12080);
#9534=LINE('',#55112,#12081);
#9535=LINE('',#55115,#12082);
#9536=LINE('',#55117,#12083);
#9537=LINE('',#55118,#12084);
#9538=LINE('',#55124,#12085);
#9539=LINE('',#55127,#12086);
#9540=LINE('',#55129,#12087);
#9541=LINE('',#55130,#12088);
#9542=LINE('',#55136,#12089);
#9543=LINE('',#55139,#12090);
#9544=LINE('',#55141,#12091);
#9545=LINE('',#55142,#12092);
#9546=LINE('',#55148,#12093);
#9547=LINE('',#55150,#12094);
#9548=LINE('',#55151,#12095);
#9549=LINE('',#55159,#12096);
#9550=LINE('',#55162,#12097);
#9551=LINE('',#55165,#12098);
#9552=LINE('',#55167,#12099);
#9553=LINE('',#55168,#12100);
#9554=LINE('',#55173,#12101);
#9555=LINE('',#55177,#12102);
#9556=LINE('',#55179,#12103);
#9557=LINE('',#55180,#12104);
#9558=LINE('',#55185,#12105);
#9559=LINE('',#55189,#12106);
#9560=LINE('',#55191,#12107);
#9561=LINE('',#55192,#12108);
#9562=LINE('',#55197,#12109);
#9563=LINE('',#55200,#12110);
#9564=LINE('',#55201,#12111);
#9565=LINE('',#55207,#12112);
#9566=LINE('',#55210,#12113);
#9567=LINE('',#55213,#12114);
#9568=LINE('',#55215,#12115);
#9569=LINE('',#55216,#12116);
#9570=LINE('',#55222,#12117);
#9571=LINE('',#55225,#12118);
#9572=LINE('',#55227,#12119);
#9573=LINE('',#55228,#12120);
#9574=LINE('',#55234,#12121);
#9575=LINE('',#55237,#12122);
#9576=LINE('',#55239,#12123);
#9577=LINE('',#55240,#12124);
#9578=LINE('',#55246,#12125);
#9579=LINE('',#55248,#12126);
#9580=LINE('',#55249,#12127);
#9581=LINE('',#55258,#12128);
#9582=LINE('',#55264,#12129);
#9583=LINE('',#55270,#12130);
#9584=LINE('',#55276,#12131);
#9585=LINE('',#55282,#12132);
#9586=LINE('',#55288,#12133);
#9587=LINE('',#55294,#12134);
#9588=LINE('',#55300,#12135);
#9589=LINE('',#55306,#12136);
#9590=LINE('',#55312,#12137);
#9591=LINE('',#55318,#12138);
#9592=LINE('',#55324,#12139);
#9593=LINE('',#55330,#12140);
#9594=LINE('',#55336,#12141);
#9595=LINE('',#55342,#12142);
#9596=LINE('',#55348,#12143);
#9597=LINE('',#55353,#12144);
#9598=LINE('',#55355,#12145);
#9599=LINE('',#55357,#12146);
#9600=LINE('',#55358,#12147);
#9601=LINE('',#55361,#12148);
#9602=LINE('',#55363,#12149);
#9603=LINE('',#55364,#12150);
#9604=LINE('',#55367,#12151);
#9605=LINE('',#55369,#12152);
#9606=LINE('',#55370,#12153);
#9607=LINE('',#55372,#12154);
#9608=LINE('',#55373,#12155);
#9609=LINE('',#55377,#12156);
#9610=LINE('',#55379,#12157);
#9611=LINE('',#55381,#12158);
#9612=LINE('',#55382,#12159);
#9613=LINE('',#55385,#12160);
#9614=LINE('',#55387,#12161);
#9615=LINE('',#55388,#12162);
#9616=LINE('',#55391,#12163);
#9617=LINE('',#55392,#12164);
#9618=LINE('',#55395,#12165);
#9619=LINE('',#55396,#12166);
#9620=LINE('',#55398,#12167);
#9621=LINE('',#55404,#12168);
#9622=LINE('',#55406,#12169);
#9623=LINE('',#55408,#12170);
#9624=LINE('',#55409,#12171);
#9625=LINE('',#55419,#12172);
#9626=LINE('',#55421,#12173);
#9627=LINE('',#55423,#12174);
#9628=LINE('',#55424,#12175);
#9629=LINE('',#55432,#12176);
#9630=LINE('',#55433,#12177);
#9631=LINE('',#55437,#12178);
#9632=LINE('',#55440,#12179);
#9633=LINE('',#55444,#12180);
#9634=LINE('',#55447,#12181);
#9635=LINE('',#55451,#12182);
#9636=LINE('',#55454,#12183);
#9637=LINE('',#55458,#12184);
#9638=LINE('',#55461,#12185);
#9639=LINE('',#55465,#12186);
#9640=LINE('',#55468,#12187);
#9641=LINE('',#55472,#12188);
#9642=LINE('',#55475,#12189);
#9643=LINE('',#55480,#12190);
#9644=LINE('',#55486,#12191);
#9645=LINE('',#55492,#12192);
#9646=LINE('',#55498,#12193);
#9647=LINE('',#55504,#12194);
#9648=LINE('',#55510,#12195);
#9649=LINE('',#55516,#12196);
#9650=LINE('',#55522,#12197);
#9651=LINE('',#55528,#12198);
#9652=LINE('',#55534,#12199);
#9653=LINE('',#55537,#12200);
#9654=LINE('',#55539,#12201);
#9655=LINE('',#55545,#12202);
#9656=LINE('',#55547,#12203);
#9657=LINE('',#55549,#12204);
#9658=LINE('',#55550,#12205);
#9659=LINE('',#55560,#12206);
#9660=LINE('',#55562,#12207);
#9661=LINE('',#55564,#12208);
#9662=LINE('',#55565,#12209);
#9663=LINE('',#55573,#12210);
#9664=LINE('',#55574,#12211);
#9665=LINE('',#55578,#12212);
#9666=LINE('',#55581,#12213);
#9667=LINE('',#55585,#12214);
#9668=LINE('',#55588,#12215);
#9669=LINE('',#55592,#12216);
#9670=LINE('',#55595,#12217);
#9671=LINE('',#55599,#12218);
#9672=LINE('',#55602,#12219);
#9673=LINE('',#55606,#12220);
#9674=LINE('',#55609,#12221);
#9675=LINE('',#55613,#12222);
#9676=LINE('',#55616,#12223);
#9677=LINE('',#55621,#12224);
#9678=LINE('',#55627,#12225);
#9679=LINE('',#55633,#12226);
#9680=LINE('',#55639,#12227);
#9681=LINE('',#55645,#12228);
#9682=LINE('',#55651,#12229);
#9683=LINE('',#55657,#12230);
#9684=LINE('',#55663,#12231);
#9685=LINE('',#55669,#12232);
#9686=LINE('',#55675,#12233);
#9687=LINE('',#55678,#12234);
#9688=LINE('',#55680,#12235);
#9689=LINE('',#55687,#12236);
#9690=LINE('',#55693,#12237);
#9691=LINE('',#55699,#12238);
#9692=LINE('',#55705,#12239);
#9693=LINE('',#55711,#12240);
#9694=LINE('',#55717,#12241);
#9695=LINE('',#55722,#12242);
#9696=LINE('',#55724,#12243);
#9697=LINE('',#55726,#12244);
#9698=LINE('',#55727,#12245);
#9699=LINE('',#55730,#12246);
#9700=LINE('',#55732,#12247);
#9701=LINE('',#55733,#12248);
#9702=LINE('',#55736,#12249);
#9703=LINE('',#55738,#12250);
#9704=LINE('',#55739,#12251);
#9705=LINE('',#55741,#12252);
#9706=LINE('',#55742,#12253);
#9707=LINE('',#55749,#12254);
#9708=LINE('',#55751,#12255);
#9709=LINE('',#55753,#12256);
#9710=LINE('',#55754,#12257);
#9711=LINE('',#55757,#12258);
#9712=LINE('',#55759,#12259);
#9713=LINE('',#55760,#12260);
#9714=LINE('',#55763,#12261);
#9715=LINE('',#55765,#12262);
#9716=LINE('',#55767,#12263);
#9717=LINE('',#55771,#12264);
#9718=LINE('',#55772,#12265);
#9719=LINE('',#55775,#12266);
#9720=LINE('',#55777,#12267);
#9721=LINE('',#55781,#12268);
#9722=LINE('',#55782,#12269);
#9723=LINE('',#55784,#12270);
#9724=LINE('',#55786,#12271);
#9725=LINE('',#55787,#12272);
#9726=LINE('',#55789,#12273);
#9727=LINE('',#55791,#12274);
#9728=LINE('',#55793,#12275);
#9729=LINE('',#55801,#12276);
#9730=LINE('',#55807,#12277);
#9731=LINE('',#55813,#12278);
#9732=LINE('',#55819,#12279);
#9733=LINE('',#55824,#12280);
#9734=LINE('',#55826,#12281);
#9735=LINE('',#55828,#12282);
#9736=LINE('',#55829,#12283);
#9737=LINE('',#55832,#12284);
#9738=LINE('',#55834,#12285);
#9739=LINE('',#55835,#12286);
#9740=LINE('',#55838,#12287);
#9741=LINE('',#55840,#12288);
#9742=LINE('',#55841,#12289);
#9743=LINE('',#55843,#12290);
#9744=LINE('',#55844,#12291);
#9745=LINE('',#55848,#12292);
#9746=LINE('',#55850,#12293);
#9747=LINE('',#55852,#12294);
#9748=LINE('',#55853,#12295);
#9749=LINE('',#55856,#12296);
#9750=LINE('',#55858,#12297);
#9751=LINE('',#55859,#12298);
#9752=LINE('',#55862,#12299);
#9753=LINE('',#55864,#12300);
#9754=LINE('',#55865,#12301);
#9755=LINE('',#55867,#12302);
#9756=LINE('',#55868,#12303);
#9757=LINE('',#55892,#12304);
#9758=LINE('',#55907,#12305);
#9759=LINE('',#55942,#12306);
#9760=LINE('',#55945,#12307);
#9761=LINE('',#55948,#12308);
#9762=LINE('',#55950,#12309);
#9763=LINE('',#55951,#12310);
#9764=LINE('',#55954,#12311);
#9765=LINE('',#55956,#12312);
#9766=LINE('',#55957,#12313);
#9767=LINE('',#55993,#12314);
#9768=LINE('',#56007,#12315);
#9769=LINE('',#56016,#12316);
#9770=LINE('',#56021,#12317);
#9771=LINE('',#56028,#12318);
#9772=LINE('',#56031,#12319);
#9773=LINE('',#56037,#12320);
#9774=LINE('',#56042,#12321);
#9775=LINE('',#56046,#12322);
#9776=LINE('',#56059,#12323);
#9777=LINE('',#56061,#12324);
#9778=LINE('',#56062,#12325);
#9779=LINE('',#56065,#12326);
#9780=LINE('',#56066,#12327);
#9781=LINE('',#56085,#12328);
#9782=LINE('',#56096,#12329);
#9783=LINE('',#56099,#12330);
#9784=LINE('',#56110,#12331);
#9785=LINE('',#56125,#12332);
#9786=LINE('',#56144,#12333);
#9787=LINE('',#56148,#12334);
#9788=LINE('',#56152,#12335);
#9789=LINE('',#56173,#12336);
#9790=LINE('',#56199,#12337);
#9791=LINE('',#56203,#12338);
#9792=LINE('',#56210,#12339);
#9793=LINE('',#56212,#12340);
#9794=LINE('',#56213,#12341);
#9795=LINE('',#56217,#12342);
#9796=LINE('',#56220,#12343);
#9797=LINE('',#56221,#12344);
#9798=LINE('',#56231,#12345);
#9799=LINE('',#56240,#12346);
#9800=LINE('',#56250,#12347);
#9801=LINE('',#56266,#12348);
#9802=LINE('',#56269,#12349);
#9803=LINE('',#56275,#12350);
#9804=LINE('',#56280,#12351);
#9805=LINE('',#56284,#12352);
#9806=LINE('',#56297,#12353);
#9807=LINE('',#56299,#12354);
#9808=LINE('',#56300,#12355);
#9809=LINE('',#56303,#12356);
#9810=LINE('',#56304,#12357);
#9811=LINE('',#56329,#12358);
#9812=LINE('',#56332,#12359);
#9813=LINE('',#56343,#12360);
#9814=LINE('',#56345,#12361);
#9815=LINE('',#56347,#12362);
#9816=LINE('',#56348,#12363);
#9817=LINE('',#56351,#12364);
#9818=LINE('',#56353,#12365);
#9819=LINE('',#56354,#12366);
#9820=LINE('',#56358,#12367);
#9821=LINE('',#56359,#12368);
#9822=LINE('',#56360,#12369);
#9823=LINE('',#56370,#12370);
#9824=LINE('',#56377,#12371);
#9825=LINE('',#56383,#12372);
#9826=LINE('',#56415,#12373);
#9827=LINE('',#56420,#12374);
#9828=LINE('',#56422,#12375);
#9829=LINE('',#56424,#12376);
#9830=LINE('',#56818,#12377);
#9831=LINE('',#56819,#12378);
#9832=LINE('',#56820,#12379);
#9833=LINE('',#56823,#12380);
#9834=LINE('',#56824,#12381);
#9835=LINE('',#56828,#12382);
#9836=LINE('',#56830,#12383);
#9837=LINE('',#56833,#12384);
#9838=LINE('',#56836,#12385);
#9839=LINE('',#56840,#12386);
#9840=LINE('',#56843,#12387);
#9841=LINE('',#56847,#12388);
#9842=LINE('',#56850,#12389);
#9843=LINE('',#56854,#12390);
#9844=LINE('',#56857,#12391);
#9845=LINE('',#56861,#12392);
#9846=LINE('',#56864,#12393);
#9847=LINE('',#56868,#12394);
#9848=LINE('',#56871,#12395);
#9849=LINE('',#56875,#12396);
#9850=LINE('',#56878,#12397);
#9851=LINE('',#56882,#12398);
#9852=LINE('',#56885,#12399);
#9853=LINE('',#56889,#12400);
#9854=LINE('',#56892,#12401);
#9855=LINE('',#56896,#12402);
#9856=LINE('',#56899,#12403);
#9857=LINE('',#56903,#12404);
#9858=LINE('',#56906,#12405);
#9859=LINE('',#56910,#12406);
#9860=LINE('',#56913,#12407);
#9861=LINE('',#56917,#12408);
#9862=LINE('',#56920,#12409);
#9863=LINE('',#56924,#12410);
#9864=LINE('',#56927,#12411);
#9865=LINE('',#56931,#12412);
#9866=LINE('',#56934,#12413);
#9867=LINE('',#56938,#12414);
#9868=LINE('',#56941,#12415);
#9869=LINE('',#56945,#12416);
#9870=LINE('',#56948,#12417);
#9871=LINE('',#56952,#12418);
#9872=LINE('',#56955,#12419);
#9873=LINE('',#56959,#12420);
#9874=LINE('',#56962,#12421);
#9875=LINE('',#56966,#12422);
#9876=LINE('',#56969,#12423);
#9877=LINE('',#56973,#12424);
#9878=LINE('',#56976,#12425);
#9879=LINE('',#56980,#12426);
#9880=LINE('',#56983,#12427);
#9881=LINE('',#56987,#12428);
#9882=LINE('',#56990,#12429);
#9883=LINE('',#56994,#12430);
#9884=LINE('',#56997,#12431);
#9885=LINE('',#57001,#12432);
#9886=LINE('',#57004,#12433);
#9887=LINE('',#57008,#12434);
#9888=LINE('',#57011,#12435);
#9889=LINE('',#57015,#12436);
#9890=LINE('',#57018,#12437);
#9891=LINE('',#57022,#12438);
#9892=LINE('',#57025,#12439);
#9893=LINE('',#57029,#12440);
#9894=LINE('',#57032,#12441);
#9895=LINE('',#57036,#12442);
#9896=LINE('',#57039,#12443);
#9897=LINE('',#57043,#12444);
#9898=LINE('',#57046,#12445);
#9899=LINE('',#57050,#12446);
#9900=LINE('',#57053,#12447);
#9901=LINE('',#57057,#12448);
#9902=LINE('',#57060,#12449);
#9903=LINE('',#57064,#12450);
#9904=LINE('',#57067,#12451);
#9905=LINE('',#57071,#12452);
#9906=LINE('',#57074,#12453);
#9907=LINE('',#57078,#12454);
#9908=LINE('',#57081,#12455);
#9909=LINE('',#57085,#12456);
#9910=LINE('',#57088,#12457);
#9911=LINE('',#57092,#12458);
#9912=LINE('',#57095,#12459);
#9913=LINE('',#57099,#12460);
#9914=LINE('',#57102,#12461);
#9915=LINE('',#57106,#12462);
#9916=LINE('',#57109,#12463);
#9917=LINE('',#57113,#12464);
#9918=LINE('',#57116,#12465);
#9919=LINE('',#57120,#12466);
#9920=LINE('',#57123,#12467);
#9921=LINE('',#57127,#12468);
#9922=LINE('',#57130,#12469);
#9923=LINE('',#57134,#12470);
#9924=LINE('',#57137,#12471);
#9925=LINE('',#57141,#12472);
#9926=LINE('',#57144,#12473);
#9927=LINE('',#57148,#12474);
#9928=LINE('',#57151,#12475);
#9929=LINE('',#57155,#12476);
#9930=LINE('',#57158,#12477);
#9931=LINE('',#57162,#12478);
#9932=LINE('',#57165,#12479);
#9933=LINE('',#57169,#12480);
#9934=LINE('',#57172,#12481);
#9935=LINE('',#57176,#12482);
#9936=LINE('',#57179,#12483);
#9937=LINE('',#57183,#12484);
#9938=LINE('',#57186,#12485);
#9939=LINE('',#57190,#12486);
#9940=LINE('',#57193,#12487);
#9941=LINE('',#57197,#12488);
#9942=LINE('',#57200,#12489);
#9943=LINE('',#57204,#12490);
#9944=LINE('',#57207,#12491);
#9945=LINE('',#57211,#12492);
#9946=LINE('',#57214,#12493);
#9947=LINE('',#57218,#12494);
#9948=LINE('',#57221,#12495);
#9949=LINE('',#57225,#12496);
#9950=LINE('',#57228,#12497);
#9951=LINE('',#57232,#12498);
#9952=LINE('',#57235,#12499);
#9953=LINE('',#57239,#12500);
#9954=LINE('',#57242,#12501);
#9955=LINE('',#57246,#12502);
#9956=LINE('',#57249,#12503);
#9957=LINE('',#57253,#12504);
#9958=LINE('',#57256,#12505);
#9959=LINE('',#57260,#12506);
#9960=LINE('',#57263,#12507);
#9961=LINE('',#57267,#12508);
#9962=LINE('',#57270,#12509);
#9963=LINE('',#57274,#12510);
#9964=LINE('',#57277,#12511);
#9965=LINE('',#57281,#12512);
#9966=LINE('',#57284,#12513);
#9967=LINE('',#57288,#12514);
#9968=LINE('',#57291,#12515);
#9969=LINE('',#57295,#12516);
#9970=LINE('',#57298,#12517);
#9971=LINE('',#57302,#12518);
#9972=LINE('',#57305,#12519);
#9973=LINE('',#57309,#12520);
#9974=LINE('',#57312,#12521);
#9975=LINE('',#57316,#12522);
#9976=LINE('',#57319,#12523);
#9977=LINE('',#57323,#12524);
#9978=LINE('',#57326,#12525);
#9979=LINE('',#57330,#12526);
#9980=LINE('',#57333,#12527);
#9981=LINE('',#57337,#12528);
#9982=LINE('',#57340,#12529);
#9983=LINE('',#57344,#12530);
#9984=LINE('',#57347,#12531);
#9985=LINE('',#57351,#12532);
#9986=LINE('',#57354,#12533);
#9987=LINE('',#57358,#12534);
#9988=LINE('',#57361,#12535);
#9989=LINE('',#57365,#12536);
#9990=LINE('',#57368,#12537);
#9991=LINE('',#57372,#12538);
#9992=LINE('',#57375,#12539);
#9993=LINE('',#57379,#12540);
#9994=LINE('',#57382,#12541);
#9995=LINE('',#57386,#12542);
#9996=LINE('',#57389,#12543);
#9997=LINE('',#57393,#12544);
#9998=LINE('',#57396,#12545);
#9999=LINE('',#57400,#12546);
#10000=LINE('',#57403,#12547);
#10001=LINE('',#57407,#12548);
#10002=LINE('',#57410,#12549);
#10003=LINE('',#57414,#12550);
#10004=LINE('',#57417,#12551);
#10005=LINE('',#57421,#12552);
#10006=LINE('',#57424,#12553);
#10007=LINE('',#57428,#12554);
#10008=LINE('',#57431,#12555);
#10009=LINE('',#57435,#12556);
#10010=LINE('',#57438,#12557);
#10011=LINE('',#57442,#12558);
#10012=LINE('',#57445,#12559);
#10013=LINE('',#57449,#12560);
#10014=LINE('',#57452,#12561);
#10015=LINE('',#57456,#12562);
#10016=LINE('',#57459,#12563);
#10017=LINE('',#57463,#12564);
#10018=LINE('',#57466,#12565);
#10019=LINE('',#57470,#12566);
#10020=LINE('',#57473,#12567);
#10021=LINE('',#57477,#12568);
#10022=LINE('',#57480,#12569);
#10023=LINE('',#57484,#12570);
#10024=LINE('',#57487,#12571);
#10025=LINE('',#57492,#12572);
#10026=LINE('',#57587,#12573);
#10027=LINE('',#57590,#12574);
#10028=LINE('',#57594,#12575);
#10029=LINE('',#57611,#12576);
#10030=LINE('',#57616,#12577);
#10031=LINE('',#57618,#12578);
#10032=LINE('',#57620,#12579);
#10033=LINE('',#57950,#12580);
#10034=LINE('',#57951,#12581);
#10035=LINE('',#57952,#12582);
#10036=LINE('',#57955,#12583);
#10037=LINE('',#57956,#12584);
#10038=LINE('',#57960,#12585);
#10039=LINE('',#57962,#12586);
#10040=LINE('',#57965,#12587);
#10041=LINE('',#57968,#12588);
#10042=LINE('',#57972,#12589);
#10043=LINE('',#57975,#12590);
#10044=LINE('',#57979,#12591);
#10045=LINE('',#57982,#12592);
#10046=LINE('',#57986,#12593);
#10047=LINE('',#57989,#12594);
#10048=LINE('',#57993,#12595);
#10049=LINE('',#57996,#12596);
#10050=LINE('',#58000,#12597);
#10051=LINE('',#58003,#12598);
#10052=LINE('',#58007,#12599);
#10053=LINE('',#58010,#12600);
#10054=LINE('',#58014,#12601);
#10055=LINE('',#58017,#12602);
#10056=LINE('',#58021,#12603);
#10057=LINE('',#58024,#12604);
#10058=LINE('',#58028,#12605);
#10059=LINE('',#58031,#12606);
#10060=LINE('',#58035,#12607);
#10061=LINE('',#58038,#12608);
#10062=LINE('',#58042,#12609);
#10063=LINE('',#58045,#12610);
#10064=LINE('',#58049,#12611);
#10065=LINE('',#58052,#12612);
#10066=LINE('',#58056,#12613);
#10067=LINE('',#58059,#12614);
#10068=LINE('',#58063,#12615);
#10069=LINE('',#58066,#12616);
#10070=LINE('',#58070,#12617);
#10071=LINE('',#58073,#12618);
#10072=LINE('',#58077,#12619);
#10073=LINE('',#58080,#12620);
#10074=LINE('',#58084,#12621);
#10075=LINE('',#58087,#12622);
#10076=LINE('',#58091,#12623);
#10077=LINE('',#58094,#12624);
#10078=LINE('',#58098,#12625);
#10079=LINE('',#58101,#12626);
#10080=LINE('',#58105,#12627);
#10081=LINE('',#58108,#12628);
#10082=LINE('',#58112,#12629);
#10083=LINE('',#58115,#12630);
#10084=LINE('',#58119,#12631);
#10085=LINE('',#58122,#12632);
#10086=LINE('',#58126,#12633);
#10087=LINE('',#58129,#12634);
#10088=LINE('',#58133,#12635);
#10089=LINE('',#58136,#12636);
#10090=LINE('',#58140,#12637);
#10091=LINE('',#58143,#12638);
#10092=LINE('',#58147,#12639);
#10093=LINE('',#58150,#12640);
#10094=LINE('',#58154,#12641);
#10095=LINE('',#58157,#12642);
#10096=LINE('',#58161,#12643);
#10097=LINE('',#58164,#12644);
#10098=LINE('',#58168,#12645);
#10099=LINE('',#58171,#12646);
#10100=LINE('',#58175,#12647);
#10101=LINE('',#58178,#12648);
#10102=LINE('',#58182,#12649);
#10103=LINE('',#58185,#12650);
#10104=LINE('',#58189,#12651);
#10105=LINE('',#58192,#12652);
#10106=LINE('',#58196,#12653);
#10107=LINE('',#58199,#12654);
#10108=LINE('',#58203,#12655);
#10109=LINE('',#58206,#12656);
#10110=LINE('',#58210,#12657);
#10111=LINE('',#58213,#12658);
#10112=LINE('',#58217,#12659);
#10113=LINE('',#58220,#12660);
#10114=LINE('',#58224,#12661);
#10115=LINE('',#58227,#12662);
#10116=LINE('',#58231,#12663);
#10117=LINE('',#58234,#12664);
#10118=LINE('',#58238,#12665);
#10119=LINE('',#58241,#12666);
#10120=LINE('',#58245,#12667);
#10121=LINE('',#58248,#12668);
#10122=LINE('',#58252,#12669);
#10123=LINE('',#58255,#12670);
#10124=LINE('',#58259,#12671);
#10125=LINE('',#58262,#12672);
#10126=LINE('',#58266,#12673);
#10127=LINE('',#58269,#12674);
#10128=LINE('',#58273,#12675);
#10129=LINE('',#58276,#12676);
#10130=LINE('',#58280,#12677);
#10131=LINE('',#58283,#12678);
#10132=LINE('',#58287,#12679);
#10133=LINE('',#58290,#12680);
#10134=LINE('',#58294,#12681);
#10135=LINE('',#58297,#12682);
#10136=LINE('',#58301,#12683);
#10137=LINE('',#58304,#12684);
#10138=LINE('',#58308,#12685);
#10139=LINE('',#58311,#12686);
#10140=LINE('',#58315,#12687);
#10141=LINE('',#58318,#12688);
#10142=LINE('',#58322,#12689);
#10143=LINE('',#58325,#12690);
#10144=LINE('',#58329,#12691);
#10145=LINE('',#58332,#12692);
#10146=LINE('',#58336,#12693);
#10147=LINE('',#58339,#12694);
#10148=LINE('',#58343,#12695);
#10149=LINE('',#58346,#12696);
#10150=LINE('',#58350,#12697);
#10151=LINE('',#58353,#12698);
#10152=LINE('',#58357,#12699);
#10153=LINE('',#58360,#12700);
#10154=LINE('',#58364,#12701);
#10155=LINE('',#58367,#12702);
#10156=LINE('',#58371,#12703);
#10157=LINE('',#58374,#12704);
#10158=LINE('',#58378,#12705);
#10159=LINE('',#58381,#12706);
#10160=LINE('',#58385,#12707);
#10161=LINE('',#58388,#12708);
#10162=LINE('',#58392,#12709);
#10163=LINE('',#58395,#12710);
#10164=LINE('',#58399,#12711);
#10165=LINE('',#58402,#12712);
#10166=LINE('',#58406,#12713);
#10167=LINE('',#58409,#12714);
#10168=LINE('',#58413,#12715);
#10169=LINE('',#58416,#12716);
#10170=LINE('',#58420,#12717);
#10171=LINE('',#58423,#12718);
#10172=LINE('',#58427,#12719);
#10173=LINE('',#58430,#12720);
#10174=LINE('',#58434,#12721);
#10175=LINE('',#58437,#12722);
#10176=LINE('',#58441,#12723);
#10177=LINE('',#58444,#12724);
#10178=LINE('',#58448,#12725);
#10179=LINE('',#58451,#12726);
#10180=LINE('',#58455,#12727);
#10181=LINE('',#58458,#12728);
#10182=LINE('',#58462,#12729);
#10183=LINE('',#58465,#12730);
#10184=LINE('',#58469,#12731);
#10185=LINE('',#58472,#12732);
#10186=LINE('',#58476,#12733);
#10187=LINE('',#58479,#12734);
#10188=LINE('',#58483,#12735);
#10189=LINE('',#58486,#12736);
#10190=LINE('',#58490,#12737);
#10191=LINE('',#58493,#12738);
#10192=LINE('',#58497,#12739);
#10193=LINE('',#58500,#12740);
#10194=LINE('',#58504,#12741);
#10195=LINE('',#58507,#12742);
#10196=LINE('',#58512,#12743);
#10197=LINE('',#58591,#12744);
#10198=LINE('',#58594,#12745);
#10199=LINE('',#58598,#12746);
#10200=LINE('',#58614,#12747);
#10201=LINE('',#58620,#12748);
#10202=LINE('',#58625,#12749);
#10203=LINE('',#58630,#12750);
#10204=LINE('',#58639,#12751);
#10205=LINE('',#58646,#12752);
#10206=LINE('',#58652,#12753);
#10207=LINE('',#58657,#12754);
#10208=LINE('',#58662,#12755);
#10209=LINE('',#58671,#12756);
#10210=LINE('',#58677,#12757);
#10211=LINE('',#58686,#12758);
#10212=LINE('',#58689,#12759);
#10213=LINE('',#58694,#12760);
#10214=LINE('',#58702,#12761);
#10215=LINE('',#58708,#12762);
#10216=LINE('',#58715,#12763);
#10217=LINE('',#58724,#12764);
#10218=LINE('',#58732,#12765);
#10219=LINE('',#58735,#12766);
#10220=LINE('',#58740,#12767);
#10221=LINE('',#58747,#12768);
#10222=LINE('',#58756,#12769);
#10223=LINE('',#58764,#12770);
#10224=LINE('',#58767,#12771);
#10225=LINE('',#58771,#12772);
#10226=LINE('',#58773,#12773);
#10227=LINE('',#58775,#12774);
#10228=LINE('',#58777,#12775);
#10229=LINE('',#58783,#12776);
#10230=LINE('',#58785,#12777);
#10231=LINE('',#58787,#12778);
#10232=LINE('',#58789,#12779);
#10233=LINE('',#58791,#12780);
#10234=LINE('',#58793,#12781);
#10235=LINE('',#58795,#12782);
#10236=LINE('',#58797,#12783);
#10237=LINE('',#58799,#12784);
#10238=LINE('',#58804,#12785);
#10239=LINE('',#58810,#12786);
#10240=LINE('',#58813,#12787);
#10241=LINE('',#58816,#12788);
#10242=LINE('',#58818,#12789);
#10243=LINE('',#58819,#12790);
#10244=LINE('',#58825,#12791);
#10245=LINE('',#58828,#12792);
#10246=LINE('',#58831,#12793);
#10247=LINE('',#58833,#12794);
#10248=LINE('',#58835,#12795);
#10249=LINE('',#58837,#12796);
#10250=LINE('',#58838,#12797);
#10251=LINE('',#58841,#12798);
#10252=LINE('',#58842,#12799);
#10253=LINE('',#58844,#12800);
#10254=LINE('',#58845,#12801);
#10255=LINE('',#58848,#12802);
#10256=LINE('',#58850,#12803);
#10257=LINE('',#58851,#12804);
#10258=LINE('',#58855,#12805);
#10259=LINE('',#58859,#12806);
#10260=LINE('',#58861,#12807);
#10261=LINE('',#58863,#12808);
#10262=LINE('',#58864,#12809);
#10263=LINE('',#58867,#12810);
#10264=LINE('',#58868,#12811);
#10265=LINE('',#58873,#12812);
#10266=LINE('',#58875,#12813);
#10267=LINE('',#58877,#12814);
#10268=LINE('',#58882,#12815);
#10269=LINE('',#58884,#12816);
#10270=LINE('',#58886,#12817);
#10271=LINE('',#58894,#12818);
#10272=LINE('',#58900,#12819);
#10273=LINE('',#58903,#12820);
#10274=LINE('',#58905,#12821);
#10275=LINE('',#58907,#12822);
#10276=LINE('',#58909,#12823);
#10277=LINE('',#58911,#12824);
#10278=LINE('',#58912,#12825);
#10279=LINE('',#58921,#12826);
#10280=LINE('',#58927,#12827);
#10281=LINE('',#58931,#12828);
#10282=LINE('',#58933,#12829);
#10283=LINE('',#58937,#12830);
#10284=LINE('',#58941,#12831);
#10285=LINE('',#58943,#12832);
#10286=LINE('',#58945,#12833);
#10287=LINE('',#58947,#12834);
#10288=LINE('',#58948,#12835);
#10289=LINE('',#58951,#12836);
#10290=LINE('',#58957,#12837);
#10291=LINE('',#58958,#12838);
#10292=LINE('',#58961,#12839);
#10293=LINE('',#58962,#12840);
#10294=LINE('',#58965,#12841);
#10295=LINE('',#58971,#12842);
#10296=LINE('',#58973,#12843);
#10297=LINE('',#58975,#12844);
#10298=LINE('',#58976,#12845);
#10299=LINE('',#58981,#12846);
#10300=LINE('',#58985,#12847);
#10301=LINE('',#58987,#12848);
#10302=LINE('',#58992,#12849);
#10303=LINE('',#58994,#12850);
#10304=LINE('',#58996,#12851);
#10305=LINE('',#58998,#12852);
#10306=LINE('',#59000,#12853);
#10307=LINE('',#59002,#12854);
#10308=LINE('',#59003,#12855);
#10309=LINE('',#59012,#12856);
#10310=LINE('',#59019,#12857);
#10311=LINE('',#59024,#12858);
#10312=LINE('',#59030,#12859);
#10313=LINE('',#59035,#12860);
#10314=LINE('',#59040,#12861);
#10315=LINE('',#59043,#12862);
#10316=LINE('',#59044,#12863);
#10317=LINE('',#59046,#12864);
#10318=LINE('',#59050,#12865);
#10319=LINE('',#59052,#12866);
#10320=LINE('',#59054,#12867);
#10321=LINE('',#59055,#12868);
#10322=LINE('',#59058,#12869);
#10323=LINE('',#59060,#12870);
#10324=LINE('',#59061,#12871);
#10325=LINE('',#59064,#12872);
#10326=LINE('',#59066,#12873);
#10327=LINE('',#59067,#12874);
#10328=LINE('',#59069,#12875);
#10329=LINE('',#59081,#12876);
#10330=LINE('',#59090,#12877);
#10331=LINE('',#59098,#12878);
#10332=LINE('',#59106,#12879);
#10333=LINE('',#59114,#12880);
#10334=LINE('',#59119,#12881);
#10335=LINE('',#59121,#12882);
#10336=LINE('',#59123,#12883);
#10337=LINE('',#59124,#12884);
#10338=LINE('',#59125,#12885);
#10339=LINE('',#59127,#12886);
#10340=LINE('',#59129,#12887);
#10341=LINE('',#59131,#12888);
#10342=LINE('',#59132,#12889);
#10343=LINE('',#59134,#12890);
#10344=LINE('',#59139,#12891);
#10345=LINE('',#59141,#12892);
#10346=LINE('',#59142,#12893);
#10347=LINE('',#59146,#12894);
#10348=LINE('',#59148,#12895);
#10349=LINE('',#59151,#12896);
#10350=LINE('',#59156,#12897);
#10351=LINE('',#59166,#12898);
#10352=LINE('',#59172,#12899);
#10353=LINE('',#59174,#12900);
#10354=LINE('',#59175,#12901);
#10355=LINE('',#59183,#12902);
#10356=LINE('',#59188,#12903);
#10357=LINE('',#59189,#12904);
#10358=LINE('',#59197,#12905);
#10359=LINE('',#59202,#12906);
#10360=LINE('',#59203,#12907);
#10361=LINE('',#59211,#12908);
#10362=LINE('',#59216,#12909);
#10363=LINE('',#59217,#12910);
#10364=LINE('',#59246,#12911);
#10365=LINE('',#59248,#12912);
#10366=LINE('',#59249,#12913);
#10367=LINE('',#59251,#12914);
#10368=LINE('',#59252,#12915);
#10369=LINE('',#59263,#12916);
#10370=LINE('',#59269,#12917);
#10371=LINE('',#59271,#12918);
#10372=LINE('',#59272,#12919);
#10373=LINE('',#59280,#12920);
#10374=LINE('',#59285,#12921);
#10375=LINE('',#59286,#12922);
#10376=LINE('',#59294,#12923);
#10377=LINE('',#59299,#12924);
#10378=LINE('',#59300,#12925);
#10379=LINE('',#59308,#12926);
#10380=LINE('',#59313,#12927);
#10381=LINE('',#59314,#12928);
#10382=LINE('',#59343,#12929);
#10383=LINE('',#59345,#12930);
#10384=LINE('',#59346,#12931);
#10385=LINE('',#59348,#12932);
#10386=LINE('',#59349,#12933);
#10387=LINE('',#59355,#12934);
#10388=LINE('',#59356,#12935);
#10389=LINE('',#59359,#12936);
#10390=LINE('',#59361,#12937);
#10391=LINE('',#59362,#12938);
#10392=LINE('',#59365,#12939);
#10393=LINE('',#59366,#12940);
#10394=LINE('',#59369,#12941);
#10395=LINE('',#59370,#12942);
#10396=LINE('',#59373,#12943);
#10397=LINE('',#59374,#12944);
#10398=LINE('',#59377,#12945);
#10399=LINE('',#59378,#12946);
#10400=LINE('',#59380,#12947);
#10401=LINE('',#59383,#12948);
#10402=LINE('',#59385,#12949);
#10403=LINE('',#59395,#12950);
#10404=LINE('',#59397,#12951);
#10405=LINE('',#59399,#12952);
#10406=LINE('',#59401,#12953);
#10407=LINE('',#59403,#12954);
#10408=LINE('',#59404,#12955);
#10409=LINE('',#59408,#12956);
#10410=LINE('',#59409,#12957);
#10411=LINE('',#59410,#12958);
#10412=LINE('',#59413,#12959);
#10413=LINE('',#59414,#12960);
#10414=LINE('',#59417,#12961);
#10415=LINE('',#59418,#12962);
#10416=LINE('',#59421,#12963);
#10417=LINE('',#59422,#12964);
#10418=LINE('',#59425,#12965);
#10419=LINE('',#59426,#12966);
#10420=LINE('',#59428,#12967);
#10421=LINE('',#59435,#12968);
#10422=LINE('',#59437,#12969);
#10423=LINE('',#59439,#12970);
#10424=LINE('',#59441,#12971);
#10425=LINE('',#59443,#12972);
#10426=LINE('',#59444,#12973);
#10427=LINE('',#59448,#12974);
#10428=LINE('',#59449,#12975);
#10429=LINE('',#59450,#12976);
#10430=LINE('',#59453,#12977);
#10431=LINE('',#59454,#12978);
#10432=LINE('',#59457,#12979);
#10433=LINE('',#59458,#12980);
#10434=LINE('',#59461,#12981);
#10435=LINE('',#59462,#12982);
#10436=LINE('',#59465,#12983);
#10437=LINE('',#59466,#12984);
#10438=LINE('',#59468,#12985);
#10439=LINE('',#59474,#12986);
#10440=LINE('',#59475,#12987);
#10441=LINE('',#59478,#12988);
#10442=LINE('',#59479,#12989);
#10443=LINE('',#59481,#12990);
#10444=LINE('',#59486,#12991);
#10445=LINE('',#59490,#12992);
#10446=LINE('',#59496,#12993);
#10447=LINE('',#59502,#12994);
#10448=LINE('',#59507,#12995);
#10449=LINE('',#59513,#12996);
#10450=LINE('',#59519,#12997);
#10451=LINE('',#59524,#12998);
#10452=LINE('',#59530,#12999);
#10453=LINE('',#59536,#13000);
#10454=LINE('',#59544,#13001);
#10455=LINE('',#59548,#13002);
#10456=LINE('',#59554,#13003);
#10457=LINE('',#59561,#13004);
#10458=LINE('',#59565,#13005);
#10459=LINE('',#59571,#13006);
#10460=LINE('',#59578,#13007);
#10461=LINE('',#59582,#13008);
#10462=LINE('',#59588,#13009);
#10463=LINE('',#59595,#13010);
#10464=LINE('',#59599,#13011);
#10465=LINE('',#59605,#13012);
#10466=LINE('',#59608,#13013);
#10467=LINE('',#59611,#13014);
#10468=LINE('',#59614,#13015);
#10469=LINE('',#59617,#13016);
#10470=LINE('',#59620,#13017);
#10471=LINE('',#59623,#13018);
#10472=LINE('',#59626,#13019);
#10473=LINE('',#59629,#13020);
#10474=LINE('',#59632,#13021);
#10475=LINE('',#59634,#13022);
#10476=LINE('',#59635,#13023);
#10477=LINE('',#59638,#13024);
#10478=LINE('',#59639,#13025);
#10479=LINE('',#59642,#13026);
#10480=LINE('',#59644,#13027);
#10481=LINE('',#59645,#13028);
#10482=LINE('',#59648,#13029);
#10483=LINE('',#59649,#13030);
#10484=LINE('',#59652,#13031);
#10485=LINE('',#59653,#13032);
#10486=LINE('',#59656,#13033);
#10487=LINE('',#59657,#13034);
#10488=LINE('',#59660,#13035);
#10489=LINE('',#59661,#13036);
#10490=LINE('',#59663,#13037);
#10491=LINE('',#59666,#13038);
#10492=LINE('',#59667,#13039);
#10493=LINE('',#59670,#13040);
#10494=LINE('',#59672,#13041);
#10495=LINE('',#59674,#13042);
#10496=LINE('',#59676,#13043);
#10497=LINE('',#59678,#13044);
#10498=LINE('',#59680,#13045);
#10499=LINE('',#59682,#13046);
#10500=LINE('',#59683,#13047);
#10501=LINE('',#59691,#13048);
#10502=LINE('',#59698,#13049);
#10503=LINE('',#59703,#13050);
#10504=LINE('',#59706,#13051);
#10505=LINE('',#59707,#13052);
#10506=LINE('',#59710,#13053);
#10507=LINE('',#59711,#13054);
#10508=LINE('',#59714,#13055);
#10509=LINE('',#59715,#13056);
#10510=LINE('',#59718,#13057);
#10511=LINE('',#59719,#13058);
#10512=LINE('',#59722,#13059);
#10513=LINE('',#59723,#13060);
#10514=LINE('',#59725,#13061);
#10515=LINE('',#59728,#13062);
#10516=LINE('',#59737,#13063);
#10517=LINE('',#59741,#13064);
#10518=LINE('',#59821,#13065);
#10519=LINE('',#59824,#13066);
#10520=LINE('',#59825,#13067);
#10521=LINE('',#59832,#13068);
#10522=LINE('',#59840,#13069);
#10523=LINE('',#59845,#13070);
#10524=LINE('',#59847,#13071);
#10525=LINE('',#59849,#13072);
#10526=LINE('',#59851,#13073);
#10527=LINE('',#59853,#13074);
#10528=LINE('',#59854,#13075);
#10529=LINE('',#59857,#13076);
#10530=LINE('',#59859,#13077);
#10531=LINE('',#59861,#13078);
#10532=LINE('',#59863,#13079);
#10533=LINE('',#59865,#13080);
#10534=LINE('',#59866,#13081);
#10535=LINE('',#59873,#13082);
#10536=LINE('',#59881,#13083);
#10537=LINE('',#59889,#13084);
#10538=LINE('',#59894,#13085);
#10539=LINE('',#59896,#13086);
#10540=LINE('',#59899,#13087);
#10541=LINE('',#59917,#13088);
#10542=LINE('',#59920,#13089);
#10543=LINE('',#59997,#13090);
#10544=LINE('',#60000,#13091);
#10545=LINE('',#60001,#13092);
#10546=LINE('',#60005,#13093);
#10547=LINE('',#60007,#13094);
#10548=LINE('',#60009,#13095);
#10549=LINE('',#60011,#13096);
#10550=LINE('',#60013,#13097);
#10551=LINE('',#60014,#13098);
#10552=LINE('',#60018,#13099);
#10553=LINE('',#60019,#13100);
#10554=LINE('',#60020,#13101);
#10555=LINE('',#60023,#13102);
#10556=LINE('',#60024,#13103);
#10557=LINE('',#60027,#13104);
#10558=LINE('',#60028,#13105);
#10559=LINE('',#60031,#13106);
#10560=LINE('',#60032,#13107);
#10561=LINE('',#60035,#13108);
#10562=LINE('',#60036,#13109);
#10563=LINE('',#60038,#13110);
#10564=LINE('',#60042,#13111);
#10565=LINE('',#60044,#13112);
#10566=LINE('',#60046,#13113);
#10567=LINE('',#60048,#13114);
#10568=LINE('',#60050,#13115);
#10569=LINE('',#60051,#13116);
#10570=LINE('',#60055,#13117);
#10571=LINE('',#60056,#13118);
#10572=LINE('',#60057,#13119);
#10573=LINE('',#60060,#13120);
#10574=LINE('',#60061,#13121);
#10575=LINE('',#60064,#13122);
#10576=LINE('',#60065,#13123);
#10577=LINE('',#60068,#13124);
#10578=LINE('',#60069,#13125);
#10579=LINE('',#60072,#13126);
#10580=LINE('',#60073,#13127);
#10581=LINE('',#60075,#13128);
#10582=LINE('',#60084,#13129);
#10583=LINE('',#60121,#13130);
#10584=LINE('',#60128,#13131);
#10585=LINE('',#60139,#13132);
#10586=LINE('',#60143,#13133);
#10587=LINE('',#60145,#13134);
#10588=LINE('',#60147,#13135);
#10589=LINE('',#60149,#13136);
#10590=LINE('',#60151,#13137);
#10591=LINE('',#60152,#13138);
#10592=LINE('',#60156,#13139);
#10593=LINE('',#60157,#13140);
#10594=LINE('',#60158,#13141);
#10595=LINE('',#60161,#13142);
#10596=LINE('',#60162,#13143);
#10597=LINE('',#60165,#13144);
#10598=LINE('',#60166,#13145);
#10599=LINE('',#60169,#13146);
#10600=LINE('',#60170,#13147);
#10601=LINE('',#60173,#13148);
#10602=LINE('',#60174,#13149);
#10603=LINE('',#60176,#13150);
#10604=LINE('',#60180,#13151);
#10605=LINE('',#60182,#13152);
#10606=LINE('',#60184,#13153);
#10607=LINE('',#60186,#13154);
#10608=LINE('',#60188,#13155);
#10609=LINE('',#60189,#13156);
#10610=LINE('',#60193,#13157);
#10611=LINE('',#60194,#13158);
#10612=LINE('',#60195,#13159);
#10613=LINE('',#60198,#13160);
#10614=LINE('',#60199,#13161);
#10615=LINE('',#60202,#13162);
#10616=LINE('',#60203,#13163);
#10617=LINE('',#60206,#13164);
#10618=LINE('',#60207,#13165);
#10619=LINE('',#60210,#13166);
#10620=LINE('',#60211,#13167);
#10621=LINE('',#60213,#13168);
#10622=LINE('',#60222,#13169);
#10623=LINE('',#60259,#13170);
#10624=LINE('',#60266,#13171);
#10625=LINE('',#60277,#13172);
#10626=LINE('',#60314,#13173);
#10627=LINE('',#60317,#13174);
#10628=LINE('',#60321,#13175);
#10629=LINE('',#60323,#13176);
#10630=LINE('',#60328,#13177);
#10631=LINE('',#60365,#13178);
#10632=LINE('',#60372,#13179);
#10633=LINE('',#60375,#13180);
#10634=LINE('',#60390,#13181);
#10635=LINE('',#60398,#13182);
#10636=LINE('',#60401,#13183);
#10637=LINE('',#60408,#13184);
#10638=LINE('',#60414,#13185);
#10639=LINE('',#60418,#13186);
#10640=LINE('',#60422,#13187);
#10641=LINE('',#60426,#13188);
#10642=LINE('',#60430,#13189);
#10643=LINE('',#60433,#13190);
#10644=LINE('',#60451,#13191);
#10645=LINE('',#60452,#13192);
#10646=LINE('',#60461,#13193);
#10647=LINE('',#60488,#13194);
#10648=LINE('',#60490,#13195);
#10649=LINE('',#60492,#13196);
#10650=LINE('',#60499,#13197);
#10651=LINE('',#60503,#13198);
#10652=LINE('',#60507,#13199);
#10653=LINE('',#60511,#13200);
#10654=LINE('',#60515,#13201);
#10655=LINE('',#60518,#13202);
#10656=LINE('',#60536,#13203);
#10657=LINE('',#60537,#13204);
#10658=LINE('',#60546,#13205);
#10659=LINE('',#60573,#13206);
#10660=LINE('',#60575,#13207);
#10661=LINE('',#60577,#13208);
#10662=LINE('',#60592,#13209);
#10663=LINE('',#60598,#13210);
#10664=LINE('',#60603,#13211);
#10665=LINE('',#60608,#13212);
#10666=LINE('',#60614,#13213);
#10667=LINE('',#60620,#13214);
#10668=LINE('',#60626,#13215);
#10669=LINE('',#60635,#13216);
#10670=LINE('',#60643,#13217);
#10671=LINE('',#60648,#13218);
#10672=LINE('',#60650,#13219);
#10673=LINE('',#60652,#13220);
#10674=LINE('',#60653,#13221);
#10675=LINE('',#60658,#13222);
#10676=LINE('',#60664,#13223);
#10677=LINE('',#60670,#13224);
#10678=LINE('',#60674,#13225);
#10679=LINE('',#60676,#13226);
#10680=LINE('',#60677,#13227);
#10681=LINE('',#60682,#13228);
#10682=LINE('',#60688,#13229);
#10683=LINE('',#60697,#13230);
#10684=LINE('',#60699,#13231);
#10685=LINE('',#60701,#13232);
#10686=LINE('',#60702,#13233);
#10687=LINE('',#60707,#13234);
#10688=LINE('',#60713,#13235);
#10689=LINE('',#60719,#13236);
#10690=LINE('',#60723,#13237);
#10691=LINE('',#60725,#13238);
#10692=LINE('',#60726,#13239);
#10693=LINE('',#60731,#13240);
#10694=LINE('',#60737,#13241);
#10695=LINE('',#60746,#13242);
#10696=LINE('',#60748,#13243);
#10697=LINE('',#60750,#13244);
#10698=LINE('',#60751,#13245);
#10699=LINE('',#60756,#13246);
#10700=LINE('',#60762,#13247);
#10701=LINE('',#60768,#13248);
#10702=LINE('',#60772,#13249);
#10703=LINE('',#60774,#13250);
#10704=LINE('',#60775,#13251);
#10705=LINE('',#60780,#13252);
#10706=LINE('',#60786,#13253);
#10707=LINE('',#60794,#13254);
#10708=LINE('',#60798,#13255);
#10709=LINE('',#60802,#13256);
#10710=LINE('',#60814,#13257);
#10711=LINE('',#60825,#13258);
#10712=LINE('',#60836,#13259);
#10713=LINE('',#60840,#13260);
#10714=LINE('',#60842,#13261);
#10715=LINE('',#60846,#13262);
#10716=LINE('',#60848,#13263);
#10717=LINE('',#60853,#13264);
#10718=LINE('',#60857,#13265);
#10719=LINE('',#60859,#13266);
#10720=LINE('',#60862,#13267);
#10721=LINE('',#60866,#13268);
#10722=LINE('',#60870,#13269);
#10723=LINE('',#60872,#13270);
#10724=LINE('',#60875,#13271);
#10725=LINE('',#60882,#13272);
#10726=LINE('',#60888,#13273);
#10727=LINE('',#60890,#13274);
#10728=LINE('',#60891,#13275);
#10729=LINE('',#60894,#13276);
#10730=LINE('',#60896,#13277);
#10731=LINE('',#60897,#13278);
#10732=LINE('',#60900,#13279);
#10733=LINE('',#60902,#13280);
#10734=LINE('',#60903,#13281);
#10735=LINE('',#60906,#13282);
#10736=LINE('',#60908,#13283);
#10737=LINE('',#60909,#13284);
#10738=LINE('',#60912,#13285);
#10739=LINE('',#60914,#13286);
#10740=LINE('',#60915,#13287);
#10741=LINE('',#60917,#13288);
#10742=LINE('',#60919,#13289);
#10743=LINE('',#60920,#13290);
#10744=LINE('',#60921,#13291);
#10745=LINE('',#60924,#13292);
#10746=LINE('',#60928,#13293);
#10747=LINE('',#60929,#13294);
#10748=LINE('',#60931,#13295);
#10749=LINE('',#60933,#13296);
#10750=LINE('',#60934,#13297);
#10751=LINE('',#60935,#13298);
#10752=LINE('',#60938,#13299);
#10753=LINE('',#60942,#13300);
#10754=LINE('',#60943,#13301);
#10755=LINE('',#60945,#13302);
#10756=LINE('',#60947,#13303);
#10757=LINE('',#60949,#13304);
#10758=LINE('',#60951,#13305);
#10759=LINE('',#60952,#13306);
#10760=LINE('',#60957,#13307);
#10761=LINE('',#60962,#13308);
#10762=LINE('',#60966,#13309);
#10763=LINE('',#60969,#13310);
#10764=LINE('',#60971,#13311);
#10765=LINE('',#60973,#13312);
#10766=LINE('',#60975,#13313);
#10767=LINE('',#60976,#13314);
#10768=LINE('',#60977,#13315);
#10769=LINE('',#60982,#13316);
#10770=LINE('',#60984,#13317);
#10771=LINE('',#60987,#13318);
#10772=LINE('',#60989,#13319);
#10773=LINE('',#60992,#13320);
#10774=LINE('',#60994,#13321);
#10775=LINE('',#60997,#13322);
#10776=LINE('',#60999,#13323);
#10777=LINE('',#61003,#13324);
#10778=LINE('',#61004,#13325);
#10779=LINE('',#61008,#13326);
#10780=LINE('',#61010,#13327);
#10781=LINE('',#61012,#13328);
#10782=LINE('',#61014,#13329);
#10783=LINE('',#61017,#13330);
#10784=LINE('',#61019,#13331);
#10785=LINE('',#61022,#13332);
#10786=LINE('',#61024,#13333);
#10787=LINE('',#61036,#13334);
#10788=LINE('',#61039,#13335);
#10789=LINE('',#61042,#13336);
#10790=LINE('',#61044,#13337);
#10791=LINE('',#61045,#13338);
#10792=LINE('',#61050,#13339);
#10793=LINE('',#61056,#13340);
#10794=LINE('',#61062,#13341);
#10795=LINE('',#61066,#13342);
#10796=LINE('',#61068,#13343);
#10797=LINE('',#61069,#13344);
#10798=LINE('',#61074,#13345);
#10799=LINE('',#61083,#13346);
#10800=LINE('',#61085,#13347);
#10801=LINE('',#61087,#13348);
#10802=LINE('',#61088,#13349);
#10803=LINE('',#61093,#13350);
#10804=LINE('',#61099,#13351);
#10805=LINE('',#61105,#13352);
#10806=LINE('',#61109,#13353);
#10807=LINE('',#61111,#13354);
#10808=LINE('',#61112,#13355);
#10809=LINE('',#61117,#13356);
#10810=LINE('',#61123,#13357);
#10811=LINE('',#61134,#13358);
#10812=LINE('',#61137,#13359);
#10813=LINE('',#61142,#13360);
#10814=LINE('',#61146,#13361);
#10815=LINE('',#61148,#13362);
#10816=LINE('',#61149,#13363);
#10817=LINE('',#61154,#13364);
#10818=LINE('',#61160,#13365);
#10819=LINE('',#61166,#13366);
#10820=LINE('',#61170,#13367);
#10821=LINE('',#61172,#13368);
#10822=LINE('',#61173,#13369);
#10823=LINE('',#61183,#13370);
#10824=LINE('',#61186,#13371);
#10825=LINE('',#61191,#13372);
#10826=LINE('',#61195,#13373);
#10827=LINE('',#61197,#13374);
#10828=LINE('',#61198,#13375);
#10829=LINE('',#61203,#13376);
#10830=LINE('',#61209,#13377);
#10831=LINE('',#61215,#13378);
#10832=LINE('',#61219,#13379);
#10833=LINE('',#61221,#13380);
#10834=LINE('',#61222,#13381);
#10835=LINE('',#61231,#13382);
#10836=LINE('',#61232,#13383);
#10837=LINE('',#61236,#13384);
#10838=LINE('',#61239,#13385);
#10839=LINE('',#61240,#13386);
#10840=LINE('',#61244,#13387);
#10841=LINE('',#61248,#13388);
#10842=LINE('',#61252,#13389);
#10843=LINE('',#61256,#13390);
#10844=LINE('',#61258,#13391);
#10845=LINE('',#61266,#13392);
#10846=LINE('',#61268,#13393);
#10847=LINE('',#61270,#13394);
#10848=LINE('',#61272,#13395);
#10849=LINE('',#61274,#13396);
#10850=LINE('',#61276,#13397);
#10851=LINE('',#61278,#13398);
#10852=LINE('',#61279,#13399);
#10853=LINE('',#61281,#13400);
#10854=LINE('',#61282,#13401);
#10855=LINE('',#61284,#13402);
#10856=LINE('',#61285,#13403);
#10857=LINE('',#61288,#13404);
#10858=LINE('',#61289,#13405);
#10859=LINE('',#61291,#13406);
#10860=LINE('',#61294,#13407);
#10861=LINE('',#61304,#13408);
#10862=LINE('',#61308,#13409);
#10863=LINE('',#61313,#13410);
#10864=LINE('',#61317,#13411);
#10865=LINE('',#61319,#13412);
#10866=LINE('',#61321,#13413);
#10867=LINE('',#61322,#13414);
#10868=LINE('',#61325,#13415);
#10869=LINE('',#61327,#13416);
#10870=LINE('',#61328,#13417);
#10871=LINE('',#61331,#13418);
#10872=LINE('',#61333,#13419);
#10873=LINE('',#61334,#13420);
#10874=LINE('',#61337,#13421);
#10875=LINE('',#61339,#13422);
#10876=LINE('',#61340,#13423);
#10877=LINE('',#61343,#13424);
#10878=LINE('',#61345,#13425);
#10879=LINE('',#61346,#13426);
#10880=LINE('',#61348,#13427);
#10881=LINE('',#61350,#13428);
#10882=LINE('',#61357,#13429);
#10883=LINE('',#61466,#13430);
#10884=LINE('',#61538,#13431);
#10885=LINE('',#61575,#13432);
#10886=LINE('',#61615,#13433);
#10887=LINE('',#61658,#13434);
#10888=LINE('',#61666,#13435);
#10889=LINE('',#61672,#13436);
#10890=LINE('',#61681,#13437);
#10891=LINE('',#61685,#13438);
#10892=LINE('',#61691,#13439);
#10893=VECTOR('',#38180,10.);
#10894=VECTOR('',#38181,10.);
#10895=VECTOR('',#38182,10.);
#10896=VECTOR('',#38183,10.);
#10897=VECTOR('',#38186,10.);
#10898=VECTOR('',#38187,10.);
#10899=VECTOR('',#38188,10.);
#10900=VECTOR('',#38189,10.);
#10901=VECTOR('',#38192,9.99999999999999);
#10902=VECTOR('',#38193,9.99999999999999);
#10903=VECTOR('',#38196,10.);
#10904=VECTOR('',#38197,9.99999999999999);
#10905=VECTOR('',#38200,10.);
#10906=VECTOR('',#38203,10.);
#10907=VECTOR('',#38204,10.);
#10908=VECTOR('',#38207,10.);
#10909=VECTOR('',#38210,10.);
#10910=VECTOR('',#38211,10.);
#10911=VECTOR('',#38214,10.);
#10912=VECTOR('',#38225,10.);
#10913=VECTOR('',#38226,10.);
#10914=VECTOR('',#38227,10.);
#10915=VECTOR('',#38230,10.);
#10916=VECTOR('',#38235,10.);
#10917=VECTOR('',#38236,9.99999999999999);
#10918=VECTOR('',#38239,10.);
#10919=VECTOR('',#38240,10.);
#10920=VECTOR('',#38243,10.);
#10921=VECTOR('',#38244,10.);
#10922=VECTOR('',#38245,10.);
#10923=VECTOR('',#38248,10.);
#10924=VECTOR('',#38253,10.);
#10925=VECTOR('',#38254,10.);
#10926=VECTOR('',#38257,10.);
#10927=VECTOR('',#38258,10.);
#10928=VECTOR('',#38263,10.);
#10929=VECTOR('',#38270,10.);
#10930=VECTOR('',#38273,10.);
#10931=VECTOR('',#38276,10.);
#10932=VECTOR('',#38277,10.);
#10933=VECTOR('',#38280,10.);
#10934=VECTOR('',#38283,10.);
#10935=VECTOR('',#38284,10.);
#10936=VECTOR('',#38297,85.);
#10937=VECTOR('',#38300,85.);
#10938=VECTOR('',#38303,85.);
#10939=VECTOR('',#38306,85.);
#10940=VECTOR('',#38317,60.);
#10941=VECTOR('',#38320,60.);
#10942=VECTOR('',#38323,60.);
#10943=VECTOR('',#38326,60.);
#10944=VECTOR('',#38331,13.46);
#10945=VECTOR('',#38332,13.46);
#10946=VECTOR('',#38343,6.406394945352);
#10947=VECTOR('',#38346,6.40650331130805);
#10948=VECTOR('',#38351,13.1015672783503);
#10949=VECTOR('',#38352,6.406394945352);
#10950=VECTOR('',#38355,6.406394945352);
#10951=VECTOR('',#38356,13.1015672783303);
#10952=VECTOR('',#38363,13.1015672783301);
#10953=VECTOR('',#38364,6.406394945352);
#10954=VECTOR('',#38367,6.406394945352);
#10955=VECTOR('',#38368,13.1015672783004);
#10956=VECTOR('',#38375,13.1015672783503);
#10957=VECTOR('',#38376,6.406394945352);
#10958=VECTOR('',#38377,13.1015672783303);
#10959=VECTOR('',#38384,13.1015672783301);
#10960=VECTOR('',#38385,6.406394945352);
#10961=VECTOR('',#38388,6.406394945352);
#10962=VECTOR('',#38389,13.1015672783004);
#10963=VECTOR('',#38394,5.75);
#10964=VECTOR('',#38397,5.75);
#10965=VECTOR('',#38400,5.75);
#10966=VECTOR('',#38403,5.75);
#10967=VECTOR('',#38418,47.25);
#10968=VECTOR('',#38447,10.1277288760101);
#10969=VECTOR('',#38448,60.8968295013);
#10970=VECTOR('',#38449,10.1277306467203);
#10971=VECTOR('',#38454,10.1275050058501);
#10972=VECTOR('',#38455,60.8968295013);
#10973=VECTOR('',#38456,10.1275545073903);
#10974=VECTOR('',#38461,10.1277288760101);
#10975=VECTOR('',#38462,60.8968295013);
#10976=VECTOR('',#38463,10.1277306467203);
#10977=VECTOR('',#38468,10.1275522165901);
#10978=VECTOR('',#38469,60.8968295013);
#10979=VECTOR('',#38470,10.1274976633303);
#10980=VECTOR('',#38475,13.6647791615402);
#10981=VECTOR('',#38490,6.40650331130805);
#10982=VECTOR('',#38501,13.46);
#10983=VECTOR('',#38502,13.46);
#10984=VECTOR('',#38505,6.40650331130805);
#10985=VECTOR('',#38506,60.89682950219);
#10986=VECTOR('',#38507,6.40650330990706);
#10987=VECTOR('',#38508,13.46);
#10988=VECTOR('',#38523,13.46);
#10989=VECTOR('',#38526,6.40650330990706);
#10990=VECTOR('',#38527,60.89682950219);
#10991=VECTOR('',#38534,13.6647800109101);
#10992=VECTOR('',#38561,13.6647772519894);
#10993=VECTOR('',#38578,13.6647772688202);
#10994=VECTOR('',#38617,13.6647800109101);
#10995=VECTOR('',#38628,60.89682950219);
#10996=VECTOR('',#38633,6.40650330990706);
#10997=VECTOR('',#38634,13.46);
#10998=VECTOR('',#38639,13.46);
#10999=VECTOR('',#38650,6.40650331130805);
#11000=VECTOR('',#38653,60.89682950219);
#11001=VECTOR('',#38654,6.40650330906005);
#11002=VECTOR('',#38667,13.6647772688694);
#11003=VECTOR('',#38680,13.6647791615402);
#11004=VECTOR('',#38717,13.6647772519099);
#11005=VECTOR('',#38764,35.75);
#11006=VECTOR('',#38773,27.315);
#11007=VECTOR('',#38782,23.435);
#11008=VECTOR('',#38791,15.);
#11009=VECTOR('',#38800,23.435);
#11010=VECTOR('',#38809,27.315);
#11011=VECTOR('',#38818,35.75);
#11012=VECTOR('',#38823,60.);
#11013=VECTOR('',#38826,60.);
#11014=VECTOR('',#38829,60.);
#11015=VECTOR('',#38832,60.);
#11016=VECTOR('',#38835,3.81);
#11017=VECTOR('',#38836,3.81);
#11018=VECTOR('',#38839,3.81);
#11019=VECTOR('',#38842,3.81);
#11020=VECTOR('',#38845,3.81);
#11021=VECTOR('',#38848,3.81);
#11022=VECTOR('',#38851,3.81);
#11023=VECTOR('',#38854,3.81);
#11024=VECTOR('',#38875,6.);
#11025=VECTOR('',#38882,5.46323125);
#11026=VECTOR('',#38899,10.);
#11027=VECTOR('',#38900,10.);
#11028=VECTOR('',#38901,10.);
#11029=VECTOR('',#38902,10.);
#11030=VECTOR('',#38903,10.);
#11031=VECTOR('',#38904,10.);
#11032=VECTOR('',#38907,9.);
#11033=VECTOR('',#38910,10.);
#11034=VECTOR('',#38911,10.);
#11035=VECTOR('',#38914,10.);
#11036=VECTOR('',#38917,10.);
#11037=VECTOR('',#38920,10.);
#11038=VECTOR('',#38923,10.);
#11039=VECTOR('',#38928,2.88675134594813);
#11040=VECTOR('',#38947,5.);
#11041=VECTOR('',#38954,4.5399125);
#11042=VECTOR('',#38971,10.);
#11043=VECTOR('',#38972,10.);
#11044=VECTOR('',#38973,10.);
#11045=VECTOR('',#38974,10.);
#11046=VECTOR('',#38975,9.99999999999999);
#11047=VECTOR('',#38976,10.);
#11048=VECTOR('',#38979,8.);
#11049=VECTOR('',#38982,10.);
#11050=VECTOR('',#38983,10.);
#11051=VECTOR('',#38986,10.);
#11052=VECTOR('',#38989,10.);
#11053=VECTOR('',#38992,10.);
#11054=VECTOR('',#38995,10.);
#11055=VECTOR('',#39000,2.3094010767585);
#11056=VECTOR('',#39019,5.);
#11057=VECTOR('',#39026,4.5399125);
#11058=VECTOR('',#39043,10.);
#11059=VECTOR('',#39044,10.);
#11060=VECTOR('',#39045,10.);
#11061=VECTOR('',#39046,10.);
#11062=VECTOR('',#39047,10.);
#11063=VECTOR('',#39048,10.);
#11064=VECTOR('',#39051,8.);
#11065=VECTOR('',#39054,10.);
#11066=VECTOR('',#39055,10.);
#11067=VECTOR('',#39058,10.);
#11068=VECTOR('',#39061,10.);
#11069=VECTOR('',#39064,10.);
#11070=VECTOR('',#39067,10.);
#11071=VECTOR('',#39072,2.3094010767585);
#11072=VECTOR('',#39091,5.);
#11073=VECTOR('',#39098,4.5399125);
#11074=VECTOR('',#39129,10.);
#11075=VECTOR('',#39130,10.);
#11076=VECTOR('',#39131,10.);
#11077=VECTOR('',#39134,10.);
#11078=VECTOR('',#39135,10.);
#11079=VECTOR('',#39138,10.);
#11080=VECTOR('',#39139,10.);
#11081=VECTOR('',#39142,10.);
#11082=VECTOR('',#39143,10.);
#11083=VECTOR('',#39144,9.99999999999999);
#11084=VECTOR('',#39149,10.);
#11085=VECTOR('',#39152,10.);
#11086=VECTOR('',#39159,7.3);
#11087=VECTOR('',#39164,10.);
#11088=VECTOR('',#39165,10.);
#11089=VECTOR('',#39166,10.);
#11090=VECTOR('',#39167,10.);
#11091=VECTOR('',#39170,10.);
#11092=VECTOR('',#39171,10.);
#11093=VECTOR('',#39172,10.);
#11094=VECTOR('',#39175,10.);
#11095=VECTOR('',#39176,10.);
#11096=VECTOR('',#39177,10.);
#11097=VECTOR('',#39180,10.);
#11098=VECTOR('',#39181,10.);
#11099=VECTOR('',#39184,10.);
#11100=VECTOR('',#39185,10.);
#11101=VECTOR('',#39186,10.);
#11102=VECTOR('',#39187,10.);
#11103=VECTOR('',#39190,10.);
#11104=VECTOR('',#39191,10.);
#11105=VECTOR('',#39192,10.);
#11106=VECTOR('',#39195,10.);
#11107=VECTOR('',#39196,10.);
#11108=VECTOR('',#39197,10.);
#11109=VECTOR('',#39200,10.);
#11110=VECTOR('',#39201,10.);
#11111=VECTOR('',#39206,10.);
#11112=VECTOR('',#39207,10.);
#11113=VECTOR('',#39208,10.);
#11114=VECTOR('',#39209,10.);
#11115=VECTOR('',#39212,10.);
#11116=VECTOR('',#39213,10.);
#11117=VECTOR('',#39214,10.);
#11118=VECTOR('',#39217,10.);
#11119=VECTOR('',#39218,10.);
#11120=VECTOR('',#39219,10.);
#11121=VECTOR('',#39222,10.);
#11122=VECTOR('',#39223,10.);
#11123=VECTOR('',#39234,4.);
#11124=VECTOR('',#39241,4.);
#11125=VECTOR('',#39248,4.);
#11126=VECTOR('',#39255,4.);
#11127=VECTOR('',#39262,4.);
#11128=VECTOR('',#39269,4.);
#11129=VECTOR('',#39274,10.);
#11130=VECTOR('',#39275,10.);
#11131=VECTOR('',#39276,10.);
#11132=VECTOR('',#39277,10.);
#11133=VECTOR('',#39278,10.);
#11134=VECTOR('',#39279,10.);
#11135=VECTOR('',#39280,10.);
#11136=VECTOR('',#39281,10.);
#11137=VECTOR('',#39284,10.);
#11138=VECTOR('',#39285,10.);
#11139=VECTOR('',#39286,10.);
#11140=VECTOR('',#39289,10.);
#11141=VECTOR('',#39290,10.);
#11142=VECTOR('',#39293,10.);
#11143=VECTOR('',#39294,10.);
#11144=VECTOR('',#39297,10.);
#11145=VECTOR('',#39300,10.);
#11146=VECTOR('',#39301,10.);
#11147=VECTOR('',#39302,10.);
#11148=VECTOR('',#39305,10.);
#11149=VECTOR('',#39306,10.);
#11150=VECTOR('',#39307,10.);
#11151=VECTOR('',#39308,10.);
#11152=VECTOR('',#39311,10.);
#11153=VECTOR('',#39312,10.);
#11154=VECTOR('',#39313,10.);
#11155=VECTOR('',#39314,10.);
#11156=VECTOR('',#39317,10.);
#11157=VECTOR('',#39318,10.);
#11158=VECTOR('',#39319,10.);
#11159=VECTOR('',#39322,10.);
#11160=VECTOR('',#39323,10.);
#11161=VECTOR('',#39324,10.);
#11162=VECTOR('',#39325,10.);
#11163=VECTOR('',#39328,10.);
#11164=VECTOR('',#39329,10.);
#11165=VECTOR('',#39330,10.);
#11166=VECTOR('',#39333,10.);
#11167=VECTOR('',#39334,10.);
#11168=VECTOR('',#39335,10.);
#11169=VECTOR('',#39338,10.);
#11170=VECTOR('',#39339,10.);
#11171=VECTOR('',#39340,10.);
#11172=VECTOR('',#39343,10.);
#11173=VECTOR('',#39344,10.);
#11174=VECTOR('',#39347,10.);
#11175=VECTOR('',#39348,10.);
#11176=VECTOR('',#39353,10.);
#11177=VECTOR('',#39354,10.);
#11178=VECTOR('',#39357,10.);
#11179=VECTOR('',#39358,10.);
#11180=VECTOR('',#39361,10.);
#11181=VECTOR('',#39362,10.);
#11182=VECTOR('',#39365,10.);
#11183=VECTOR('',#39376,10.);
#11184=VECTOR('',#39377,10.);
#11185=VECTOR('',#39378,9.99999999999999);
#11186=VECTOR('',#39381,10.);
#11187=VECTOR('',#39382,10.);
#11188=VECTOR('',#39385,10.);
#11189=VECTOR('',#39386,10.);
#11190=VECTOR('',#39391,10.);
#11191=VECTOR('',#39394,4.08939999999975);
#11192=VECTOR('',#39399,10.);
#11193=VECTOR('',#39404,10.);
#11194=VECTOR('',#39407,10.);
#11195=VECTOR('',#39408,10.);
#11196=VECTOR('',#39411,10.);
#11197=VECTOR('',#39412,10.);
#11198=VECTOR('',#39415,10.);
#11199=VECTOR('',#39416,10.);
#11200=VECTOR('',#39419,10.);
#11201=VECTOR('',#39420,10.);
#11202=VECTOR('',#39423,10.);
#11203=VECTOR('',#39424,10.);
#11204=VECTOR('',#39425,10.);
#11205=VECTOR('',#39428,10.);
#11206=VECTOR('',#39429,10.);
#11207=VECTOR('',#39430,10.);
#11208=VECTOR('',#39435,4.08939999999991);
#11209=VECTOR('',#39446,10.);
#11210=VECTOR('',#39449,10.);
#11211=VECTOR('',#39450,10.);
#11212=VECTOR('',#39451,10.);
#11213=VECTOR('',#39484,10.);
#11214=VECTOR('',#39485,10.);
#11215=VECTOR('',#39486,10.);
#11216=VECTOR('',#39491,10.);
#11217=VECTOR('',#39492,10.);
#11218=VECTOR('',#39501,4.08939999999986);
#11219=VECTOR('',#39506,4.08939999999985);
#11220=VECTOR('',#39513,10.);
#11221=VECTOR('',#39514,10.);
#11222=VECTOR('',#39515,10.);
#11223=VECTOR('',#39520,10.);
#11224=VECTOR('',#39521,10.);
#11225=VECTOR('',#39526,10.);
#11226=VECTOR('',#39527,10.);
#11227=VECTOR('',#39532,10.);
#11228=VECTOR('',#39533,10.);
#11229=VECTOR('',#39538,10.);
#11230=VECTOR('',#39539,10.);
#11231=VECTOR('',#39544,10.);
#11232=VECTOR('',#39545,10.);
#11233=VECTOR('',#39550,10.);
#11234=VECTOR('',#39551,10.);
#11235=VECTOR('',#39556,10.);
#11236=VECTOR('',#39557,10.);
#11237=VECTOR('',#39562,10.);
#11238=VECTOR('',#39563,10.);
#11239=VECTOR('',#39568,10.);
#11240=VECTOR('',#39569,10.);
#11241=VECTOR('',#39574,10.);
#11242=VECTOR('',#39575,10.);
#11243=VECTOR('',#39580,10.);
#11244=VECTOR('',#39589,10.);
#11245=VECTOR('',#39594,10.);
#11246=VECTOR('',#39597,10.);
#11247=VECTOR('',#39600,10.);
#11248=VECTOR('',#39601,10.);
#11249=VECTOR('',#39602,10.);
#11250=VECTOR('',#39609,10.);
#11251=VECTOR('',#39612,10.);
#11252=VECTOR('',#39613,10.);
#11253=VECTOR('',#39614,10.);
#11254=VECTOR('',#39621,10.);
#11255=VECTOR('',#39624,10.);
#11256=VECTOR('',#39625,10.);
#11257=VECTOR('',#39626,10.);
#11258=VECTOR('',#39633,10.);
#11259=VECTOR('',#39636,10.);
#11260=VECTOR('',#39637,10.);
#11261=VECTOR('',#39640,10.);
#11262=VECTOR('',#39641,10.);
#11263=VECTOR('',#39642,10.);
#11264=VECTOR('',#39643,10.);
#11265=VECTOR('',#39650,10.);
#11266=VECTOR('',#39653,10.);
#11267=VECTOR('',#39656,10.);
#11268=VECTOR('',#39659,10.);
#11269=VECTOR('',#39664,10.);
#11270=VECTOR('',#39667,10.);
#11271=VECTOR('',#39670,10.);
#11272=VECTOR('',#39671,10.);
#11273=VECTOR('',#39676,10.);
#11274=VECTOR('',#39679,10.);
#11275=VECTOR('',#39680,10.);
#11276=VECTOR('',#39685,10.);
#11277=VECTOR('',#39688,10.);
#11278=VECTOR('',#39689,10.);
#11279=VECTOR('',#39694,10.);
#11280=VECTOR('',#39697,10.);
#11281=VECTOR('',#39730,4.08940000000001);
#11282=VECTOR('',#39761,4.0894);
#11283=VECTOR('',#39764,10.);
#11284=VECTOR('',#39765,10.);
#11285=VECTOR('',#39766,10.);
#11286=VECTOR('',#39769,10.);
#11287=VECTOR('',#39770,10.);
#11288=VECTOR('',#39773,10.);
#11289=VECTOR('',#39774,10.);
#11290=VECTOR('',#39777,10.);
#11291=VECTOR('',#39778,10.);
#11292=VECTOR('',#39781,10.);
#11293=VECTOR('',#39782,10.);
#11294=VECTOR('',#39785,9.99999999999999);
#11295=VECTOR('',#39786,10.);
#11296=VECTOR('',#39789,10.);
#11297=VECTOR('',#39790,10.);
#11298=VECTOR('',#39793,10.);
#11299=VECTOR('',#39794,10.);
#11300=VECTOR('',#39797,10.);
#11301=VECTOR('',#39798,10.);
#11302=VECTOR('',#39801,10.);
#11303=VECTOR('',#39802,10.);
#11304=VECTOR('',#39805,10.);
#11305=VECTOR('',#39806,10.);
#11306=VECTOR('',#39809,10.);
#11307=VECTOR('',#39814,10.);
#11308=VECTOR('',#39815,10.);
#11309=VECTOR('',#39816,10.);
#11310=VECTOR('',#39819,10.);
#11311=VECTOR('',#39820,10.);
#11312=VECTOR('',#39823,10.);
#11313=VECTOR('',#39824,10.);
#11314=VECTOR('',#39827,10.);
#11315=VECTOR('',#39828,10.);
#11316=VECTOR('',#39831,10.);
#11317=VECTOR('',#39832,10.);
#11318=VECTOR('',#39835,10.);
#11319=VECTOR('',#39836,10.);
#11320=VECTOR('',#39839,10.);
#11321=VECTOR('',#39840,10.);
#11322=VECTOR('',#39843,10.);
#11323=VECTOR('',#39844,10.);
#11324=VECTOR('',#39847,10.);
#11325=VECTOR('',#39848,10.);
#11326=VECTOR('',#39851,10.);
#11327=VECTOR('',#39852,10.);
#11328=VECTOR('',#39855,10.);
#11329=VECTOR('',#39856,10.);
#11330=VECTOR('',#39859,10.);
#11331=VECTOR('',#39864,10.);
#11332=VECTOR('',#39865,10.);
#11333=VECTOR('',#39866,10.);
#11334=VECTOR('',#39867,10.);
#11335=VECTOR('',#39868,10.);
#11336=VECTOR('',#39869,10.);
#11337=VECTOR('',#39870,10.);
#11338=VECTOR('',#39871,10.);
#11339=VECTOR('',#39872,10.);
#11340=VECTOR('',#39875,10.);
#11341=VECTOR('',#39878,10.);
#11342=VECTOR('',#39881,10.);
#11343=VECTOR('',#39884,10.);
#11344=VECTOR('',#39887,10.);
#11345=VECTOR('',#39890,10.);
#11346=VECTOR('',#39893,10.);
#11347=VECTOR('',#39896,10.);
#11348=VECTOR('',#39901,10.);
#11349=VECTOR('',#39902,10.);
#11350=VECTOR('',#39905,10.);
#11351=VECTOR('',#39906,10.);
#11352=VECTOR('',#39917,10.);
#11353=VECTOR('',#39918,10.);
#11354=VECTOR('',#39921,10.);
#11355=VECTOR('',#39922,10.);
#11356=VECTOR('',#39929,10.);
#11357=VECTOR('',#39930,10.);
#11358=VECTOR('',#39939,10.);
#11359=VECTOR('',#39942,10.);
#11360=VECTOR('',#39951,10.);
#11361=VECTOR('',#39952,10.);
#11362=VECTOR('',#39953,10.);
#11363=VECTOR('',#39956,10.);
#11364=VECTOR('',#39957,10.);
#11365=VECTOR('',#39960,10.);
#11366=VECTOR('',#39961,10.);
#11367=VECTOR('',#39964,10.);
#11368=VECTOR('',#39965,10.);
#11369=VECTOR('',#39968,10.);
#11370=VECTOR('',#39969,10.);
#11371=VECTOR('',#39972,10.);
#11372=VECTOR('',#39973,10.);
#11373=VECTOR('',#39976,10.);
#11374=VECTOR('',#39977,10.);
#11375=VECTOR('',#39980,10.);
#11376=VECTOR('',#39981,10.);
#11377=VECTOR('',#39984,10.);
#11378=VECTOR('',#39985,10.);
#11379=VECTOR('',#39988,10.);
#11380=VECTOR('',#39989,10.);
#11381=VECTOR('',#39992,10.);
#11382=VECTOR('',#39993,10.);
#11383=VECTOR('',#39996,11.1759999999998);
#11384=VECTOR('',#40003,10.);
#11385=VECTOR('',#40030,10.);
#11386=VECTOR('',#40031,10.);
#11387=VECTOR('',#40032,10.);
#11388=VECTOR('',#40033,10.);
#11389=VECTOR('',#40034,10.);
#11390=VECTOR('',#40035,10.);
#11391=VECTOR('',#40036,10.);
#11392=VECTOR('',#40037,10.);
#11393=VECTOR('',#40038,10.);
#11394=VECTOR('',#40039,10.);
#11395=VECTOR('',#40042,10.);
#11396=VECTOR('',#40045,10.);
#11397=VECTOR('',#40048,10.);
#11398=VECTOR('',#40051,10.);
#11399=VECTOR('',#40054,10.);
#11400=VECTOR('',#40057,10.);
#11401=VECTOR('',#40060,10.);
#11402=VECTOR('',#40063,10.);
#11403=VECTOR('',#40066,10.);
#11404=VECTOR('',#40077,4.12749999999997);
#11405=VECTOR('',#40090,4.12750000000001);
#11406=VECTOR('',#40103,4.12749999999996);
#11407=VECTOR('',#40130,90.9319999999999);
#11408=VECTOR('',#40139,82.931);
#11409=VECTOR('',#40148,10.);
#11410=VECTOR('',#40149,10.);
#11411=VECTOR('',#40150,10.);
#11412=VECTOR('',#40153,10.);
#11413=VECTOR('',#40154,10.);
#11414=VECTOR('',#40155,10.);
#11415=VECTOR('',#40156,10.);
#11416=VECTOR('',#40157,10.);
#11417=VECTOR('',#40158,10.);
#11418=VECTOR('',#40159,10.);
#11419=VECTOR('',#40160,10.);
#11420=VECTOR('',#40161,10.);
#11421=VECTOR('',#40162,10.);
#11422=VECTOR('',#40163,10.);
#11423=VECTOR('',#40164,10.);
#11424=VECTOR('',#40165,10.);
#11425=VECTOR('',#40166,10.);
#11426=VECTOR('',#40167,10.);
#11427=VECTOR('',#40172,10.);
#11428=VECTOR('',#40175,10.);
#11429=VECTOR('',#40176,10.);
#11430=VECTOR('',#40177,10.);
#11431=VECTOR('',#40178,10.);
#11432=VECTOR('',#40179,10.);
#11433=VECTOR('',#40180,10.);
#11434=VECTOR('',#40183,10.);
#11435=VECTOR('',#40184,10.);
#11436=VECTOR('',#40185,10.);
#11437=VECTOR('',#40186,10.);
#11438=VECTOR('',#40187,10.);
#11439=VECTOR('',#40188,10.);
#11440=VECTOR('',#40191,10.);
#11441=VECTOR('',#40194,10.);
#11442=VECTOR('',#40199,10.);
#11443=VECTOR('',#40202,10.);
#11444=VECTOR('',#40207,10.);
#11445=VECTOR('',#40208,10.);
#11446=VECTOR('',#40211,10.);
#11447=VECTOR('',#40212,10.);
#11448=VECTOR('',#40217,10.);
#11449=VECTOR('',#40220,10.);
#11450=VECTOR('',#40223,10.);
#11451=VECTOR('',#40226,10.);
#11452=VECTOR('',#40237,10.);
#11453=VECTOR('',#40238,10.);
#11454=VECTOR('',#40241,10.);
#11455=VECTOR('',#40242,10.);
#11456=VECTOR('',#40247,10.);
#11457=VECTOR('',#40250,10.);
#11458=VECTOR('',#40257,3.90270999999991);
#11459=VECTOR('',#40264,3.98868900000005);
#11460=VECTOR('',#40273,3.90270999999999);
#11461=VECTOR('',#40280,3.98868900000002);
#11462=VECTOR('',#40289,3.90271000000012);
#11463=VECTOR('',#40296,3.98868900000004);
#11464=VECTOR('',#40305,3.90271);
#11465=VECTOR('',#40312,3.98868900000001);
#11466=VECTOR('',#40317,82.8587325401841);
#11467=VECTOR('',#40334,57.15);
#11468=VECTOR('',#40343,52.451);
#11469=VECTOR('',#40352,13.081);
#11470=VECTOR('',#40361,12.446);
#11471=VECTOR('',#40370,8.76299999999995);
#11472=VECTOR('',#40373,2.794);
#11473=VECTOR('',#40382,8.76299999999997);
#11474=VECTOR('',#40391,2.794);
#11475=VECTOR('',#40402,2.79400000000002);
#11476=VECTOR('',#40409,8.76300000000001);
#11477=VECTOR('',#40414,8.763);
#11478=VECTOR('',#40423,2.79399999999998);
#11479=VECTOR('',#40428,10.);
#11480=VECTOR('',#40429,10.);
#11481=VECTOR('',#40430,10.);
#11482=VECTOR('',#40431,10.);
#11483=VECTOR('',#40432,10.);
#11484=VECTOR('',#40435,10.);
#11485=VECTOR('',#40442,10.);
#11486=VECTOR('',#40443,10.);
#11487=VECTOR('',#40444,10.);
#11488=VECTOR('',#40445,10.);
#11489=VECTOR('',#40476,2.18439999999999);
#11490=VECTOR('',#40519,2.18440000000006);
#11491=VECTOR('',#40560,10.);
#11492=VECTOR('',#40561,10.);
#11493=VECTOR('',#40562,10.);
#11494=VECTOR('',#40565,10.);
#11495=VECTOR('',#40566,10.);
#11496=VECTOR('',#40569,10.);
#11497=VECTOR('',#40570,10.);
#11498=VECTOR('',#40573,10.);
#11499=VECTOR('',#40574,10.);
#11500=VECTOR('',#40577,10.);
#11501=VECTOR('',#40578,10.);
#11502=VECTOR('',#40581,10.);
#11503=VECTOR('',#40582,10.);
#11504=VECTOR('',#40585,10.);
#11505=VECTOR('',#40586,10.);
#11506=VECTOR('',#40589,10.);
#11507=VECTOR('',#40590,10.);
#11508=VECTOR('',#40593,10.);
#11509=VECTOR('',#40594,10.);
#11510=VECTOR('',#40597,10.);
#11511=VECTOR('',#40598,10.);
#11512=VECTOR('',#40601,10.);
#11513=VECTOR('',#40602,10.);
#11514=VECTOR('',#40605,10.);
#11515=VECTOR('',#40606,10.);
#11516=VECTOR('',#40609,10.);
#11517=VECTOR('',#40610,10.);
#11518=VECTOR('',#40613,10.);
#11519=VECTOR('',#40614,10.);
#11520=VECTOR('',#40617,10.);
#11521=VECTOR('',#40618,10.);
#11522=VECTOR('',#40621,10.);
#11523=VECTOR('',#40626,10.);
#11524=VECTOR('',#40629,10.);
#11525=VECTOR('',#40632,10.);
#11526=VECTOR('',#40635,10.);
#11527=VECTOR('',#40638,10.);
#11528=VECTOR('',#40641,10.);
#11529=VECTOR('',#40644,10.);
#11530=VECTOR('',#40647,10.);
#11531=VECTOR('',#40650,10.);
#11532=VECTOR('',#40653,10.);
#11533=VECTOR('',#40656,10.);
#11534=VECTOR('',#40659,10.);
#11535=VECTOR('',#40662,10.);
#11536=VECTOR('',#40671,10.);
#11537=VECTOR('',#40674,10.);
#11538=VECTOR('',#40677,10.);
#11539=VECTOR('',#40678,10.);
#11540=VECTOR('',#40679,10.);
#11541=VECTOR('',#40680,10.);
#11542=VECTOR('',#40681,10.);
#11543=VECTOR('',#40682,10.);
#11544=VECTOR('',#40683,10.);
#11545=VECTOR('',#40684,10.);
#11546=VECTOR('',#40685,10.);
#11547=VECTOR('',#40686,10.);
#11548=VECTOR('',#40687,10.);
#11549=VECTOR('',#40692,10.);
#11550=VECTOR('',#40693,10.);
#11551=VECTOR('',#40694,10.);
#11552=VECTOR('',#40695,10.);
#11553=VECTOR('',#40704,10.);
#11554=VECTOR('',#40709,10.);
#11555=VECTOR('',#40710,10.);
#11556=VECTOR('',#40711,10.);
#11557=VECTOR('',#40712,10.);
#11558=VECTOR('',#40713,10.);
#11559=VECTOR('',#40714,10.);
#11560=VECTOR('',#40715,10.);
#11561=VECTOR('',#40716,10.);
#11562=VECTOR('',#40719,10.);
#11563=VECTOR('',#40720,10.);
#11564=VECTOR('',#40721,10.);
#11565=VECTOR('',#40722,10.);
#11566=VECTOR('',#40731,10.);
#11567=VECTOR('',#40740,10.);
#11568=VECTOR('',#40741,10.);
#11569=VECTOR('',#40742,10.);
#11570=VECTOR('',#40745,10.);
#11571=VECTOR('',#40748,10.);
#11572=VECTOR('',#40751,10.);
#11573=VECTOR('',#40752,10.);
#11574=VECTOR('',#40753,10.);
#11575=VECTOR('',#40754,10.);
#11576=VECTOR('',#40761,10.);
#11577=VECTOR('',#40846,10.);
#11578=VECTOR('',#40847,10.);
#11579=VECTOR('',#40852,10.);
#11580=VECTOR('',#40853,10.);
#11581=VECTOR('',#40864,10.);
#11582=VECTOR('',#40867,10.);
#11583=VECTOR('',#40868,10.);
#11584=VECTOR('',#40881,10.);
#11585=VECTOR('',#40884,10.);
#11586=VECTOR('',#40887,10.);
#11587=VECTOR('',#40888,10.);
#11588=VECTOR('',#40891,10.);
#11589=VECTOR('',#40892,10.);
#11590=VECTOR('',#40895,10.);
#11591=VECTOR('',#40898,10.);
#11592=VECTOR('',#40899,10.);
#11593=VECTOR('',#40902,10.);
#11594=VECTOR('',#40903,10.);
#11595=VECTOR('',#40906,10.);
#11596=VECTOR('',#40909,10.);
#11597=VECTOR('',#40910,10.);
#11598=VECTOR('',#40913,10.);
#11599=VECTOR('',#40914,10.);
#11600=VECTOR('',#40917,10.);
#11601=VECTOR('',#40920,10.);
#11602=VECTOR('',#40921,10.);
#11603=VECTOR('',#40924,10.);
#11604=VECTOR('',#40925,10.);
#11605=VECTOR('',#40930,10.);
#11606=VECTOR('',#40935,10.);
#11607=VECTOR('',#40938,10.);
#11608=VECTOR('',#40939,10.);
#11609=VECTOR('',#40940,10.);
#11610=VECTOR('',#40941,10.);
#11611=VECTOR('',#40944,10.);
#11612=VECTOR('',#40945,10.);
#11613=VECTOR('',#40946,10.);
#11614=VECTOR('',#40949,10.);
#11615=VECTOR('',#40950,10.);
#11616=VECTOR('',#40951,10.);
#11617=VECTOR('',#40952,10.);
#11618=VECTOR('',#40959,10.);
#11619=VECTOR('',#40960,10.);
#11620=VECTOR('',#40961,10.);
#11621=VECTOR('',#40962,10.);
#11622=VECTOR('',#40979,5.68799999999971);
#11623=VECTOR('',#40982,5.188);
#11624=VECTOR('',#40991,5.68799999999971);
#11625=VECTOR('',#40994,5.188);
#11626=VECTOR('',#41003,5.68799999999971);
#11627=VECTOR('',#41006,5.188);
#11628=VECTOR('',#41015,5.68799999999971);
#11629=VECTOR('',#41018,5.188);
#11630=VECTOR('',#41025,5.688);
#11631=VECTOR('',#41028,5.688);
#11632=VECTOR('',#41031,5.688);
#11633=VECTOR('',#41034,5.688);
#11634=VECTOR('',#41037,10.);
#11635=VECTOR('',#41042,10.);
#11636=VECTOR('',#41043,10.);
#11637=VECTOR('',#41044,10.);
#11638=VECTOR('',#41047,10.);
#11639=VECTOR('',#41050,10.);
#11640=VECTOR('',#41055,10.);
#11641=VECTOR('',#41056,10.);
#11642=VECTOR('',#41059,10.);
#11643=VECTOR('',#41064,10.);
#11644=VECTOR('',#41069,10.);
#11645=VECTOR('',#41070,10.);
#11646=VECTOR('',#41073,10.);
#11647=VECTOR('',#41076,10.);
#11648=VECTOR('',#41083,10.);
#11649=VECTOR('',#41084,10.);
#11650=VECTOR('',#41085,10.);
#11651=VECTOR('',#41086,10.);
#11652=VECTOR('',#41091,10.);
#11653=VECTOR('',#41096,10.);
#11654=VECTOR('',#41097,10.);
#11655=VECTOR('',#41098,10.);
#11656=VECTOR('',#41103,10.);
#11657=VECTOR('',#41108,10.);
#11658=VECTOR('',#41109,10.);
#11659=VECTOR('',#41110,10.);
#11660=VECTOR('',#41111,10.);
#11661=VECTOR('',#41116,10.);
#11662=VECTOR('',#41121,10.);
#11663=VECTOR('',#41122,10.);
#11664=VECTOR('',#41123,10.);
#11665=VECTOR('',#41128,10.);
#11666=VECTOR('',#41133,10.);
#11667=VECTOR('',#41134,10.);
#11668=VECTOR('',#41135,10.);
#11669=VECTOR('',#41142,10.);
#11670=VECTOR('',#41145,10.);
#11671=VECTOR('',#41146,10.);
#11672=VECTOR('',#41147,10.);
#11673=VECTOR('',#41156,10.);
#11674=VECTOR('',#41157,10.);
#11675=VECTOR('',#41158,10.);
#11676=VECTOR('',#41163,10.);
#11677=VECTOR('',#41168,10.);
#11678=VECTOR('',#41169,10.);
#11679=VECTOR('',#41170,10.);
#11680=VECTOR('',#41183,10.);
#11681=VECTOR('',#41184,10.);
#11682=VECTOR('',#41185,10.);
#11683=VECTOR('',#41186,10.);
#11684=VECTOR('',#41191,10.);
#11685=VECTOR('',#41196,10.);
#11686=VECTOR('',#41197,10.);
#11687=VECTOR('',#41198,10.);
#11688=VECTOR('',#41203,10.);
#11689=VECTOR('',#41208,10.);
#11690=VECTOR('',#41209,10.);
#11691=VECTOR('',#41210,10.);
#11692=VECTOR('',#41211,10.);
#11693=VECTOR('',#41216,10.);
#11694=VECTOR('',#41221,10.);
#11695=VECTOR('',#41222,10.);
#11696=VECTOR('',#41223,10.);
#11697=VECTOR('',#41228,10.);
#11698=VECTOR('',#41233,10.);
#11699=VECTOR('',#41234,10.);
#11700=VECTOR('',#41235,10.);
#11701=VECTOR('',#41242,10.);
#11702=VECTOR('',#41245,10.);
#11703=VECTOR('',#41246,10.);
#11704=VECTOR('',#41247,10.);
#11705=VECTOR('',#41256,10.);
#11706=VECTOR('',#41257,10.);
#11707=VECTOR('',#41258,10.);
#11708=VECTOR('',#41263,10.);
#11709=VECTOR('',#41268,10.);
#11710=VECTOR('',#41269,10.);
#11711=VECTOR('',#41270,10.);
#11712=VECTOR('',#41283,10.);
#11713=VECTOR('',#41284,10.);
#11714=VECTOR('',#41285,10.);
#11715=VECTOR('',#41286,10.);
#11716=VECTOR('',#41291,10.);
#11717=VECTOR('',#41296,10.);
#11718=VECTOR('',#41297,10.);
#11719=VECTOR('',#41298,10.);
#11720=VECTOR('',#41303,10.);
#11721=VECTOR('',#41308,10.);
#11722=VECTOR('',#41309,10.);
#11723=VECTOR('',#41310,10.);
#11724=VECTOR('',#41311,10.);
#11725=VECTOR('',#41316,10.);
#11726=VECTOR('',#41321,10.);
#11727=VECTOR('',#41322,10.);
#11728=VECTOR('',#41323,10.);
#11729=VECTOR('',#41328,10.);
#11730=VECTOR('',#41333,10.);
#11731=VECTOR('',#41334,10.);
#11732=VECTOR('',#41335,10.);
#11733=VECTOR('',#41342,10.);
#11734=VECTOR('',#41345,10.);
#11735=VECTOR('',#41346,10.);
#11736=VECTOR('',#41347,10.);
#11737=VECTOR('',#41356,10.);
#11738=VECTOR('',#41357,10.);
#11739=VECTOR('',#41358,10.);
#11740=VECTOR('',#41363,10.);
#11741=VECTOR('',#41368,10.);
#11742=VECTOR('',#41369,10.);
#11743=VECTOR('',#41370,10.);
#11744=VECTOR('',#41383,10.);
#11745=VECTOR('',#41384,10.);
#11746=VECTOR('',#41385,10.);
#11747=VECTOR('',#41386,10.);
#11748=VECTOR('',#41391,10.);
#11749=VECTOR('',#41396,10.);
#11750=VECTOR('',#41397,10.);
#11751=VECTOR('',#41398,10.);
#11752=VECTOR('',#41403,10.);
#11753=VECTOR('',#41408,10.);
#11754=VECTOR('',#41409,10.);
#11755=VECTOR('',#41410,10.);
#11756=VECTOR('',#41411,10.);
#11757=VECTOR('',#41416,10.);
#11758=VECTOR('',#41421,10.);
#11759=VECTOR('',#41422,10.);
#11760=VECTOR('',#41423,10.);
#11761=VECTOR('',#41428,10.);
#11762=VECTOR('',#41433,10.);
#11763=VECTOR('',#41434,10.);
#11764=VECTOR('',#41435,10.);
#11765=VECTOR('',#41442,10.);
#11766=VECTOR('',#41445,10.);
#11767=VECTOR('',#41446,10.);
#11768=VECTOR('',#41447,10.);
#11769=VECTOR('',#41456,10.);
#11770=VECTOR('',#41457,10.);
#11771=VECTOR('',#41458,10.);
#11772=VECTOR('',#41463,10.);
#11773=VECTOR('',#41468,10.);
#11774=VECTOR('',#41469,10.);
#11775=VECTOR('',#41470,10.);
#11776=VECTOR('',#41485,10.);
#11777=VECTOR('',#41488,10.);
#11778=VECTOR('',#41491,10.);
#11779=VECTOR('',#41494,10.);
#11780=VECTOR('',#41495,10.);
#11781=VECTOR('',#41498,10.);
#11782=VECTOR('',#41501,10.);
#11783=VECTOR('',#41504,10.);
#11784=VECTOR('',#41509,10.);
#11785=VECTOR('',#41510,10.);
#11786=VECTOR('',#41511,10.);
#11787=VECTOR('',#41514,10.);
#11788=VECTOR('',#41519,10.);
#11789=VECTOR('',#41520,10.);
#11790=VECTOR('',#41523,10.);
#11791=VECTOR('',#41528,10.);
#11792=VECTOR('',#41531,10.);
#11793=VECTOR('',#41534,10.);
#11794=VECTOR('',#41537,10.);
#11795=VECTOR('',#41540,10.);
#11796=VECTOR('',#41541,10.);
#11797=VECTOR('',#41544,10.);
#11798=VECTOR('',#41547,10.);
#11799=VECTOR('',#41550,10.);
#11800=VECTOR('',#41551,10.);
#11801=VECTOR('',#41554,10.);
#11802=VECTOR('',#41559,10.);
#11803=VECTOR('',#41562,10.);
#11804=VECTOR('',#41565,10.);
#11805=VECTOR('',#41568,10.);
#11806=VECTOR('',#41575,10.);
#11807=VECTOR('',#41578,10.);
#11808=VECTOR('',#41585,10.);
#11809=VECTOR('',#41588,10.);
#11810=VECTOR('',#41591,10.);
#11811=VECTOR('',#41594,10.);
#11812=VECTOR('',#41595,10.);
#11813=VECTOR('',#41598,10.);
#11814=VECTOR('',#41601,10.);
#11815=VECTOR('',#41604,10.);
#11816=VECTOR('',#41609,10.);
#11817=VECTOR('',#41610,10.);
#11818=VECTOR('',#41611,10.);
#11819=VECTOR('',#41614,10.);
#11820=VECTOR('',#41619,10.);
#11821=VECTOR('',#41620,10.);
#11822=VECTOR('',#41623,10.);
#11823=VECTOR('',#41628,10.);
#11824=VECTOR('',#41631,10.);
#11825=VECTOR('',#41634,10.);
#11826=VECTOR('',#41635,10.);
#11827=VECTOR('',#41638,10.);
#11828=VECTOR('',#41643,10.);
#11829=VECTOR('',#41644,10.);
#11830=VECTOR('',#41649,10.);
#11831=VECTOR('',#41652,10.);
#11832=VECTOR('',#41653,10.);
#11833=VECTOR('',#41656,10.);
#11834=VECTOR('',#41661,10.);
#11835=VECTOR('',#41664,10.);
#11836=VECTOR('',#41667,10.);
#11837=VECTOR('',#41670,10.);
#11838=VECTOR('',#41675,10.);
#11839=VECTOR('',#41678,10.);
#11840=VECTOR('',#41683,10.);
#11841=VECTOR('',#41686,10.);
#11842=VECTOR('',#41689,10.);
#11843=VECTOR('',#41692,10.);
#11844=VECTOR('',#41695,10.);
#11845=VECTOR('',#41698,10.);
#11846=VECTOR('',#41701,10.);
#11847=VECTOR('',#41704,10.);
#11848=VECTOR('',#41709,10.);
#11849=VECTOR('',#41710,10.);
#11850=VECTOR('',#41711,10.);
#11851=VECTOR('',#41714,10.);
#11852=VECTOR('',#41719,10.);
#11853=VECTOR('',#41720,10.);
#11854=VECTOR('',#41723,10.);
#11855=VECTOR('',#41728,10.);
#11856=VECTOR('',#41729,10.);
#11857=VECTOR('',#41730,10.);
#11858=VECTOR('',#41733,10.);
#11859=VECTOR('',#41738,10.);
#11860=VECTOR('',#41739,10.);
#11861=VECTOR('',#41742,10.);
#11862=VECTOR('',#41747,10.);
#11863=VECTOR('',#41750,10.);
#11864=VECTOR('',#41753,10.);
#11865=VECTOR('',#41756,10.);
#11866=VECTOR('',#41761,10.);
#11867=VECTOR('',#41764,10.);
#11868=VECTOR('',#41767,10.);
#11869=VECTOR('',#41770,10.);
#11870=VECTOR('',#41775,10.);
#11871=VECTOR('',#41778,10.);
#11872=VECTOR('',#41783,10.);
#11873=VECTOR('',#41786,10.);
#11874=VECTOR('',#41789,10.);
#11875=VECTOR('',#41792,10.);
#11876=VECTOR('',#41795,10.);
#11877=VECTOR('',#41798,10.);
#11878=VECTOR('',#41801,10.);
#11879=VECTOR('',#41804,10.);
#11880=VECTOR('',#41809,10.);
#11881=VECTOR('',#41810,10.);
#11882=VECTOR('',#41811,10.);
#11883=VECTOR('',#41814,10.);
#11884=VECTOR('',#41819,10.);
#11885=VECTOR('',#41820,10.);
#11886=VECTOR('',#41823,10.);
#11887=VECTOR('',#41828,10.);
#11888=VECTOR('',#41829,10.);
#11889=VECTOR('',#41830,10.);
#11890=VECTOR('',#41833,10.);
#11891=VECTOR('',#41838,10.);
#11892=VECTOR('',#41839,10.);
#11893=VECTOR('',#41842,10.);
#11894=VECTOR('',#41847,10.);
#11895=VECTOR('',#41850,10.);
#11896=VECTOR('',#41853,10.);
#11897=VECTOR('',#41856,10.);
#11898=VECTOR('',#41861,10.);
#11899=VECTOR('',#41864,10.);
#11900=VECTOR('',#41867,10.);
#11901=VECTOR('',#41870,10.);
#11902=VECTOR('',#41875,10.);
#11903=VECTOR('',#41878,10.);
#11904=VECTOR('',#41883,10.);
#11905=VECTOR('',#41884,10.);
#11906=VECTOR('',#41885,10.);
#11907=VECTOR('',#41886,10.);
#11908=VECTOR('',#41891,10.);
#11909=VECTOR('',#41896,10.);
#11910=VECTOR('',#41897,10.);
#11911=VECTOR('',#41898,10.);
#11912=VECTOR('',#41903,10.);
#11913=VECTOR('',#41908,10.);
#11914=VECTOR('',#41909,10.);
#11915=VECTOR('',#41910,10.);
#11916=VECTOR('',#41911,10.);
#11917=VECTOR('',#41916,10.);
#11918=VECTOR('',#41921,10.);
#11919=VECTOR('',#41922,10.);
#11920=VECTOR('',#41923,10.);
#11921=VECTOR('',#41928,10.);
#11922=VECTOR('',#41933,10.);
#11923=VECTOR('',#41934,10.);
#11924=VECTOR('',#41935,10.);
#11925=VECTOR('',#41942,10.);
#11926=VECTOR('',#41945,10.);
#11927=VECTOR('',#41946,10.);
#11928=VECTOR('',#41947,10.);
#11929=VECTOR('',#41956,10.);
#11930=VECTOR('',#41957,10.);
#11931=VECTOR('',#41958,10.);
#11932=VECTOR('',#41963,10.);
#11933=VECTOR('',#41968,10.);
#11934=VECTOR('',#41969,10.);
#11935=VECTOR('',#41970,10.);
#11936=VECTOR('',#41983,10.);
#11937=VECTOR('',#41984,10.);
#11938=VECTOR('',#41985,10.);
#11939=VECTOR('',#41986,10.);
#11940=VECTOR('',#41991,10.);
#11941=VECTOR('',#41996,10.);
#11942=VECTOR('',#41997,10.);
#11943=VECTOR('',#41998,10.);
#11944=VECTOR('',#42003,10.);
#11945=VECTOR('',#42008,10.);
#11946=VECTOR('',#42009,10.);
#11947=VECTOR('',#42010,10.);
#11948=VECTOR('',#42011,10.);
#11949=VECTOR('',#42016,10.);
#11950=VECTOR('',#42021,10.);
#11951=VECTOR('',#42022,10.);
#11952=VECTOR('',#42023,10.);
#11953=VECTOR('',#42028,10.);
#11954=VECTOR('',#42033,10.);
#11955=VECTOR('',#42034,10.);
#11956=VECTOR('',#42035,10.);
#11957=VECTOR('',#42042,10.);
#11958=VECTOR('',#42045,10.);
#11959=VECTOR('',#42046,10.);
#11960=VECTOR('',#42047,10.);
#11961=VECTOR('',#42056,10.);
#11962=VECTOR('',#42057,10.);
#11963=VECTOR('',#42058,10.);
#11964=VECTOR('',#42063,10.);
#11965=VECTOR('',#42068,10.);
#11966=VECTOR('',#42069,10.);
#11967=VECTOR('',#42070,10.);
#11968=VECTOR('',#42083,10.);
#11969=VECTOR('',#42084,10.);
#11970=VECTOR('',#42085,10.);
#11971=VECTOR('',#42086,10.);
#11972=VECTOR('',#42091,10.);
#11973=VECTOR('',#42096,10.);
#11974=VECTOR('',#42097,10.);
#11975=VECTOR('',#42098,10.);
#11976=VECTOR('',#42103,10.);
#11977=VECTOR('',#42108,10.);
#11978=VECTOR('',#42109,10.);
#11979=VECTOR('',#42110,10.);
#11980=VECTOR('',#42111,10.);
#11981=VECTOR('',#42116,10.);
#11982=VECTOR('',#42121,10.);
#11983=VECTOR('',#42122,10.);
#11984=VECTOR('',#42123,10.);
#11985=VECTOR('',#42128,10.);
#11986=VECTOR('',#42133,10.);
#11987=VECTOR('',#42134,10.);
#11988=VECTOR('',#42135,10.);
#11989=VECTOR('',#42142,10.);
#11990=VECTOR('',#42145,10.);
#11991=VECTOR('',#42146,10.);
#11992=VECTOR('',#42147,10.);
#11993=VECTOR('',#42156,10.);
#11994=VECTOR('',#42157,10.);
#11995=VECTOR('',#42158,10.);
#11996=VECTOR('',#42163,10.);
#11997=VECTOR('',#42168,10.);
#11998=VECTOR('',#42169,10.);
#11999=VECTOR('',#42170,10.);
#12000=VECTOR('',#42185,10.);
#12001=VECTOR('',#42188,10.);
#12002=VECTOR('',#42191,10.);
#12003=VECTOR('',#42192,10.);
#12004=VECTOR('',#42193,10.);
#12005=VECTOR('',#42198,10.);
#12006=VECTOR('',#42203,10.);
#12007=VECTOR('',#42204,10.);
#12008=VECTOR('',#42205,10.);
#12009=VECTOR('',#42210,10.);
#12010=VECTOR('',#42215,10.);
#12011=VECTOR('',#42216,10.);
#12012=VECTOR('',#42217,10.);
#12013=VECTOR('',#42222,10.);
#12014=VECTOR('',#42227,10.);
#12015=VECTOR('',#42228,10.);
#12016=VECTOR('',#42233,10.);
#12017=VECTOR('',#42236,10.);
#12018=VECTOR('',#42239,10.);
#12019=VECTOR('',#42240,10.);
#12020=VECTOR('',#42241,10.);
#12021=VECTOR('',#42248,10.);
#12022=VECTOR('',#42251,10.);
#12023=VECTOR('',#42252,10.);
#12024=VECTOR('',#42253,10.);
#12025=VECTOR('',#42260,10.);
#12026=VECTOR('',#42263,10.);
#12027=VECTOR('',#42264,10.);
#12028=VECTOR('',#42265,10.);
#12029=VECTOR('',#42272,10.);
#12030=VECTOR('',#42275,10.);
#12031=VECTOR('',#42276,10.);
#12032=VECTOR('',#42285,10.);
#12033=VECTOR('',#42288,10.);
#12034=VECTOR('',#42291,10.);
#12035=VECTOR('',#42292,10.);
#12036=VECTOR('',#42293,10.);
#12037=VECTOR('',#42298,10.);
#12038=VECTOR('',#42303,10.);
#12039=VECTOR('',#42304,10.);
#12040=VECTOR('',#42305,10.);
#12041=VECTOR('',#42310,10.);
#12042=VECTOR('',#42315,10.);
#12043=VECTOR('',#42316,10.);
#12044=VECTOR('',#42317,10.);
#12045=VECTOR('',#42322,10.);
#12046=VECTOR('',#42327,10.);
#12047=VECTOR('',#42328,10.);
#12048=VECTOR('',#42333,10.);
#12049=VECTOR('',#42336,10.);
#12050=VECTOR('',#42339,10.);
#12051=VECTOR('',#42340,10.);
#12052=VECTOR('',#42341,10.);
#12053=VECTOR('',#42348,10.);
#12054=VECTOR('',#42351,10.);
#12055=VECTOR('',#42352,10.);
#12056=VECTOR('',#42353,10.);
#12057=VECTOR('',#42360,10.);
#12058=VECTOR('',#42363,10.);
#12059=VECTOR('',#42364,10.);
#12060=VECTOR('',#42365,10.);
#12061=VECTOR('',#42372,10.);
#12062=VECTOR('',#42375,10.);
#12063=VECTOR('',#42376,10.);
#12064=VECTOR('',#42385,10.);
#12065=VECTOR('',#42388,10.);
#12066=VECTOR('',#42391,10.);
#12067=VECTOR('',#42392,10.);
#12068=VECTOR('',#42393,10.);
#12069=VECTOR('',#42398,10.);
#12070=VECTOR('',#42403,10.);
#12071=VECTOR('',#42404,10.);
#12072=VECTOR('',#42405,10.);
#12073=VECTOR('',#42410,10.);
#12074=VECTOR('',#42415,10.);
#12075=VECTOR('',#42416,10.);
#12076=VECTOR('',#42417,10.);
#12077=VECTOR('',#42422,10.);
#12078=VECTOR('',#42427,10.);
#12079=VECTOR('',#42428,10.);
#12080=VECTOR('',#42433,10.);
#12081=VECTOR('',#42436,10.);
#12082=VECTOR('',#42439,10.);
#12083=VECTOR('',#42440,10.);
#12084=VECTOR('',#42441,10.);
#12085=VECTOR('',#42448,10.);
#12086=VECTOR('',#42451,10.);
#12087=VECTOR('',#42452,10.);
#12088=VECTOR('',#42453,10.);
#12089=VECTOR('',#42460,10.);
#12090=VECTOR('',#42463,10.);
#12091=VECTOR('',#42464,10.);
#12092=VECTOR('',#42465,10.);
#12093=VECTOR('',#42472,10.);
#12094=VECTOR('',#42475,10.);
#12095=VECTOR('',#42476,10.);
#12096=VECTOR('',#42485,10.);
#12097=VECTOR('',#42488,10.);
#12098=VECTOR('',#42491,10.);
#12099=VECTOR('',#42492,10.);
#12100=VECTOR('',#42493,10.);
#12101=VECTOR('',#42498,10.);
#12102=VECTOR('',#42503,10.);
#12103=VECTOR('',#42504,10.);
#12104=VECTOR('',#42505,10.);
#12105=VECTOR('',#42510,10.);
#12106=VECTOR('',#42515,10.);
#12107=VECTOR('',#42516,10.);
#12108=VECTOR('',#42517,10.);
#12109=VECTOR('',#42522,10.);
#12110=VECTOR('',#42527,10.);
#12111=VECTOR('',#42528,10.);
#12112=VECTOR('',#42533,10.);
#12113=VECTOR('',#42536,10.);
#12114=VECTOR('',#42539,10.);
#12115=VECTOR('',#42540,10.);
#12116=VECTOR('',#42541,10.);
#12117=VECTOR('',#42548,10.);
#12118=VECTOR('',#42551,10.);
#12119=VECTOR('',#42552,10.);
#12120=VECTOR('',#42553,10.);
#12121=VECTOR('',#42560,10.);
#12122=VECTOR('',#42563,10.);
#12123=VECTOR('',#42564,10.);
#12124=VECTOR('',#42565,10.);
#12125=VECTOR('',#42572,10.);
#12126=VECTOR('',#42575,10.);
#12127=VECTOR('',#42576,10.);
#12128=VECTOR('',#42589,5.053);
#12129=VECTOR('',#42596,5.053);
#12130=VECTOR('',#42603,5.053);
#12131=VECTOR('',#42610,5.053);
#12132=VECTOR('',#42617,5.053);
#12133=VECTOR('',#42624,5.053);
#12134=VECTOR('',#42631,5.053);
#12135=VECTOR('',#42638,5.053);
#12136=VECTOR('',#42645,5.053);
#12137=VECTOR('',#42652,5.053);
#12138=VECTOR('',#42659,5.053);
#12139=VECTOR('',#42666,5.053);
#12140=VECTOR('',#42673,5.053);
#12141=VECTOR('',#42680,5.053);
#12142=VECTOR('',#42687,5.053);
#12143=VECTOR('',#42694,5.053);
#12144=VECTOR('',#42699,10.);
#12145=VECTOR('',#42700,10.);
#12146=VECTOR('',#42701,10.);
#12147=VECTOR('',#42702,10.);
#12148=VECTOR('',#42705,10.);
#12149=VECTOR('',#42706,10.);
#12150=VECTOR('',#42707,10.);
#12151=VECTOR('',#42710,10.);
#12152=VECTOR('',#42711,10.);
#12153=VECTOR('',#42712,10.);
#12154=VECTOR('',#42715,10.);
#12155=VECTOR('',#42716,10.);
#12156=VECTOR('',#42719,10.);
#12157=VECTOR('',#42720,10.);
#12158=VECTOR('',#42721,10.);
#12159=VECTOR('',#42722,10.);
#12160=VECTOR('',#42725,10.);
#12161=VECTOR('',#42726,10.);
#12162=VECTOR('',#42727,10.);
#12163=VECTOR('',#42730,10.);
#12164=VECTOR('',#42731,10.);
#12165=VECTOR('',#42734,10.);
#12166=VECTOR('',#42735,10.);
#12167=VECTOR('',#42738,10.);
#12168=VECTOR('',#42745,10.);
#12169=VECTOR('',#42746,10.);
#12170=VECTOR('',#42747,10.);
#12171=VECTOR('',#42748,10.);
#12172=VECTOR('',#42757,10.);
#12173=VECTOR('',#42758,10.);
#12174=VECTOR('',#42759,10.);
#12175=VECTOR('',#42760,10.);
#12176=VECTOR('',#42769,10.);
#12177=VECTOR('',#42770,10.);
#12178=VECTOR('',#42773,2.094);
#12179=VECTOR('',#42778,4.188);
#12180=VECTOR('',#42781,2.094);
#12181=VECTOR('',#42786,4.188);
#12182=VECTOR('',#42789,2.094);
#12183=VECTOR('',#42794,4.188);
#12184=VECTOR('',#42797,2.094);
#12185=VECTOR('',#42802,4.188);
#12186=VECTOR('',#42805,2.094);
#12187=VECTOR('',#42810,4.188);
#12188=VECTOR('',#42813,2.094);
#12189=VECTOR('',#42818,4.188);
#12190=VECTOR('',#42823,5.188);
#12191=VECTOR('',#42830,5.188);
#12192=VECTOR('',#42837,5.188);
#12193=VECTOR('',#42844,5.188);
#12194=VECTOR('',#42851,5.188);
#12195=VECTOR('',#42858,5.188);
#12196=VECTOR('',#42865,5.188);
#12197=VECTOR('',#42872,5.188);
#12198=VECTOR('',#42879,20.);
#12199=VECTOR('',#42886,20.);
#12200=VECTOR('',#42891,10.);
#12201=VECTOR('',#42894,10.);
#12202=VECTOR('',#42901,10.);
#12203=VECTOR('',#42902,10.);
#12204=VECTOR('',#42903,10.);
#12205=VECTOR('',#42904,10.);
#12206=VECTOR('',#42913,10.);
#12207=VECTOR('',#42914,10.);
#12208=VECTOR('',#42915,10.);
#12209=VECTOR('',#42916,10.);
#12210=VECTOR('',#42925,10.);
#12211=VECTOR('',#42926,10.);
#12212=VECTOR('',#42929,2.094);
#12213=VECTOR('',#42934,4.188);
#12214=VECTOR('',#42937,2.094);
#12215=VECTOR('',#42942,4.188);
#12216=VECTOR('',#42945,2.094);
#12217=VECTOR('',#42950,4.188);
#12218=VECTOR('',#42953,2.094);
#12219=VECTOR('',#42958,4.188);
#12220=VECTOR('',#42961,2.094);
#12221=VECTOR('',#42966,4.188);
#12222=VECTOR('',#42969,2.094);
#12223=VECTOR('',#42974,4.188);
#12224=VECTOR('',#42979,5.188);
#12225=VECTOR('',#42986,5.188);
#12226=VECTOR('',#42993,5.188);
#12227=VECTOR('',#43000,5.188);
#12228=VECTOR('',#43007,5.188);
#12229=VECTOR('',#43014,5.188);
#12230=VECTOR('',#43021,5.188);
#12231=VECTOR('',#43028,5.188);
#12232=VECTOR('',#43035,20.);
#12233=VECTOR('',#43042,20.);
#12234=VECTOR('',#43047,10.);
#12235=VECTOR('',#43050,10.);
#12236=VECTOR('',#43059,5.5);
#12237=VECTOR('',#43066,5.5);
#12238=VECTOR('',#43073,5.5);
#12239=VECTOR('',#43080,5.5);
#12240=VECTOR('',#43087,5.5);
#12241=VECTOR('',#43094,5.5);
#12242=VECTOR('',#43099,10.);
#12243=VECTOR('',#43100,10.);
#12244=VECTOR('',#43101,10.);
#12245=VECTOR('',#43102,10.);
#12246=VECTOR('',#43105,10.);
#12247=VECTOR('',#43106,10.);
#12248=VECTOR('',#43107,10.);
#12249=VECTOR('',#43110,10.);
#12250=VECTOR('',#43111,10.);
#12251=VECTOR('',#43112,10.);
#12252=VECTOR('',#43115,10.);
#12253=VECTOR('',#43116,10.);
#12254=VECTOR('',#43125,10.);
#12255=VECTOR('',#43126,10.);
#12256=VECTOR('',#43127,10.);
#12257=VECTOR('',#43128,10.);
#12258=VECTOR('',#43131,10.);
#12259=VECTOR('',#43132,10.);
#12260=VECTOR('',#43133,10.);
#12261=VECTOR('',#43136,10.);
#12262=VECTOR('',#43137,10.);
#12263=VECTOR('',#43138,10.);
#12264=VECTOR('',#43141,10.);
#12265=VECTOR('',#43142,10.);
#12266=VECTOR('',#43145,10.);
#12267=VECTOR('',#43146,10.);
#12268=VECTOR('',#43151,10.);
#12269=VECTOR('',#43152,10.);
#12270=VECTOR('',#43153,10.);
#12271=VECTOR('',#43154,10.);
#12272=VECTOR('',#43155,10.);
#12273=VECTOR('',#43158,10.);
#12274=VECTOR('',#43161,10.);
#12275=VECTOR('',#43164,10.);
#12276=VECTOR('',#43175,7.);
#12277=VECTOR('',#43182,7.);
#12278=VECTOR('',#43189,7.);
#12279=VECTOR('',#43196,7.);
#12280=VECTOR('',#43201,10.);
#12281=VECTOR('',#43202,10.);
#12282=VECTOR('',#43203,10.);
#12283=VECTOR('',#43204,10.);
#12284=VECTOR('',#43207,10.);
#12285=VECTOR('',#43208,10.);
#12286=VECTOR('',#43209,10.);
#12287=VECTOR('',#43212,10.);
#12288=VECTOR('',#43213,10.);
#12289=VECTOR('',#43214,10.);
#12290=VECTOR('',#43217,10.);
#12291=VECTOR('',#43218,10.);
#12292=VECTOR('',#43221,10.);
#12293=VECTOR('',#43222,10.);
#12294=VECTOR('',#43223,10.);
#12295=VECTOR('',#43224,10.);
#12296=VECTOR('',#43227,10.);
#12297=VECTOR('',#43228,10.);
#12298=VECTOR('',#43229,10.);
#12299=VECTOR('',#43232,10.);
#12300=VECTOR('',#43233,10.);
#12301=VECTOR('',#43234,10.);
#12302=VECTOR('',#43237,10.);
#12303=VECTOR('',#43238,10.);
#12304=VECTOR('',#43281,20.);
#12305=VECTOR('',#43284,10.);
#12306=VECTOR('',#43289,10.);
#12307=VECTOR('',#43292,10.);
#12308=VECTOR('',#43295,10.);
#12309=VECTOR('',#43296,10.);
#12310=VECTOR('',#43297,10.);
#12311=VECTOR('',#43300,10.);
#12312=VECTOR('',#43301,10.);
#12313=VECTOR('',#43302,10.);
#12314=VECTOR('',#43327,15.);
#12315=VECTOR('',#43344,15.);
#12316=VECTOR('',#43355,18.25);
#12317=VECTOR('',#43360,18.5);
#12318=VECTOR('',#43369,18.25);
#12319=VECTOR('',#43372,18.5);
#12320=VECTOR('',#43379,14.5);
#12321=VECTOR('',#43386,10.);
#12322=VECTOR('',#43389,10.);
#12323=VECTOR('',#43392,10.);
#12324=VECTOR('',#43393,10.);
#12325=VECTOR('',#43394,10.);
#12326=VECTOR('',#43397,10.);
#12327=VECTOR('',#43398,10.);
#12328=VECTOR('',#43413,14.5);
#12329=VECTOR('',#43430,19.75);
#12330=VECTOR('',#43433,19.75);
#12331=VECTOR('',#43448,20.);
#12332=VECTOR('',#43451,10.);
#12333=VECTOR('',#43460,12.25);
#12334=VECTOR('',#43465,12.5);
#12335=VECTOR('',#43468,10.);
#12336=VECTOR('',#43469,10.);
#12337=VECTOR('',#43478,14.75);
#12338=VECTOR('',#43483,15.);
#12339=VECTOR('',#43492,10.);
#12340=VECTOR('',#43493,10.);
#12341=VECTOR('',#43494,10.);
#12342=VECTOR('',#43499,10.);
#12343=VECTOR('',#43502,10.);
#12344=VECTOR('',#43503,10.);
#12345=VECTOR('',#43516,18.25);
#12346=VECTOR('',#43527,18.5);
#12347=VECTOR('',#43540,15.);
#12348=VECTOR('',#43561,18.25);
#12349=VECTOR('',#43564,18.5);
#12350=VECTOR('',#43571,14.5);
#12351=VECTOR('',#43578,10.);
#12352=VECTOR('',#43581,10.);
#12353=VECTOR('',#43584,10.);
#12354=VECTOR('',#43585,10.);
#12355=VECTOR('',#43586,10.);
#12356=VECTOR('',#43589,10.);
#12357=VECTOR('',#43590,10.);
#12358=VECTOR('',#43615,19.75);
#12359=VECTOR('',#43618,19.75);
#12360=VECTOR('',#43633,10.);
#12361=VECTOR('',#43634,10.);
#12362=VECTOR('',#43635,10.);
#12363=VECTOR('',#43636,10.);
#12364=VECTOR('',#43639,10.);
#12365=VECTOR('',#43640,10.);
#12366=VECTOR('',#43641,10.);
#12367=VECTOR('',#43644,10.);
#12368=VECTOR('',#43645,10.);
#12369=VECTOR('',#43646,10.);
#12370=VECTOR('',#43661,30.);
#12371=VECTOR('',#43670,18.5);
#12372=VECTOR('',#43677,33.);
#12373=VECTOR('',#43732,30.);
#12374=VECTOR('',#43737,10.);
#12375=VECTOR('',#43738,10.);
#12376=VECTOR('',#43739,10.);
#12377=VECTOR('',#44136,10.);
#12378=VECTOR('',#44137,10.);
#12379=VECTOR('',#44138,10.);
#12380=VECTOR('',#44141,10.);
#12381=VECTOR('',#44142,10.);
#12382=VECTOR('',#44147,10.);
#12383=VECTOR('',#44150,10.);
#12384=VECTOR('',#44153,10.);
#12385=VECTOR('',#44156,10.);
#12386=VECTOR('',#44161,10.);
#12387=VECTOR('',#44164,10.);
#12388=VECTOR('',#44169,10.);
#12389=VECTOR('',#44172,10.);
#12390=VECTOR('',#44177,10.);
#12391=VECTOR('',#44180,10.);
#12392=VECTOR('',#44185,10.);
#12393=VECTOR('',#44188,10.);
#12394=VECTOR('',#44193,10.);
#12395=VECTOR('',#44196,10.);
#12396=VECTOR('',#44201,10.);
#12397=VECTOR('',#44204,10.);
#12398=VECTOR('',#44209,10.);
#12399=VECTOR('',#44212,10.);
#12400=VECTOR('',#44217,10.);
#12401=VECTOR('',#44220,10.);
#12402=VECTOR('',#44225,10.);
#12403=VECTOR('',#44228,10.);
#12404=VECTOR('',#44233,10.);
#12405=VECTOR('',#44236,10.);
#12406=VECTOR('',#44241,10.);
#12407=VECTOR('',#44244,10.);
#12408=VECTOR('',#44249,10.);
#12409=VECTOR('',#44252,10.);
#12410=VECTOR('',#44257,10.);
#12411=VECTOR('',#44260,10.);
#12412=VECTOR('',#44265,10.);
#12413=VECTOR('',#44268,10.);
#12414=VECTOR('',#44273,10.);
#12415=VECTOR('',#44276,10.);
#12416=VECTOR('',#44281,10.);
#12417=VECTOR('',#44284,10.);
#12418=VECTOR('',#44289,10.);
#12419=VECTOR('',#44292,10.);
#12420=VECTOR('',#44297,10.);
#12421=VECTOR('',#44300,10.);
#12422=VECTOR('',#44305,10.);
#12423=VECTOR('',#44308,10.);
#12424=VECTOR('',#44313,10.);
#12425=VECTOR('',#44316,10.);
#12426=VECTOR('',#44321,10.);
#12427=VECTOR('',#44324,10.);
#12428=VECTOR('',#44329,10.);
#12429=VECTOR('',#44332,10.);
#12430=VECTOR('',#44337,10.);
#12431=VECTOR('',#44340,10.);
#12432=VECTOR('',#44345,10.);
#12433=VECTOR('',#44348,10.);
#12434=VECTOR('',#44353,10.);
#12435=VECTOR('',#44356,10.);
#12436=VECTOR('',#44361,10.);
#12437=VECTOR('',#44364,10.);
#12438=VECTOR('',#44369,10.);
#12439=VECTOR('',#44372,10.);
#12440=VECTOR('',#44377,10.);
#12441=VECTOR('',#44380,10.);
#12442=VECTOR('',#44385,10.);
#12443=VECTOR('',#44388,10.);
#12444=VECTOR('',#44393,10.);
#12445=VECTOR('',#44396,10.);
#12446=VECTOR('',#44401,10.);
#12447=VECTOR('',#44404,10.);
#12448=VECTOR('',#44409,10.);
#12449=VECTOR('',#44412,10.);
#12450=VECTOR('',#44417,10.);
#12451=VECTOR('',#44420,10.);
#12452=VECTOR('',#44425,10.);
#12453=VECTOR('',#44428,10.);
#12454=VECTOR('',#44433,10.);
#12455=VECTOR('',#44436,10.);
#12456=VECTOR('',#44441,10.);
#12457=VECTOR('',#44444,10.);
#12458=VECTOR('',#44449,10.);
#12459=VECTOR('',#44452,10.);
#12460=VECTOR('',#44457,10.);
#12461=VECTOR('',#44460,10.);
#12462=VECTOR('',#44465,10.);
#12463=VECTOR('',#44468,10.);
#12464=VECTOR('',#44473,10.);
#12465=VECTOR('',#44476,10.);
#12466=VECTOR('',#44481,10.);
#12467=VECTOR('',#44484,10.);
#12468=VECTOR('',#44489,10.);
#12469=VECTOR('',#44492,10.);
#12470=VECTOR('',#44497,10.);
#12471=VECTOR('',#44500,10.);
#12472=VECTOR('',#44505,10.);
#12473=VECTOR('',#44508,10.);
#12474=VECTOR('',#44513,10.);
#12475=VECTOR('',#44516,10.);
#12476=VECTOR('',#44521,10.);
#12477=VECTOR('',#44524,10.);
#12478=VECTOR('',#44529,10.);
#12479=VECTOR('',#44532,10.);
#12480=VECTOR('',#44537,10.);
#12481=VECTOR('',#44540,10.);
#12482=VECTOR('',#44545,10.);
#12483=VECTOR('',#44548,10.);
#12484=VECTOR('',#44553,10.);
#12485=VECTOR('',#44556,10.);
#12486=VECTOR('',#44561,10.);
#12487=VECTOR('',#44564,10.);
#12488=VECTOR('',#44569,10.);
#12489=VECTOR('',#44572,10.);
#12490=VECTOR('',#44577,10.);
#12491=VECTOR('',#44580,10.);
#12492=VECTOR('',#44585,10.);
#12493=VECTOR('',#44588,10.);
#12494=VECTOR('',#44593,10.);
#12495=VECTOR('',#44596,10.);
#12496=VECTOR('',#44601,10.);
#12497=VECTOR('',#44604,10.);
#12498=VECTOR('',#44609,10.);
#12499=VECTOR('',#44612,10.);
#12500=VECTOR('',#44617,10.);
#12501=VECTOR('',#44620,10.);
#12502=VECTOR('',#44625,10.);
#12503=VECTOR('',#44628,10.);
#12504=VECTOR('',#44633,10.);
#12505=VECTOR('',#44636,10.);
#12506=VECTOR('',#44641,10.);
#12507=VECTOR('',#44644,10.);
#12508=VECTOR('',#44649,10.);
#12509=VECTOR('',#44652,10.);
#12510=VECTOR('',#44657,10.);
#12511=VECTOR('',#44660,10.);
#12512=VECTOR('',#44665,10.);
#12513=VECTOR('',#44668,10.);
#12514=VECTOR('',#44673,10.);
#12515=VECTOR('',#44676,10.);
#12516=VECTOR('',#44681,10.);
#12517=VECTOR('',#44684,10.);
#12518=VECTOR('',#44689,10.);
#12519=VECTOR('',#44692,10.);
#12520=VECTOR('',#44697,10.);
#12521=VECTOR('',#44700,10.);
#12522=VECTOR('',#44705,10.);
#12523=VECTOR('',#44708,10.);
#12524=VECTOR('',#44713,10.);
#12525=VECTOR('',#44716,10.);
#12526=VECTOR('',#44721,10.);
#12527=VECTOR('',#44724,10.);
#12528=VECTOR('',#44729,10.);
#12529=VECTOR('',#44732,10.);
#12530=VECTOR('',#44737,10.);
#12531=VECTOR('',#44740,10.);
#12532=VECTOR('',#44745,10.);
#12533=VECTOR('',#44748,10.);
#12534=VECTOR('',#44753,10.);
#12535=VECTOR('',#44756,10.);
#12536=VECTOR('',#44761,10.);
#12537=VECTOR('',#44764,10.);
#12538=VECTOR('',#44769,10.);
#12539=VECTOR('',#44772,10.);
#12540=VECTOR('',#44777,10.);
#12541=VECTOR('',#44780,10.);
#12542=VECTOR('',#44785,10.);
#12543=VECTOR('',#44788,10.);
#12544=VECTOR('',#44793,10.);
#12545=VECTOR('',#44796,10.);
#12546=VECTOR('',#44801,10.);
#12547=VECTOR('',#44804,10.);
#12548=VECTOR('',#44809,10.);
#12549=VECTOR('',#44812,10.);
#12550=VECTOR('',#44817,10.);
#12551=VECTOR('',#44820,10.);
#12552=VECTOR('',#44825,10.);
#12553=VECTOR('',#44828,10.);
#12554=VECTOR('',#44833,10.);
#12555=VECTOR('',#44836,10.);
#12556=VECTOR('',#44841,10.);
#12557=VECTOR('',#44844,10.);
#12558=VECTOR('',#44849,10.);
#12559=VECTOR('',#44852,10.);
#12560=VECTOR('',#44857,10.);
#12561=VECTOR('',#44860,10.);
#12562=VECTOR('',#44865,10.);
#12563=VECTOR('',#44868,10.);
#12564=VECTOR('',#44873,10.);
#12565=VECTOR('',#44876,10.);
#12566=VECTOR('',#44881,10.);
#12567=VECTOR('',#44884,10.);
#12568=VECTOR('',#44889,10.);
#12569=VECTOR('',#44892,10.);
#12570=VECTOR('',#44897,10.);
#12571=VECTOR('',#44900,10.);
#12572=VECTOR('',#44907,10.);
#12573=VECTOR('',#45094,10.);
#12574=VECTOR('',#45097,10.);
#12575=VECTOR('',#45102,10.);
#12576=VECTOR('',#45127,30.);
#12577=VECTOR('',#45132,10.);
#12578=VECTOR('',#45133,10.);
#12579=VECTOR('',#45134,10.);
#12580=VECTOR('',#45467,10.);
#12581=VECTOR('',#45468,10.);
#12582=VECTOR('',#45469,10.);
#12583=VECTOR('',#45472,10.);
#12584=VECTOR('',#45473,10.);
#12585=VECTOR('',#45478,10.);
#12586=VECTOR('',#45481,10.);
#12587=VECTOR('',#45484,10.);
#12588=VECTOR('',#45487,10.);
#12589=VECTOR('',#45492,10.);
#12590=VECTOR('',#45495,10.);
#12591=VECTOR('',#45500,10.);
#12592=VECTOR('',#45503,10.);
#12593=VECTOR('',#45508,10.);
#12594=VECTOR('',#45511,10.);
#12595=VECTOR('',#45516,10.);
#12596=VECTOR('',#45519,10.);
#12597=VECTOR('',#45524,10.);
#12598=VECTOR('',#45527,10.);
#12599=VECTOR('',#45532,10.);
#12600=VECTOR('',#45535,10.);
#12601=VECTOR('',#45540,10.);
#12602=VECTOR('',#45543,10.);
#12603=VECTOR('',#45548,10.);
#12604=VECTOR('',#45551,10.);
#12605=VECTOR('',#45556,10.);
#12606=VECTOR('',#45559,10.);
#12607=VECTOR('',#45564,10.);
#12608=VECTOR('',#45567,10.);
#12609=VECTOR('',#45572,10.);
#12610=VECTOR('',#45575,10.);
#12611=VECTOR('',#45580,10.);
#12612=VECTOR('',#45583,10.);
#12613=VECTOR('',#45588,10.);
#12614=VECTOR('',#45591,10.);
#12615=VECTOR('',#45596,10.);
#12616=VECTOR('',#45599,10.);
#12617=VECTOR('',#45604,10.);
#12618=VECTOR('',#45607,10.);
#12619=VECTOR('',#45612,10.);
#12620=VECTOR('',#45615,10.);
#12621=VECTOR('',#45620,10.);
#12622=VECTOR('',#45623,10.);
#12623=VECTOR('',#45628,10.);
#12624=VECTOR('',#45631,10.);
#12625=VECTOR('',#45636,10.);
#12626=VECTOR('',#45639,10.);
#12627=VECTOR('',#45644,10.);
#12628=VECTOR('',#45647,10.);
#12629=VECTOR('',#45652,10.);
#12630=VECTOR('',#45655,10.);
#12631=VECTOR('',#45660,10.);
#12632=VECTOR('',#45663,10.);
#12633=VECTOR('',#45668,10.);
#12634=VECTOR('',#45671,10.);
#12635=VECTOR('',#45676,10.);
#12636=VECTOR('',#45679,10.);
#12637=VECTOR('',#45684,10.);
#12638=VECTOR('',#45687,10.);
#12639=VECTOR('',#45692,10.);
#12640=VECTOR('',#45695,10.);
#12641=VECTOR('',#45700,10.);
#12642=VECTOR('',#45703,10.);
#12643=VECTOR('',#45708,10.);
#12644=VECTOR('',#45711,10.);
#12645=VECTOR('',#45716,10.);
#12646=VECTOR('',#45719,10.);
#12647=VECTOR('',#45724,10.);
#12648=VECTOR('',#45727,10.);
#12649=VECTOR('',#45732,10.);
#12650=VECTOR('',#45735,10.);
#12651=VECTOR('',#45740,10.);
#12652=VECTOR('',#45743,10.);
#12653=VECTOR('',#45748,10.);
#12654=VECTOR('',#45751,10.);
#12655=VECTOR('',#45756,10.);
#12656=VECTOR('',#45759,10.);
#12657=VECTOR('',#45764,10.);
#12658=VECTOR('',#45767,10.);
#12659=VECTOR('',#45772,10.);
#12660=VECTOR('',#45775,10.);
#12661=VECTOR('',#45780,10.);
#12662=VECTOR('',#45783,10.);
#12663=VECTOR('',#45788,10.);
#12664=VECTOR('',#45791,10.);
#12665=VECTOR('',#45796,10.);
#12666=VECTOR('',#45799,10.);
#12667=VECTOR('',#45804,10.);
#12668=VECTOR('',#45807,10.);
#12669=VECTOR('',#45812,10.);
#12670=VECTOR('',#45815,10.);
#12671=VECTOR('',#45820,10.);
#12672=VECTOR('',#45823,10.);
#12673=VECTOR('',#45828,10.);
#12674=VECTOR('',#45831,10.);
#12675=VECTOR('',#45836,10.);
#12676=VECTOR('',#45839,10.);
#12677=VECTOR('',#45844,10.);
#12678=VECTOR('',#45847,10.);
#12679=VECTOR('',#45852,10.);
#12680=VECTOR('',#45855,10.);
#12681=VECTOR('',#45860,10.);
#12682=VECTOR('',#45863,10.);
#12683=VECTOR('',#45868,10.);
#12684=VECTOR('',#45871,10.);
#12685=VECTOR('',#45876,10.);
#12686=VECTOR('',#45879,10.);
#12687=VECTOR('',#45884,10.);
#12688=VECTOR('',#45887,10.);
#12689=VECTOR('',#45892,10.);
#12690=VECTOR('',#45895,10.);
#12691=VECTOR('',#45900,10.);
#12692=VECTOR('',#45903,10.);
#12693=VECTOR('',#45908,10.);
#12694=VECTOR('',#45911,10.);
#12695=VECTOR('',#45916,10.);
#12696=VECTOR('',#45919,10.);
#12697=VECTOR('',#45924,10.);
#12698=VECTOR('',#45927,10.);
#12699=VECTOR('',#45932,10.);
#12700=VECTOR('',#45935,10.);
#12701=VECTOR('',#45940,10.);
#12702=VECTOR('',#45943,10.);
#12703=VECTOR('',#45948,10.);
#12704=VECTOR('',#45951,10.);
#12705=VECTOR('',#45956,10.);
#12706=VECTOR('',#45959,10.);
#12707=VECTOR('',#45964,10.);
#12708=VECTOR('',#45967,10.);
#12709=VECTOR('',#45972,10.);
#12710=VECTOR('',#45975,10.);
#12711=VECTOR('',#45980,10.);
#12712=VECTOR('',#45983,10.);
#12713=VECTOR('',#45988,10.);
#12714=VECTOR('',#45991,10.);
#12715=VECTOR('',#45996,10.);
#12716=VECTOR('',#45999,10.);
#12717=VECTOR('',#46004,10.);
#12718=VECTOR('',#46007,10.);
#12719=VECTOR('',#46012,10.);
#12720=VECTOR('',#46015,10.);
#12721=VECTOR('',#46020,10.);
#12722=VECTOR('',#46023,10.);
#12723=VECTOR('',#46028,10.);
#12724=VECTOR('',#46031,10.);
#12725=VECTOR('',#46036,10.);
#12726=VECTOR('',#46039,10.);
#12727=VECTOR('',#46044,10.);
#12728=VECTOR('',#46047,10.);
#12729=VECTOR('',#46052,10.);
#12730=VECTOR('',#46055,10.);
#12731=VECTOR('',#46060,10.);
#12732=VECTOR('',#46063,10.);
#12733=VECTOR('',#46068,10.);
#12734=VECTOR('',#46071,10.);
#12735=VECTOR('',#46076,10.);
#12736=VECTOR('',#46079,10.);
#12737=VECTOR('',#46084,10.);
#12738=VECTOR('',#46087,10.);
#12739=VECTOR('',#46092,10.);
#12740=VECTOR('',#46095,10.);
#12741=VECTOR('',#46100,10.);
#12742=VECTOR('',#46103,10.);
#12743=VECTOR('',#46110,10.);
#12744=VECTOR('',#46265,10.);
#12745=VECTOR('',#46268,10.);
#12746=VECTOR('',#46273,10.);
#12747=VECTOR('',#46298,3.21359174399996);
#12748=VECTOR('',#46305,0.322047616000012);
#12749=VECTOR('',#46312,3.22047616000001);
#12750=VECTOR('',#46317,3.9116);
#12751=VECTOR('',#46330,4.19099999999999);
#12752=VECTOR('',#46337,3.21359174400012);
#12753=VECTOR('',#46344,0.322047616);
#12754=VECTOR('',#46351,3.22047616000001);
#12755=VECTOR('',#46356,3.91160000000001);
#12756=VECTOR('',#46369,4.19099999999999);
#12757=VECTOR('',#46374,2.74142809600001);
#12758=VECTOR('',#46387,2.74750784000002);
#12759=VECTOR('',#46390,0.274750783999988);
#12760=VECTOR('',#46395,3.3527999999999);
#12761=VECTOR('',#46406,3.6322);
#12762=VECTOR('',#46413,3.9116);
#12763=VECTOR('',#46422,4.191);
#12764=VECTOR('',#46433,3.21359174400008);
#12765=VECTOR('',#46444,3.22047616000001);
#12766=VECTOR('',#46447,0.322047616);
#12767=VECTOR('',#46452,3.91160000000001);
#12768=VECTOR('',#46461,4.19099999999999);
#12769=VECTOR('',#46472,3.21359174399998);
#12770=VECTOR('',#46483,3.22047616000001);
#12771=VECTOR('',#46486,0.322047616000012);
#12772=VECTOR('',#46489,10.);
#12773=VECTOR('',#46490,10.);
#12774=VECTOR('',#46491,10.);
#12775=VECTOR('',#46492,10.);
#12776=VECTOR('',#46493,10.);
#12777=VECTOR('',#46494,10.);
#12778=VECTOR('',#46495,10.);
#12779=VECTOR('',#46496,10.);
#12780=VECTOR('',#46497,10.);
#12781=VECTOR('',#46498,10.);
#12782=VECTOR('',#46499,10.);
#12783=VECTOR('',#46500,10.);
#12784=VECTOR('',#46501,10.);
#12785=VECTOR('',#46502,10.);
#12786=VECTOR('',#46507,10.);
#12787=VECTOR('',#46510,10.);
#12788=VECTOR('',#46513,10.);
#12789=VECTOR('',#46514,10.);
#12790=VECTOR('',#46515,10.);
#12791=VECTOR('',#46520,10.);
#12792=VECTOR('',#46523,10.);
#12793=VECTOR('',#46526,10.);
#12794=VECTOR('',#46527,10.);
#12795=VECTOR('',#46528,10.);
#12796=VECTOR('',#46529,10.);
#12797=VECTOR('',#46530,10.);
#12798=VECTOR('',#46533,9.99999999999999);
#12799=VECTOR('',#46534,10.);
#12800=VECTOR('',#46535,10.);
#12801=VECTOR('',#46536,10.);
#12802=VECTOR('',#46539,10.);
#12803=VECTOR('',#46540,10.);
#12804=VECTOR('',#46541,10.);
#12805=VECTOR('',#46546,10.);
#12806=VECTOR('',#46549,10.);
#12807=VECTOR('',#46550,10.);
#12808=VECTOR('',#46551,10.);
#12809=VECTOR('',#46552,10.);
#12810=VECTOR('',#46555,10.);
#12811=VECTOR('',#46556,10.);
#12812=VECTOR('',#46561,10.);
#12813=VECTOR('',#46562,10.);
#12814=VECTOR('',#46563,10.);
#12815=VECTOR('',#46568,10.);
#12816=VECTOR('',#46569,10.);
#12817=VECTOR('',#46570,10.);
#12818=VECTOR('',#46579,4.70822528);
#12819=VECTOR('',#46588,10.);
#12820=VECTOR('',#46591,10.);
#12821=VECTOR('',#46592,10.);
#12822=VECTOR('',#46593,10.);
#12823=VECTOR('',#46594,10.);
#12824=VECTOR('',#46595,10.);
#12825=VECTOR('',#46596,10.);
#12826=VECTOR('',#46605,4.70822528000001);
#12827=VECTOR('',#46612,10.);
#12828=VECTOR('',#46617,10.);
#12829=VECTOR('',#46618,10.);
#12830=VECTOR('',#46621,10.);
#12831=VECTOR('',#46624,10.);
#12832=VECTOR('',#46625,10.);
#12833=VECTOR('',#46626,10.);
#12834=VECTOR('',#46627,10.);
#12835=VECTOR('',#46628,10.);
#12836=VECTOR('',#46631,4.70822528000003);
#12837=VECTOR('',#46638,10.);
#12838=VECTOR('',#46639,10.);
#12839=VECTOR('',#46642,10.);
#12840=VECTOR('',#46643,10.);
#12841=VECTOR('',#46646,4.70822527999992);
#12842=VECTOR('',#46653,10.);
#12843=VECTOR('',#46654,10.);
#12844=VECTOR('',#46655,10.);
#12845=VECTOR('',#46656,10.);
#12846=VECTOR('',#46663,10.);
#12847=VECTOR('',#46666,10.);
#12848=VECTOR('',#46667,10.);
#12849=VECTOR('',#46668,10.);
#12850=VECTOR('',#46669,10.);
#12851=VECTOR('',#46670,10.);
#12852=VECTOR('',#46671,10.);
#12853=VECTOR('',#46672,10.);
#12854=VECTOR('',#46673,10.);
#12855=VECTOR('',#46674,10.);
#12856=VECTOR('',#46679,28.8698432);
#12857=VECTOR('',#46686,10.);
#12858=VECTOR('',#46691,10.);
#12859=VECTOR('',#46696,28.8519616);
#12860=VECTOR('',#46701,10.);
#12861=VECTOR('',#46706,10.);
#12862=VECTOR('',#46709,10.);
#12863=VECTOR('',#46710,10.);
#12864=VECTOR('',#46713,10.);
#12865=VECTOR('',#46716,10.);
#12866=VECTOR('',#46717,10.);
#12867=VECTOR('',#46718,10.);
#12868=VECTOR('',#46719,10.);
#12869=VECTOR('',#46722,10.);
#12870=VECTOR('',#46723,10.);
#12871=VECTOR('',#46724,10.);
#12872=VECTOR('',#46727,10.);
#12873=VECTOR('',#46728,10.);
#12874=VECTOR('',#46729,10.);
#12875=VECTOR('',#46732,10.);
#12876=VECTOR('',#46739,10.);
#12877=VECTOR('',#46748,4.70822528000001);
#12878=VECTOR('',#46757,4.70822528);
#12879=VECTOR('',#46766,4.70822528000001);
#12880=VECTOR('',#46775,4.70822528000002);
#12881=VECTOR('',#46782,10.);
#12882=VECTOR('',#46783,10.);
#12883=VECTOR('',#46784,10.);
#12884=VECTOR('',#46785,10.);
#12885=VECTOR('',#46786,10.);
#12886=VECTOR('',#46789,10.);
#12887=VECTOR('',#46790,10.);
#12888=VECTOR('',#46791,10.);
#12889=VECTOR('',#46792,10.);
#12890=VECTOR('',#46795,10.);
#12891=VECTOR('',#46800,10.);
#12892=VECTOR('',#46801,10.);
#12893=VECTOR('',#46802,10.);
#12894=VECTOR('',#46805,10.);
#12895=VECTOR('',#46806,10.);
#12896=VECTOR('',#46809,10.);
#12897=VECTOR('',#46814,22.5);
#12898=VECTOR('',#46821,10.);
#12899=VECTOR('',#46822,10.);
#12900=VECTOR('',#46823,10.);
#12901=VECTOR('',#46824,10.);
#12902=VECTOR('',#46827,10.);
#12903=VECTOR('',#46828,10.);
#12904=VECTOR('',#46829,10.);
#12905=VECTOR('',#46832,10.);
#12906=VECTOR('',#46833,10.);
#12907=VECTOR('',#46834,10.);
#12908=VECTOR('',#46837,10.);
#12909=VECTOR('',#46838,10.);
#12910=VECTOR('',#46839,10.);
#12911=VECTOR('',#46862,10.);
#12912=VECTOR('',#46863,10.);
#12913=VECTOR('',#46864,10.);
#12914=VECTOR('',#46867,10.);
#12915=VECTOR('',#46868,10.);
#12916=VECTOR('',#46877,10.);
#12917=VECTOR('',#46878,10.);
#12918=VECTOR('',#46879,10.);
#12919=VECTOR('',#46880,10.);
#12920=VECTOR('',#46883,10.);
#12921=VECTOR('',#46884,10.);
#12922=VECTOR('',#46885,10.);
#12923=VECTOR('',#46888,10.);
#12924=VECTOR('',#46889,10.);
#12925=VECTOR('',#46890,10.);
#12926=VECTOR('',#46893,10.);
#12927=VECTOR('',#46894,10.);
#12928=VECTOR('',#46895,10.);
#12929=VECTOR('',#46918,10.);
#12930=VECTOR('',#46919,10.);
#12931=VECTOR('',#46920,10.);
#12932=VECTOR('',#46923,10.);
#12933=VECTOR('',#46924,10.);
#12934=VECTOR('',#46933,10.);
#12935=VECTOR('',#46934,10.);
#12936=VECTOR('',#46937,10.);
#12937=VECTOR('',#46938,10.);
#12938=VECTOR('',#46939,10.);
#12939=VECTOR('',#46942,10.);
#12940=VECTOR('',#46943,10.);
#12941=VECTOR('',#46946,10.);
#12942=VECTOR('',#46947,10.);
#12943=VECTOR('',#46950,10.);
#12944=VECTOR('',#46951,10.);
#12945=VECTOR('',#46954,10.);
#12946=VECTOR('',#46955,10.);
#12947=VECTOR('',#46958,10.);
#12948=VECTOR('',#46963,10.);
#12949=VECTOR('',#46966,10.);
#12950=VECTOR('',#46981,10.);
#12951=VECTOR('',#46982,10.);
#12952=VECTOR('',#46983,10.);
#12953=VECTOR('',#46984,10.);
#12954=VECTOR('',#46985,10.);
#12955=VECTOR('',#46986,10.);
#12956=VECTOR('',#46989,10.);
#12957=VECTOR('',#46990,10.);
#12958=VECTOR('',#46991,10.);
#12959=VECTOR('',#46994,10.);
#12960=VECTOR('',#46995,10.);
#12961=VECTOR('',#46998,10.);
#12962=VECTOR('',#46999,10.);
#12963=VECTOR('',#47002,10.);
#12964=VECTOR('',#47003,10.);
#12965=VECTOR('',#47006,10.);
#12966=VECTOR('',#47007,10.);
#12967=VECTOR('',#47010,10.);
#12968=VECTOR('',#47019,10.);
#12969=VECTOR('',#47020,10.);
#12970=VECTOR('',#47021,10.);
#12971=VECTOR('',#47022,10.);
#12972=VECTOR('',#47023,10.);
#12973=VECTOR('',#47024,9.99999999999999);
#12974=VECTOR('',#47027,9.99999999999999);
#12975=VECTOR('',#47028,10.);
#12976=VECTOR('',#47029,10.);
#12977=VECTOR('',#47032,10.);
#12978=VECTOR('',#47033,10.);
#12979=VECTOR('',#47036,10.);
#12980=VECTOR('',#47037,10.);
#12981=VECTOR('',#47040,10.);
#12982=VECTOR('',#47041,10.);
#12983=VECTOR('',#47044,10.);
#12984=VECTOR('',#47045,10.);
#12985=VECTOR('',#47048,10.);
#12986=VECTOR('',#47057,10.);
#12987=VECTOR('',#47058,10.);
#12988=VECTOR('',#47061,10.);
#12989=VECTOR('',#47062,10.);
#12990=VECTOR('',#47065,10.);
#12991=VECTOR('',#47072,5.83240278777977);
#12992=VECTOR('',#47075,0.274750783999998);
#12993=VECTOR('',#47082,2.74750784);
#12994=VECTOR('',#47089,2.80803705600002);
#12995=VECTOR('',#47094,0.274750783999993);
#12996=VECTOR('',#47101,2.74750784000001);
#12997=VECTOR('',#47108,2.808037056);
#12998=VECTOR('',#47113,0.274750783999995);
#12999=VECTOR('',#47120,2.74750784);
#13000=VECTOR('',#47127,2.80803705600003);
#13001=VECTOR('',#47136,3.28958854399998);
#13002=VECTOR('',#47141,3.2204761600001);
#13003=VECTOR('',#47148,0.322047616000123);
#13004=VECTOR('',#47155,3.2895885439999);
#13005=VECTOR('',#47160,3.22047616000001);
#13006=VECTOR('',#47167,0.322047615999997);
#13007=VECTOR('',#47174,3.289588544);
#13008=VECTOR('',#47179,3.22047616000007);
#13009=VECTOR('',#47186,0.322047616000094);
#13010=VECTOR('',#47193,3.2895885439999);
#13011=VECTOR('',#47198,3.22047616000001);
#13012=VECTOR('',#47205,0.32204761600005);
#13013=VECTOR('',#47208,0.470822528000023);
#13014=VECTOR('',#47211,0.470822528000024);
#13015=VECTOR('',#47214,0.470822528000001);
#13016=VECTOR('',#47217,0.470822528000002);
#13017=VECTOR('',#47220,0.47082252800002);
#13018=VECTOR('',#47223,0.470822528000018);
#13019=VECTOR('',#47226,0.470822528000013);
#13020=VECTOR('',#47229,0.470822528000016);
#13021=VECTOR('',#47232,10.);
#13022=VECTOR('',#47233,10.);
#13023=VECTOR('',#47234,10.);
#13024=VECTOR('',#47237,10.);
#13025=VECTOR('',#47238,10.);
#13026=VECTOR('',#47241,10.);
#13027=VECTOR('',#47242,10.);
#13028=VECTOR('',#47243,10.);
#13029=VECTOR('',#47246,10.);
#13030=VECTOR('',#47247,10.);
#13031=VECTOR('',#47250,10.);
#13032=VECTOR('',#47251,10.);
#13033=VECTOR('',#47254,10.);
#13034=VECTOR('',#47255,10.);
#13035=VECTOR('',#47258,10.);
#13036=VECTOR('',#47259,10.);
#13037=VECTOR('',#47262,10.);
#13038=VECTOR('',#47265,10.);
#13039=VECTOR('',#47266,10.);
#13040=VECTOR('',#47267,10.);
#13041=VECTOR('',#47268,10.);
#13042=VECTOR('',#47269,10.);
#13043=VECTOR('',#47270,10.);
#13044=VECTOR('',#47271,10.);
#13045=VECTOR('',#47272,10.);
#13046=VECTOR('',#47273,10.);
#13047=VECTOR('',#47274,10.);
#13048=VECTOR('',#47283,46.9481408);
#13049=VECTOR('',#47290,46.9997605328678);
#13050=VECTOR('',#47299,10.);
#13051=VECTOR('',#47302,10.);
#13052=VECTOR('',#47303,10.);
#13053=VECTOR('',#47306,10.);
#13054=VECTOR('',#47307,10.);
#13055=VECTOR('',#47310,10.);
#13056=VECTOR('',#47311,10.);
#13057=VECTOR('',#47314,10.);
#13058=VECTOR('',#47315,10.);
#13059=VECTOR('',#47318,10.);
#13060=VECTOR('',#47319,10.);
#13061=VECTOR('',#47322,10.);
#13062=VECTOR('',#47327,10.);
#13063=VECTOR('',#47338,67.117943679437);
#13064=VECTOR('',#47343,30.1930816);
#13065=VECTOR('',#47346,28.921462932868);
#13066=VECTOR('',#47351,67.056);
#13067=VECTOR('',#47352,67.056);
#13068=VECTOR('',#47361,46.9481408);
#13069=VECTOR('',#47370,46.9997605328686);
#13070=VECTOR('',#47375,10.);
#13071=VECTOR('',#47376,10.);
#13072=VECTOR('',#47377,10.);
#13073=VECTOR('',#47378,10.);
#13074=VECTOR('',#47379,10.);
#13075=VECTOR('',#47380,10.);
#13076=VECTOR('',#47381,10.);
#13077=VECTOR('',#47382,10.);
#13078=VECTOR('',#47383,10.);
#13079=VECTOR('',#47384,10.);
#13080=VECTOR('',#47385,10.);
#13081=VECTOR('',#47386,10.);
#13082=VECTOR('',#47395,67.0291776);
#13083=VECTOR('',#47404,2.74750783999999);
#13084=VECTOR('',#47413,37.927515520559);
#13085=VECTOR('',#47418,10.);
#13086=VECTOR('',#47419,10.);
#13087=VECTOR('',#47422,10.);
#13088=VECTOR('',#47433,10.);
#13089=VECTOR('',#47436,10.);
#13090=VECTOR('',#47443,2.74750784);
#13091=VECTOR('',#47448,10.);
#13092=VECTOR('',#47449,10.);
#13093=VECTOR('',#47452,10.);
#13094=VECTOR('',#47453,10.);
#13095=VECTOR('',#47454,10.);
#13096=VECTOR('',#47455,10.);
#13097=VECTOR('',#47456,10.);
#13098=VECTOR('',#47457,10.);
#13099=VECTOR('',#47460,10.);
#13100=VECTOR('',#47461,10.);
#13101=VECTOR('',#47462,10.);
#13102=VECTOR('',#47465,10.);
#13103=VECTOR('',#47466,10.);
#13104=VECTOR('',#47469,10.);
#13105=VECTOR('',#47470,10.);
#13106=VECTOR('',#47473,10.);
#13107=VECTOR('',#47474,10.);
#13108=VECTOR('',#47477,10.);
#13109=VECTOR('',#47478,10.);
#13110=VECTOR('',#47481,10.);
#13111=VECTOR('',#47484,10.);
#13112=VECTOR('',#47485,10.);
#13113=VECTOR('',#47486,10.);
#13114=VECTOR('',#47487,10.);
#13115=VECTOR('',#47488,10.);
#13116=VECTOR('',#47489,10.);
#13117=VECTOR('',#47492,10.);
#13118=VECTOR('',#47493,10.);
#13119=VECTOR('',#47494,10.);
#13120=VECTOR('',#47497,10.);
#13121=VECTOR('',#47498,10.);
#13122=VECTOR('',#47501,10.);
#13123=VECTOR('',#47502,10.);
#13124=VECTOR('',#47505,10.);
#13125=VECTOR('',#47506,10.);
#13126=VECTOR('',#47509,10.);
#13127=VECTOR('',#47510,10.);
#13128=VECTOR('',#47513,10.);
#13129=VECTOR('',#47524,3.2861910399999);
#13130=VECTOR('',#47527,3.3528);
#13131=VECTOR('',#47534,2.74142809599801);
#13132=VECTOR('',#47549,3.28619103999997);
#13133=VECTOR('',#47552,10.);
#13134=VECTOR('',#47553,10.);
#13135=VECTOR('',#47554,10.);
#13136=VECTOR('',#47555,10.);
#13137=VECTOR('',#47556,10.);
#13138=VECTOR('',#47557,10.);
#13139=VECTOR('',#47560,10.);
#13140=VECTOR('',#47561,10.);
#13141=VECTOR('',#47562,10.);
#13142=VECTOR('',#47565,10.);
#13143=VECTOR('',#47566,10.);
#13144=VECTOR('',#47569,10.);
#13145=VECTOR('',#47570,10.);
#13146=VECTOR('',#47573,10.);
#13147=VECTOR('',#47574,10.);
#13148=VECTOR('',#47577,10.);
#13149=VECTOR('',#47578,10.);
#13150=VECTOR('',#47581,10.);
#13151=VECTOR('',#47584,10.);
#13152=VECTOR('',#47585,10.);
#13153=VECTOR('',#47586,10.);
#13154=VECTOR('',#47587,10.);
#13155=VECTOR('',#47588,10.);
#13156=VECTOR('',#47589,9.99999999999999);
#13157=VECTOR('',#47592,10.);
#13158=VECTOR('',#47593,10.);
#13159=VECTOR('',#47594,10.);
#13160=VECTOR('',#47597,10.);
#13161=VECTOR('',#47598,10.);
#13162=VECTOR('',#47601,10.);
#13163=VECTOR('',#47602,10.);
#13164=VECTOR('',#47605,10.);
#13165=VECTOR('',#47606,10.);
#13166=VECTOR('',#47609,10.);
#13167=VECTOR('',#47610,10.);
#13168=VECTOR('',#47613,10.);
#13169=VECTOR('',#47624,3.28619104000002);
#13170=VECTOR('',#47627,3.35280000000001);
#13171=VECTOR('',#47634,2.74142809600037);
#13172=VECTOR('',#47649,3.28619104000001);
#13173=VECTOR('',#47652,3.3528);
#13174=VECTOR('',#47655,2.74142809599998);
#13175=VECTOR('',#47662,2.74750783999998);
#13176=VECTOR('',#47665,2.74750784000003);
#13177=VECTOR('',#47672,2.74142809599988);
#13178=VECTOR('',#47675,3.3528);
#13179=VECTOR('',#47682,37.9894592000001);
#13180=VECTOR('',#47687,37.0614901167744);
#13181=VECTOR('',#47698,37.9894592000001);
#13182=VECTOR('',#47709,46.9481408);
#13183=VECTOR('',#47712,37.9894592000001);
#13184=VECTOR('',#47723,46.9481408);
#13185=VECTOR('',#47728,10.);
#13186=VECTOR('',#47731,10.);
#13187=VECTOR('',#47734,10.);
#13188=VECTOR('',#47737,10.);
#13189=VECTOR('',#47740,10.);
#13190=VECTOR('',#47743,10.);
#13191=VECTOR('',#47748,10.);
#13192=VECTOR('',#47749,10.);
#13193=VECTOR('',#47752,10.);
#13194=VECTOR('',#47765,10.);
#13195=VECTOR('',#47768,10.);
#13196=VECTOR('',#47771,10.);
#13197=VECTOR('',#47778,10.);
#13198=VECTOR('',#47781,10.);
#13199=VECTOR('',#47784,10.);
#13200=VECTOR('',#47787,10.);
#13201=VECTOR('',#47790,10.);
#13202=VECTOR('',#47793,10.);
#13203=VECTOR('',#47798,10.);
#13204=VECTOR('',#47799,10.);
#13205=VECTOR('',#47802,10.);
#13206=VECTOR('',#47815,10.);
#13207=VECTOR('',#47818,10.);
#13208=VECTOR('',#47821,10.);
#13209=VECTOR('',#47840,2.74750784);
#13210=VECTOR('',#47847,2.74750784000001);
#13211=VECTOR('',#47854,21.82583392);
#13212=VECTOR('',#47859,3.63219999999997);
#13213=VECTOR('',#47866,3.63219999999997);
#13214=VECTOR('',#47873,3.63219999999999);
#13215=VECTOR('',#47880,3.63219999999999);
#13216=VECTOR('',#47889,9.99999999999999);
#13217=VECTOR('',#47896,10.);
#13218=VECTOR('',#47901,10.);
#13219=VECTOR('',#47902,10.);
#13220=VECTOR('',#47903,10.);
#13221=VECTOR('',#47904,10.);
#13222=VECTOR('',#47909,10.);
#13223=VECTOR('',#47916,10.);
#13224=VECTOR('',#47923,10.);
#13225=VECTOR('',#47928,10.);
#13226=VECTOR('',#47929,10.);
#13227=VECTOR('',#47930,10.);
#13228=VECTOR('',#47935,10.);
#13229=VECTOR('',#47942,10.);
#13230=VECTOR('',#47955,10.);
#13231=VECTOR('',#47956,10.);
#13232=VECTOR('',#47957,10.);
#13233=VECTOR('',#47958,10.);
#13234=VECTOR('',#47963,10.);
#13235=VECTOR('',#47970,10.);
#13236=VECTOR('',#47977,10.);
#13237=VECTOR('',#47982,10.);
#13238=VECTOR('',#47983,10.);
#13239=VECTOR('',#47984,10.);
#13240=VECTOR('',#47989,10.);
#13241=VECTOR('',#47996,10.);
#13242=VECTOR('',#48009,10.);
#13243=VECTOR('',#48010,10.);
#13244=VECTOR('',#48011,10.);
#13245=VECTOR('',#48012,10.);
#13246=VECTOR('',#48017,10.);
#13247=VECTOR('',#48024,10.);
#13248=VECTOR('',#48031,10.);
#13249=VECTOR('',#48036,10.);
#13250=VECTOR('',#48037,10.);
#13251=VECTOR('',#48038,10.);
#13252=VECTOR('',#48043,10.);
#13253=VECTOR('',#48050,10.);
#13254=VECTOR('',#48063,3.63219999999999);
#13255=VECTOR('',#48068,3.63220000000001);
#13256=VECTOR('',#48073,3.63220000000001);
#13257=VECTOR('',#48088,10.);
#13258=VECTOR('',#48101,10.);
#13259=VECTOR('',#48114,10.);
#13260=VECTOR('',#48117,10.);
#13261=VECTOR('',#48118,10.);
#13262=VECTOR('',#48121,10.);
#13263=VECTOR('',#48122,10.);
#13264=VECTOR('',#48127,10.);
#13265=VECTOR('',#48130,10.);
#13266=VECTOR('',#48131,10.);
#13267=VECTOR('',#48134,10.);
#13268=VECTOR('',#48137,10.);
#13269=VECTOR('',#48140,10.);
#13270=VECTOR('',#48141,10.);
#13271=VECTOR('',#48144,10.);
#13272=VECTOR('',#48151,58.1057817920919);
#13273=VECTOR('',#48158,10.);
#13274=VECTOR('',#48159,10.);
#13275=VECTOR('',#48160,10.);
#13276=VECTOR('',#48163,10.);
#13277=VECTOR('',#48164,10.);
#13278=VECTOR('',#48165,10.);
#13279=VECTOR('',#48168,10.);
#13280=VECTOR('',#48169,10.);
#13281=VECTOR('',#48170,10.);
#13282=VECTOR('',#48173,10.);
#13283=VECTOR('',#48174,10.);
#13284=VECTOR('',#48175,10.);
#13285=VECTOR('',#48178,10.);
#13286=VECTOR('',#48179,10.);
#13287=VECTOR('',#48180,10.);
#13288=VECTOR('',#48181,10.);
#13289=VECTOR('',#48182,10.);
#13290=VECTOR('',#48183,10.);
#13291=VECTOR('',#48184,10.);
#13292=VECTOR('',#48187,10.);
#13293=VECTOR('',#48192,10.);
#13294=VECTOR('',#48193,10.);
#13295=VECTOR('',#48194,10.);
#13296=VECTOR('',#48195,10.);
#13297=VECTOR('',#48196,10.);
#13298=VECTOR('',#48197,10.);
#13299=VECTOR('',#48200,10.);
#13300=VECTOR('',#48205,10.);
#13301=VECTOR('',#48206,10.);
#13302=VECTOR('',#48207,10.);
#13303=VECTOR('',#48208,10.);
#13304=VECTOR('',#48209,10.);
#13305=VECTOR('',#48210,10.);
#13306=VECTOR('',#48211,10.);
#13307=VECTOR('',#48216,10.);
#13308=VECTOR('',#48221,10.);
#13309=VECTOR('',#48224,10.);
#13310=VECTOR('',#48227,10.);
#13311=VECTOR('',#48228,10.);
#13312=VECTOR('',#48229,10.);
#13313=VECTOR('',#48230,10.);
#13314=VECTOR('',#48231,10.);
#13315=VECTOR('',#48232,10.);
#13316=VECTOR('',#48239,10.);
#13317=VECTOR('',#48240,10.);
#13318=VECTOR('',#48243,10.);
#13319=VECTOR('',#48244,10.);
#13320=VECTOR('',#48247,10.);
#13321=VECTOR('',#48248,10.);
#13322=VECTOR('',#48251,10.);
#13323=VECTOR('',#48252,10.);
#13324=VECTOR('',#48257,10.);
#13325=VECTOR('',#48258,10.);
#13326=VECTOR('',#48263,10.);
#13327=VECTOR('',#48266,10.);
#13328=VECTOR('',#48269,10.);
#13329=VECTOR('',#48272,10.);
#13330=VECTOR('',#48277,10.);
#13331=VECTOR('',#48280,10.);
#13332=VECTOR('',#48285,10.);
#13333=VECTOR('',#48288,10.);
#13334=VECTOR('',#48305,10.);
#13335=VECTOR('',#48308,10.);
#13336=VECTOR('',#48311,10.);
#13337=VECTOR('',#48312,10.);
#13338=VECTOR('',#48313,10.);
#13339=VECTOR('',#48318,10.);
#13340=VECTOR('',#48325,10.);
#13341=VECTOR('',#48332,10.);
#13342=VECTOR('',#48337,10.);
#13343=VECTOR('',#48338,10.);
#13344=VECTOR('',#48339,10.);
#13345=VECTOR('',#48344,10.);
#13346=VECTOR('',#48357,10.);
#13347=VECTOR('',#48358,10.);
#13348=VECTOR('',#48359,10.);
#13349=VECTOR('',#48360,10.);
#13350=VECTOR('',#48365,10.);
#13351=VECTOR('',#48372,10.);
#13352=VECTOR('',#48379,10.);
#13353=VECTOR('',#48384,10.);
#13354=VECTOR('',#48385,10.);
#13355=VECTOR('',#48386,10.);
#13356=VECTOR('',#48391,10.);
#13357=VECTOR('',#48398,10.);
#13358=VECTOR('',#48413,10.);
#13359=VECTOR('',#48416,10.);
#13360=VECTOR('',#48421,10.);
#13361=VECTOR('',#48426,10.);
#13362=VECTOR('',#48427,10.);
#13363=VECTOR('',#48428,10.);
#13364=VECTOR('',#48433,10.);
#13365=VECTOR('',#48440,10.);
#13366=VECTOR('',#48447,10.);
#13367=VECTOR('',#48452,10.);
#13368=VECTOR('',#48453,10.);
#13369=VECTOR('',#48454,10.);
#13370=VECTOR('',#48467,10.);
#13371=VECTOR('',#48470,10.);
#13372=VECTOR('',#48475,10.);
#13373=VECTOR('',#48480,10.);
#13374=VECTOR('',#48481,10.);
#13375=VECTOR('',#48482,10.);
#13376=VECTOR('',#48487,10.);
#13377=VECTOR('',#48494,10.);
#13378=VECTOR('',#48501,10.);
#13379=VECTOR('',#48506,10.);
#13380=VECTOR('',#48507,10.);
#13381=VECTOR('',#48508,10.);
#13382=VECTOR('',#48521,10.);
#13383=VECTOR('',#48522,10.);
#13384=VECTOR('',#48527,10.);
#13385=VECTOR('',#48530,10.);
#13386=VECTOR('',#48531,10.);
#13387=VECTOR('',#48536,10.);
#13388=VECTOR('',#48541,10.);
#13389=VECTOR('',#48546,10.);
#13390=VECTOR('',#48551,10.);
#13391=VECTOR('',#48554,9.99999999999999);
#13392=VECTOR('',#48563,10.);
#13393=VECTOR('',#48564,10.);
#13394=VECTOR('',#48565,10.);
#13395=VECTOR('',#48566,10.);
#13396=VECTOR('',#48567,10.);
#13397=VECTOR('',#48568,10.);
#13398=VECTOR('',#48569,10.);
#13399=VECTOR('',#48570,10.);
#13400=VECTOR('',#48573,10.);
#13401=VECTOR('',#48574,10.);
#13402=VECTOR('',#48577,9.99999999999999);
#13403=VECTOR('',#48578,10.);
#13404=VECTOR('',#48583,10.);
#13405=VECTOR('',#48584,10.);
#13406=VECTOR('',#48587,10.);
#13407=VECTOR('',#48592,10.);
#13408=VECTOR('',#48605,4.98002560000028);
#13409=VECTOR('',#48610,5.02472959999993);
#13410=VECTOR('',#48617,5.01355360000019);
#13411=VECTOR('',#48620,10.);
#13412=VECTOR('',#48621,10.);
#13413=VECTOR('',#48622,10.);
#13414=VECTOR('',#48623,10.);
#13415=VECTOR('',#48626,10.);
#13416=VECTOR('',#48627,10.);
#13417=VECTOR('',#48628,10.);
#13418=VECTOR('',#48631,10.);
#13419=VECTOR('',#48632,10.);
#13420=VECTOR('',#48633,10.);
#13421=VECTOR('',#48636,10.);
#13422=VECTOR('',#48637,10.);
#13423=VECTOR('',#48638,10.);
#13424=VECTOR('',#48641,10.);
#13425=VECTOR('',#48642,10.);
#13426=VECTOR('',#48643,10.);
#13427=VECTOR('',#48646,10.);
#13428=VECTOR('',#48649,10.);
#13429=VECTOR('',#48658,12.);
#13430=VECTOR('',#48663,4.26299999999998);
#13431=VECTOR('',#48666,4.26299999999993);
#13432=VECTOR('',#48669,3.38975000000002);
#13433=VECTOR('',#48672,3.38974999999999);
#13434=VECTOR('',#48679,22.5);
#13435=VECTOR('',#48688,24.9999999999999);
#13436=VECTOR('',#48695,20.4999999999999);
#13437=VECTOR('',#48706,30.4999999999998);
#13438=VECTOR('',#48711,35.0000000000001);
#13439=VECTOR('',#48720,26.0000000000003);
#13440=VERTEX_POINT('',#48840);
#13441=VERTEX_POINT('',#48841);
#13442=VERTEX_POINT('',#48843);
#13443=VERTEX_POINT('',#48845);
#13444=VERTEX_POINT('',#48849);
#13445=VERTEX_POINT('',#48850);
#13446=VERTEX_POINT('',#48852);
#13447=VERTEX_POINT('',#48854);
#13448=VERTEX_POINT('',#48861);
#13449=VERTEX_POINT('',#48862);
#13450=VERTEX_POINT('',#48864);
#13451=VERTEX_POINT('',#48866);
#13452=VERTEX_POINT('',#48868);
#13453=VERTEX_POINT('',#48870);
#13454=VERTEX_POINT('',#48872);
#13455=VERTEX_POINT('',#48874);
#13456=VERTEX_POINT('',#48876);
#13457=VERTEX_POINT('',#48878);
#13458=VERTEX_POINT('',#48880);
#13459=VERTEX_POINT('',#48882);
#13460=VERTEX_POINT('',#48884);
#13461=VERTEX_POINT('',#48886);
#13462=VERTEX_POINT('',#48888);
#13463=VERTEX_POINT('',#48895);
#13464=VERTEX_POINT('',#48897);
#13465=VERTEX_POINT('',#48901);
#13466=VERTEX_POINT('',#48905);
#13467=VERTEX_POINT('',#48909);
#13468=VERTEX_POINT('',#48913);
#13469=VERTEX_POINT('',#48915);
#13470=VERTEX_POINT('',#48919);
#13471=VERTEX_POINT('',#48923);
#13472=VERTEX_POINT('',#48927);
#13473=VERTEX_POINT('',#48931);
#13474=VERTEX_POINT('',#48937);
#13475=VERTEX_POINT('',#48939);
#13476=VERTEX_POINT('',#48943);
#13477=VERTEX_POINT('',#48949);
#13478=VERTEX_POINT('',#48957);
#13479=VERTEX_POINT('',#48958);
#13480=VERTEX_POINT('',#48960);
#13481=VERTEX_POINT('',#48962);
#13482=VERTEX_POINT('',#48964);
#13483=VERTEX_POINT('',#48966);
#13484=VERTEX_POINT('',#48968);
#13485=VERTEX_POINT('',#48970);
#13486=VERTEX_POINT('',#48973);
#13487=VERTEX_POINT('',#48975);
#13488=VERTEX_POINT('',#48977);
#13489=VERTEX_POINT('',#48979);
#13490=VERTEX_POINT('',#48981);
#13491=VERTEX_POINT('',#48982);
#13492=VERTEX_POINT('',#48984);
#13493=VERTEX_POINT('',#48986);
#13494=VERTEX_POINT('',#48988);
#13495=VERTEX_POINT('',#48990);
#13496=VERTEX_POINT('',#48992);
#13497=VERTEX_POINT('',#48994);
#13498=VERTEX_POINT('',#48998);
#13499=VERTEX_POINT('',#48999);
#13500=VERTEX_POINT('',#49004);
#13501=VERTEX_POINT('',#49006);
#13502=VERTEX_POINT('',#49010);
#13503=VERTEX_POINT('',#49012);
#13504=VERTEX_POINT('',#49016);
#13505=VERTEX_POINT('',#49017);
#13506=VERTEX_POINT('',#49019);
#13507=VERTEX_POINT('',#49021);
#13508=VERTEX_POINT('',#49023);
#13509=VERTEX_POINT('',#49025);
#13510=VERTEX_POINT('',#49028);
#13511=VERTEX_POINT('',#49031);
#13512=VERTEX_POINT('',#49032);
#13513=VERTEX_POINT('',#49034);
#13514=VERTEX_POINT('',#49036);
#13515=VERTEX_POINT('',#49038);
#13516=VERTEX_POINT('',#49040);
#13517=VERTEX_POINT('',#49043);
#13518=VERTEX_POINT('',#49046);
#13519=VERTEX_POINT('',#49047);
#13520=VERTEX_POINT('',#49050);
#13521=VERTEX_POINT('',#49053);
#13522=VERTEX_POINT('',#49056);
#13523=VERTEX_POINT('',#49057);
#13524=VERTEX_POINT('',#49059);
#13525=VERTEX_POINT('',#49061);
#13526=VERTEX_POINT('',#49063);
#13527=VERTEX_POINT('',#49065);
#13528=VERTEX_POINT('',#49068);
#13529=VERTEX_POINT('',#49079);
#13530=VERTEX_POINT('',#49081);
#13531=VERTEX_POINT('',#49120);
#13532=VERTEX_POINT('',#49130);
#13533=VERTEX_POINT('',#49155);
#13534=VERTEX_POINT('',#49156);
#13535=VERTEX_POINT('',#49158);
#13536=VERTEX_POINT('',#49161);
#13537=VERTEX_POINT('',#49171);
#13538=VERTEX_POINT('',#49173);
#13539=VERTEX_POINT('',#49183);
#13540=VERTEX_POINT('',#49185);
#13541=VERTEX_POINT('',#49195);
#13542=VERTEX_POINT('',#49197);
#13543=VERTEX_POINT('',#49207);
#13544=VERTEX_POINT('',#49209);
#13545=VERTEX_POINT('',#49219);
#13546=VERTEX_POINT('',#49221);
#13547=VERTEX_POINT('',#49231);
#13548=VERTEX_POINT('',#49233);
#13549=VERTEX_POINT('',#49246);
#13550=VERTEX_POINT('',#49247);
#13551=VERTEX_POINT('',#49252);
#13552=VERTEX_POINT('',#49254);
#13553=VERTEX_POINT('',#49258);
#13554=VERTEX_POINT('',#49259);
#13555=VERTEX_POINT('',#49261);
#13556=VERTEX_POINT('',#49263);
#13557=VERTEX_POINT('',#49267);
#13558=VERTEX_POINT('',#49268);
#13559=VERTEX_POINT('',#49270);
#13560=VERTEX_POINT('',#49272);
#13561=VERTEX_POINT('',#49276);
#13562=VERTEX_POINT('',#49277);
#13563=VERTEX_POINT('',#49279);
#13564=VERTEX_POINT('',#49281);
#13565=VERTEX_POINT('',#49286);
#13566=VERTEX_POINT('',#49347);
#13567=VERTEX_POINT('',#49351);
#13568=VERTEX_POINT('',#49355);
#13569=VERTEX_POINT('',#49362);
#13570=VERTEX_POINT('',#49363);
#13571=VERTEX_POINT('',#49365);
#13572=VERTEX_POINT('',#49376);
#13573=VERTEX_POINT('',#49378);
#13574=VERTEX_POINT('',#49395);
#13575=VERTEX_POINT('',#49401);
#13576=VERTEX_POINT('',#49402);
#13577=VERTEX_POINT('',#49414);
#13578=VERTEX_POINT('',#49470);
#13579=VERTEX_POINT('',#49580);
#13580=VERTEX_POINT('',#49688);
#13581=VERTEX_POINT('',#49700);
#13582=VERTEX_POINT('',#49860);
#13583=VERTEX_POINT('',#49969);
#13584=VERTEX_POINT('',#50068);
#13585=VERTEX_POINT('',#50094);
#13586=VERTEX_POINT('',#50199);
#13587=VERTEX_POINT('',#50243);
#13588=VERTEX_POINT('',#50256);
#13589=VERTEX_POINT('',#50270);
#13590=VERTEX_POINT('',#50274);
#13591=VERTEX_POINT('',#50281);
#13592=VERTEX_POINT('',#50285);
#13593=VERTEX_POINT('',#50296);
#13594=VERTEX_POINT('',#50298);
#13595=VERTEX_POINT('',#50313);
#13596=VERTEX_POINT('',#50317);
#13597=VERTEX_POINT('',#50404);
#13598=VERTEX_POINT('',#50429);
#13599=VERTEX_POINT('',#50697);
#13600=VERTEX_POINT('',#50764);
#13601=VERTEX_POINT('',#50869);
#13602=VERTEX_POINT('',#50873);
#13603=VERTEX_POINT('',#50876);
#13604=VERTEX_POINT('',#50877);
#13605=VERTEX_POINT('',#50882);
#13606=VERTEX_POINT('',#50886);
#13607=VERTEX_POINT('',#50889);
#13608=VERTEX_POINT('',#50893);
#13609=VERTEX_POINT('',#50896);
#13610=VERTEX_POINT('',#50900);
#13611=VERTEX_POINT('',#50903);
#13612=VERTEX_POINT('',#50907);
#13613=VERTEX_POINT('',#50910);
#13614=VERTEX_POINT('',#50914);
#13615=VERTEX_POINT('',#50917);
#13616=VERTEX_POINT('',#50921);
#13617=VERTEX_POINT('',#50924);
#13618=VERTEX_POINT('',#50928);
#13619=VERTEX_POINT('',#50929);
#13620=VERTEX_POINT('',#50931);
#13621=VERTEX_POINT('',#50933);
#13622=VERTEX_POINT('',#50935);
#13623=VERTEX_POINT('',#50937);
#13624=VERTEX_POINT('',#50939);
#13625=VERTEX_POINT('',#50941);
#13626=VERTEX_POINT('',#50962);
#13627=VERTEX_POINT('',#50963);
#13628=VERTEX_POINT('',#50966);
#13629=VERTEX_POINT('',#50970);
#13630=VERTEX_POINT('',#50971);
#13631=VERTEX_POINT('',#50976);
#13632=VERTEX_POINT('',#50979);
#13633=VERTEX_POINT('',#50984);
#13634=VERTEX_POINT('',#50985);
#13635=VERTEX_POINT('',#50988);
#13636=VERTEX_POINT('',#50992);
#13637=VERTEX_POINT('',#50993);
#13638=VERTEX_POINT('',#50995);
#13639=VERTEX_POINT('',#50997);
#13640=VERTEX_POINT('',#50999);
#13641=VERTEX_POINT('',#51001);
#13642=VERTEX_POINT('',#51007);
#13643=VERTEX_POINT('',#51008);
#13644=VERTEX_POINT('',#51015);
#13645=VERTEX_POINT('',#51021);
#13646=VERTEX_POINT('',#51027);
#13647=VERTEX_POINT('',#51033);
#13648=VERTEX_POINT('',#51037);
#13649=VERTEX_POINT('',#51047);
#13650=VERTEX_POINT('',#51051);
#13651=VERTEX_POINT('',#51052);
#13652=VERTEX_POINT('',#51055);
#13653=VERTEX_POINT('',#51059);
#13654=VERTEX_POINT('',#51060);
#13655=VERTEX_POINT('',#51065);
#13656=VERTEX_POINT('',#51068);
#13657=VERTEX_POINT('',#51073);
#13658=VERTEX_POINT('',#51074);
#13659=VERTEX_POINT('',#51077);
#13660=VERTEX_POINT('',#51081);
#13661=VERTEX_POINT('',#51082);
#13662=VERTEX_POINT('',#51084);
#13663=VERTEX_POINT('',#51086);
#13664=VERTEX_POINT('',#51088);
#13665=VERTEX_POINT('',#51090);
#13666=VERTEX_POINT('',#51096);
#13667=VERTEX_POINT('',#51097);
#13668=VERTEX_POINT('',#51104);
#13669=VERTEX_POINT('',#51110);
#13670=VERTEX_POINT('',#51116);
#13671=VERTEX_POINT('',#51122);
#13672=VERTEX_POINT('',#51126);
#13673=VERTEX_POINT('',#51136);
#13674=VERTEX_POINT('',#51140);
#13675=VERTEX_POINT('',#51141);
#13676=VERTEX_POINT('',#51144);
#13677=VERTEX_POINT('',#51148);
#13678=VERTEX_POINT('',#51149);
#13679=VERTEX_POINT('',#51154);
#13680=VERTEX_POINT('',#51157);
#13681=VERTEX_POINT('',#51162);
#13682=VERTEX_POINT('',#51163);
#13683=VERTEX_POINT('',#51166);
#13684=VERTEX_POINT('',#51170);
#13685=VERTEX_POINT('',#51171);
#13686=VERTEX_POINT('',#51173);
#13687=VERTEX_POINT('',#51175);
#13688=VERTEX_POINT('',#51177);
#13689=VERTEX_POINT('',#51179);
#13690=VERTEX_POINT('',#51185);
#13691=VERTEX_POINT('',#51186);
#13692=VERTEX_POINT('',#51193);
#13693=VERTEX_POINT('',#51199);
#13694=VERTEX_POINT('',#51205);
#13695=VERTEX_POINT('',#51211);
#13696=VERTEX_POINT('',#51215);
#13697=VERTEX_POINT('',#51225);
#13698=VERTEX_POINT('',#51229);
#13699=VERTEX_POINT('',#51230);
#13700=VERTEX_POINT('',#51233);
#13701=VERTEX_POINT('',#51237);
#13702=VERTEX_POINT('',#51238);
#13703=VERTEX_POINT('',#51243);
#13704=VERTEX_POINT('',#51246);
#13705=VERTEX_POINT('',#51251);
#13706=VERTEX_POINT('',#51252);
#13707=VERTEX_POINT('',#51256);
#13708=VERTEX_POINT('',#51262);
#13709=VERTEX_POINT('',#51263);
#13710=VERTEX_POINT('',#51272);
#13711=VERTEX_POINT('',#51273);
#13712=VERTEX_POINT('',#51282);
#13713=VERTEX_POINT('',#51283);
#13714=VERTEX_POINT('',#51292);
#13715=VERTEX_POINT('',#51293);
#13716=VERTEX_POINT('',#51302);
#13717=VERTEX_POINT('',#51311);
#13718=VERTEX_POINT('',#51313);
#13719=VERTEX_POINT('',#51317);
#13720=VERTEX_POINT('',#51321);
#13721=VERTEX_POINT('',#51325);
#13722=VERTEX_POINT('',#51327);
#13723=VERTEX_POINT('',#51330);
#13724=VERTEX_POINT('',#51342);
#13725=VERTEX_POINT('',#51343);
#13726=VERTEX_POINT('',#51345);
#13727=VERTEX_POINT('',#51347);
#13728=VERTEX_POINT('',#51351);
#13729=VERTEX_POINT('',#51353);
#13730=VERTEX_POINT('',#51357);
#13731=VERTEX_POINT('',#51359);
#13732=VERTEX_POINT('',#51366);
#13733=VERTEX_POINT('',#51367);
#13734=VERTEX_POINT('',#51369);
#13735=VERTEX_POINT('',#51371);
#13736=VERTEX_POINT('',#51375);
#13737=VERTEX_POINT('',#51377);
#13738=VERTEX_POINT('',#51381);
#13739=VERTEX_POINT('',#51383);
#13740=VERTEX_POINT('',#51391);
#13741=VERTEX_POINT('',#51392);
#13742=VERTEX_POINT('',#51394);
#13743=VERTEX_POINT('',#51396);
#13744=VERTEX_POINT('',#51400);
#13745=VERTEX_POINT('',#51402);
#13746=VERTEX_POINT('',#51406);
#13747=VERTEX_POINT('',#51408);
#13748=VERTEX_POINT('',#51418);
#13749=VERTEX_POINT('',#51420);
#13750=VERTEX_POINT('',#51424);
#13751=VERTEX_POINT('',#51426);
#13752=VERTEX_POINT('',#51430);
#13753=VERTEX_POINT('',#51432);
#13754=VERTEX_POINT('',#51436);
#13755=VERTEX_POINT('',#51438);
#13756=VERTEX_POINT('',#51442);
#13757=VERTEX_POINT('',#51444);
#13758=VERTEX_POINT('',#51448);
#13759=VERTEX_POINT('',#51450);
#13760=VERTEX_POINT('',#51454);
#13761=VERTEX_POINT('',#51455);
#13762=VERTEX_POINT('',#51457);
#13763=VERTEX_POINT('',#51459);
#13764=VERTEX_POINT('',#51462);
#13765=VERTEX_POINT('',#51463);
#13766=VERTEX_POINT('',#51465);
#13767=VERTEX_POINT('',#51467);
#13768=VERTEX_POINT('',#51471);
#13769=VERTEX_POINT('',#51472);
#13770=VERTEX_POINT('',#51477);
#13771=VERTEX_POINT('',#51481);
#13772=VERTEX_POINT('',#51487);
#13773=VERTEX_POINT('',#51489);
#13774=VERTEX_POINT('',#51493);
#13775=VERTEX_POINT('',#51495);
#13776=VERTEX_POINT('',#51497);
#13777=VERTEX_POINT('',#51501);
#13778=VERTEX_POINT('',#51502);
#13779=VERTEX_POINT('',#51504);
#13780=VERTEX_POINT('',#51506);
#13781=VERTEX_POINT('',#51510);
#13782=VERTEX_POINT('',#51512);
#13783=VERTEX_POINT('',#51516);
#13784=VERTEX_POINT('',#51517);
#13785=VERTEX_POINT('',#51519);
#13786=VERTEX_POINT('',#51521);
#13787=VERTEX_POINT('',#51525);
#13788=VERTEX_POINT('',#51527);
#13789=VERTEX_POINT('',#51531);
#13790=VERTEX_POINT('',#51533);
#13791=VERTEX_POINT('',#51537);
#13792=VERTEX_POINT('',#51539);
#13793=VERTEX_POINT('',#51550);
#13794=VERTEX_POINT('',#51554);
#13795=VERTEX_POINT('',#51558);
#13796=VERTEX_POINT('',#51592);
#13797=VERTEX_POINT('',#51593);
#13798=VERTEX_POINT('',#51598);
#13799=VERTEX_POINT('',#51602);
#13800=VERTEX_POINT('',#51605);
#13801=VERTEX_POINT('',#51610);
#13802=VERTEX_POINT('',#51619);
#13803=VERTEX_POINT('',#51628);
#13804=VERTEX_POINT('',#51636);
#13805=VERTEX_POINT('',#51645);
#13806=VERTEX_POINT('',#51654);
#13807=VERTEX_POINT('',#51662);
#13808=VERTEX_POINT('',#51671);
#13809=VERTEX_POINT('',#51680);
#13810=VERTEX_POINT('',#51688);
#13811=VERTEX_POINT('',#51706);
#13812=VERTEX_POINT('',#51708);
#13813=VERTEX_POINT('',#51712);
#13814=VERTEX_POINT('',#51716);
#13815=VERTEX_POINT('',#51720);
#13816=VERTEX_POINT('',#51721);
#13817=VERTEX_POINT('',#51725);
#13818=VERTEX_POINT('',#51748);
#13819=VERTEX_POINT('',#51749);
#13820=VERTEX_POINT('',#51751);
#13821=VERTEX_POINT('',#51762);
#13822=VERTEX_POINT('',#51764);
#13823=VERTEX_POINT('',#51766);
#13824=VERTEX_POINT('',#51785);
#13825=VERTEX_POINT('',#51787);
#13826=VERTEX_POINT('',#51789);
#13827=VERTEX_POINT('',#51800);
#13828=VERTEX_POINT('',#51803);
#13829=VERTEX_POINT('',#51804);
#13830=VERTEX_POINT('',#51815);
#13831=VERTEX_POINT('',#51828);
#13832=VERTEX_POINT('',#51830);
#13833=VERTEX_POINT('',#51852);
#13834=VERTEX_POINT('',#51853);
#13835=VERTEX_POINT('',#51873);
#13836=VERTEX_POINT('',#51875);
#13837=VERTEX_POINT('',#51896);
#13838=VERTEX_POINT('',#51897);
#13839=VERTEX_POINT('',#51899);
#13840=VERTEX_POINT('',#51910);
#13841=VERTEX_POINT('',#51923);
#13842=VERTEX_POINT('',#51925);
#13843=VERTEX_POINT('',#51929);
#13844=VERTEX_POINT('',#51931);
#13845=VERTEX_POINT('',#51935);
#13846=VERTEX_POINT('',#51936);
#13847=VERTEX_POINT('',#51938);
#13848=VERTEX_POINT('',#51949);
#13849=VERTEX_POINT('',#51963);
#13850=VERTEX_POINT('',#51966);
#13851=VERTEX_POINT('',#51968);
#13852=VERTEX_POINT('',#51970);
#13853=VERTEX_POINT('',#51981);
#13854=VERTEX_POINT('',#51985);
#13855=VERTEX_POINT('',#51986);
#13856=VERTEX_POINT('',#51988);
#13857=VERTEX_POINT('',#52011);
#13858=VERTEX_POINT('',#52012);
#13859=VERTEX_POINT('',#52014);
#13860=VERTEX_POINT('',#52016);
#13861=VERTEX_POINT('',#52018);
#13862=VERTEX_POINT('',#52020);
#13863=VERTEX_POINT('',#52022);
#13864=VERTEX_POINT('',#52024);
#13865=VERTEX_POINT('',#52026);
#13866=VERTEX_POINT('',#52028);
#13867=VERTEX_POINT('',#52030);
#13868=VERTEX_POINT('',#52032);
#13869=VERTEX_POINT('',#52036);
#13870=VERTEX_POINT('',#52037);
#13871=VERTEX_POINT('',#52039);
#13872=VERTEX_POINT('',#52041);
#13873=VERTEX_POINT('',#52045);
#13874=VERTEX_POINT('',#52047);
#13875=VERTEX_POINT('',#52053);
#13876=VERTEX_POINT('',#52058);
#13877=VERTEX_POINT('',#52062);
#13878=VERTEX_POINT('',#52063);
#13879=VERTEX_POINT('',#52065);
#13880=VERTEX_POINT('',#52067);
#13881=VERTEX_POINT('',#52071);
#13882=VERTEX_POINT('',#52073);
#13883=VERTEX_POINT('',#52077);
#13884=VERTEX_POINT('',#52079);
#13885=VERTEX_POINT('',#52083);
#13886=VERTEX_POINT('',#52085);
#13887=VERTEX_POINT('',#52089);
#13888=VERTEX_POINT('',#52091);
#13889=VERTEX_POINT('',#52095);
#13890=VERTEX_POINT('',#52097);
#13891=VERTEX_POINT('',#52101);
#13892=VERTEX_POINT('',#52103);
#13893=VERTEX_POINT('',#52107);
#13894=VERTEX_POINT('',#52109);
#13895=VERTEX_POINT('',#52113);
#13896=VERTEX_POINT('',#52115);
#13897=VERTEX_POINT('',#52119);
#13898=VERTEX_POINT('',#52121);
#13899=VERTEX_POINT('',#52125);
#13900=VERTEX_POINT('',#52127);
#13901=VERTEX_POINT('',#52137);
#13902=VERTEX_POINT('',#52150);
#13903=VERTEX_POINT('',#52151);
#13904=VERTEX_POINT('',#52153);
#13905=VERTEX_POINT('',#52155);
#13906=VERTEX_POINT('',#52159);
#13907=VERTEX_POINT('',#52161);
#13908=VERTEX_POINT('',#52165);
#13909=VERTEX_POINT('',#52167);
#13910=VERTEX_POINT('',#52171);
#13911=VERTEX_POINT('',#52173);
#13912=VERTEX_POINT('',#52177);
#13913=VERTEX_POINT('',#52179);
#13914=VERTEX_POINT('',#52183);
#13915=VERTEX_POINT('',#52185);
#13916=VERTEX_POINT('',#52189);
#13917=VERTEX_POINT('',#52191);
#13918=VERTEX_POINT('',#52198);
#13919=VERTEX_POINT('',#52199);
#13920=VERTEX_POINT('',#52201);
#13921=VERTEX_POINT('',#52203);
#13922=VERTEX_POINT('',#52207);
#13923=VERTEX_POINT('',#52209);
#13924=VERTEX_POINT('',#52211);
#13925=VERTEX_POINT('',#52212);
#13926=VERTEX_POINT('',#52214);
#13927=VERTEX_POINT('',#52216);
#13928=VERTEX_POINT('',#52218);
#13929=VERTEX_POINT('',#52220);
#13930=VERTEX_POINT('',#52222);
#13931=VERTEX_POINT('',#52224);
#13932=VERTEX_POINT('',#52228);
#13933=VERTEX_POINT('',#52230);
#13934=VERTEX_POINT('',#52234);
#13935=VERTEX_POINT('',#52238);
#13936=VERTEX_POINT('',#52242);
#13937=VERTEX_POINT('',#52246);
#13938=VERTEX_POINT('',#52250);
#13939=VERTEX_POINT('',#52254);
#13940=VERTEX_POINT('',#52261);
#13941=VERTEX_POINT('',#52263);
#13942=VERTEX_POINT('',#52264);
#13943=VERTEX_POINT('',#52266);
#13944=VERTEX_POINT('',#52268);
#13945=VERTEX_POINT('',#52270);
#13946=VERTEX_POINT('',#52272);
#13947=VERTEX_POINT('',#52274);
#13948=VERTEX_POINT('',#52276);
#13949=VERTEX_POINT('',#52278);
#13950=VERTEX_POINT('',#52280);
#13951=VERTEX_POINT('',#52282);
#13952=VERTEX_POINT('',#52284);
#13953=VERTEX_POINT('',#52290);
#13954=VERTEX_POINT('',#52292);
#13955=VERTEX_POINT('',#52293);
#13956=VERTEX_POINT('',#52295);
#13957=VERTEX_POINT('',#52297);
#13958=VERTEX_POINT('',#52299);
#13959=VERTEX_POINT('',#52301);
#13960=VERTEX_POINT('',#52303);
#13961=VERTEX_POINT('',#52305);
#13962=VERTEX_POINT('',#52307);
#13963=VERTEX_POINT('',#52309);
#13964=VERTEX_POINT('',#52311);
#13965=VERTEX_POINT('',#52313);
#13966=VERTEX_POINT('',#52319);
#13967=VERTEX_POINT('',#52321);
#13968=VERTEX_POINT('',#52325);
#13969=VERTEX_POINT('',#52329);
#13970=VERTEX_POINT('',#52333);
#13971=VERTEX_POINT('',#52337);
#13972=VERTEX_POINT('',#52341);
#13973=VERTEX_POINT('',#52345);
#13974=VERTEX_POINT('',#52349);
#13975=VERTEX_POINT('',#52353);
#13976=VERTEX_POINT('',#52357);
#13977=VERTEX_POINT('',#52361);
#13978=VERTEX_POINT('',#52368);
#13979=VERTEX_POINT('',#52370);
#13980=VERTEX_POINT('',#52374);
#13981=VERTEX_POINT('',#52378);
#13982=VERTEX_POINT('',#52382);
#13983=VERTEX_POINT('',#52386);
#13984=VERTEX_POINT('',#52390);
#13985=VERTEX_POINT('',#52394);
#13986=VERTEX_POINT('',#52398);
#13987=VERTEX_POINT('',#52402);
#13988=VERTEX_POINT('',#52406);
#13989=VERTEX_POINT('',#52410);
#13990=VERTEX_POINT('',#52417);
#13991=VERTEX_POINT('',#52419);
#13992=VERTEX_POINT('',#52421);
#13993=VERTEX_POINT('',#52423);
#13994=VERTEX_POINT('',#52425);
#13995=VERTEX_POINT('',#52427);
#13996=VERTEX_POINT('',#52429);
#13997=VERTEX_POINT('',#52431);
#13998=VERTEX_POINT('',#52452);
#13999=VERTEX_POINT('',#52453);
#14000=VERTEX_POINT('',#52467);
#14001=VERTEX_POINT('',#52475);
#14002=VERTEX_POINT('',#52477);
#14003=VERTEX_POINT('',#52500);
#14004=VERTEX_POINT('',#52506);
#14005=VERTEX_POINT('',#52510);
#14006=VERTEX_POINT('',#52512);
#14007=VERTEX_POINT('',#52516);
#14008=VERTEX_POINT('',#52520);
#14009=VERTEX_POINT('',#52524);
#14010=VERTEX_POINT('',#52528);
#14011=VERTEX_POINT('',#52532);
#14012=VERTEX_POINT('',#52536);
#14013=VERTEX_POINT('',#52540);
#14014=VERTEX_POINT('',#52544);
#14015=VERTEX_POINT('',#52548);
#14016=VERTEX_POINT('',#52552);
#14017=VERTEX_POINT('',#52556);
#14018=VERTEX_POINT('',#52564);
#14019=VERTEX_POINT('',#52566);
#14020=VERTEX_POINT('',#52568);
#14021=VERTEX_POINT('',#52570);
#14022=VERTEX_POINT('',#52572);
#14023=VERTEX_POINT('',#52574);
#14024=VERTEX_POINT('',#52576);
#14025=VERTEX_POINT('',#52578);
#14026=VERTEX_POINT('',#52580);
#14027=VERTEX_POINT('',#52584);
#14028=VERTEX_POINT('',#52586);
#14029=VERTEX_POINT('',#52588);
#14030=VERTEX_POINT('',#52590);
#14031=VERTEX_POINT('',#52592);
#14032=VERTEX_POINT('',#52594);
#14033=VERTEX_POINT('',#52596);
#14034=VERTEX_POINT('',#52598);
#14035=VERTEX_POINT('',#52600);
#14036=VERTEX_POINT('',#52623);
#14037=VERTEX_POINT('',#52625);
#14038=VERTEX_POINT('',#52628);
#14039=VERTEX_POINT('',#52629);
#14040=VERTEX_POINT('',#52648);
#14041=VERTEX_POINT('',#52650);
#14042=VERTEX_POINT('',#52672);
#14043=VERTEX_POINT('',#52673);
#14044=VERTEX_POINT('',#52677);
#14045=VERTEX_POINT('',#52678);
#14046=VERTEX_POINT('',#52697);
#14047=VERTEX_POINT('',#52699);
#14048=VERTEX_POINT('',#52721);
#14049=VERTEX_POINT('',#52722);
#14050=VERTEX_POINT('',#52724);
#14051=VERTEX_POINT('',#52732);
#14052=VERTEX_POINT('',#52733);
#14053=VERTEX_POINT('',#52752);
#14054=VERTEX_POINT('',#52802);
#14055=VERTEX_POINT('',#52803);
#14056=VERTEX_POINT('',#52863);
#14057=VERTEX_POINT('',#52864);
#14058=VERTEX_POINT('',#52867);
#14059=VERTEX_POINT('',#52874);
#14060=VERTEX_POINT('',#52877);
#14061=VERTEX_POINT('',#52879);
#14062=VERTEX_POINT('',#52883);
#14063=VERTEX_POINT('',#52884);
#14064=VERTEX_POINT('',#52886);
#14065=VERTEX_POINT('',#52888);
#14066=VERTEX_POINT('',#52892);
#14067=VERTEX_POINT('',#52894);
#14068=VERTEX_POINT('',#52896);
#14069=VERTEX_POINT('',#52898);
#14070=VERTEX_POINT('',#52900);
#14071=VERTEX_POINT('',#52902);
#14072=VERTEX_POINT('',#52904);
#14073=VERTEX_POINT('',#52906);
#14074=VERTEX_POINT('',#52908);
#14075=VERTEX_POINT('',#52910);
#14076=VERTEX_POINT('',#52912);
#14077=VERTEX_POINT('',#52914);
#14078=VERTEX_POINT('',#52916);
#14079=VERTEX_POINT('',#52918);
#14080=VERTEX_POINT('',#52922);
#14081=VERTEX_POINT('',#52926);
#14082=VERTEX_POINT('',#52927);
#14083=VERTEX_POINT('',#52929);
#14084=VERTEX_POINT('',#52931);
#14085=VERTEX_POINT('',#52933);
#14086=VERTEX_POINT('',#52935);
#14087=VERTEX_POINT('',#52939);
#14088=VERTEX_POINT('',#52940);
#14089=VERTEX_POINT('',#52942);
#14090=VERTEX_POINT('',#52944);
#14091=VERTEX_POINT('',#52946);
#14092=VERTEX_POINT('',#52948);
#14093=VERTEX_POINT('',#52952);
#14094=VERTEX_POINT('',#52953);
#14095=VERTEX_POINT('',#52955);
#14096=VERTEX_POINT('',#52957);
#14097=VERTEX_POINT('',#52960);
#14098=VERTEX_POINT('',#52961);
#14099=VERTEX_POINT('',#52963);
#14100=VERTEX_POINT('',#52965);
#14101=VERTEX_POINT('',#52969);
#14102=VERTEX_POINT('',#52970);
#14103=VERTEX_POINT('',#52975);
#14104=VERTEX_POINT('',#52979);
#14105=VERTEX_POINT('',#52985);
#14106=VERTEX_POINT('',#52986);
#14107=VERTEX_POINT('',#52988);
#14108=VERTEX_POINT('',#52990);
#14109=VERTEX_POINT('',#52996);
#14110=VERTEX_POINT('',#52997);
#14111=VERTEX_POINT('',#53002);
#14112=VERTEX_POINT('',#53006);
#14113=VERTEX_POINT('',#53012);
#14114=VERTEX_POINT('',#53015);
#14115=VERTEX_POINT('',#53017);
#14116=VERTEX_POINT('',#53021);
#14117=VERTEX_POINT('',#53025);
#14118=VERTEX_POINT('',#53028);
#14119=VERTEX_POINT('',#53030);
#14120=VERTEX_POINT('',#53034);
#14121=VERTEX_POINT('',#53038);
#14122=VERTEX_POINT('',#53041);
#14123=VERTEX_POINT('',#53043);
#14124=VERTEX_POINT('',#53047);
#14125=VERTEX_POINT('',#53051);
#14126=VERTEX_POINT('',#53054);
#14127=VERTEX_POINT('',#53056);
#14128=VERTEX_POINT('',#53060);
#14129=VERTEX_POINT('',#53064);
#14130=VERTEX_POINT('',#53068);
#14131=VERTEX_POINT('',#53070);
#14132=VERTEX_POINT('',#53072);
#14133=VERTEX_POINT('',#53074);
#14134=VERTEX_POINT('',#53076);
#14135=VERTEX_POINT('',#53079);
#14136=VERTEX_POINT('',#53083);
#14137=VERTEX_POINT('',#53086);
#14138=VERTEX_POINT('',#53090);
#14139=VERTEX_POINT('',#53093);
#14140=VERTEX_POINT('',#53097);
#14141=VERTEX_POINT('',#53102);
#14142=VERTEX_POINT('',#53104);
#14143=VERTEX_POINT('',#53109);
#14144=VERTEX_POINT('',#53114);
#14145=VERTEX_POINT('',#53118);
#14146=VERTEX_POINT('',#53121);
#14147=VERTEX_POINT('',#53126);
#14148=VERTEX_POINT('',#53129);
#14149=VERTEX_POINT('',#53133);
#14150=VERTEX_POINT('',#53138);
#14151=VERTEX_POINT('',#53142);
#14152=VERTEX_POINT('',#53145);
#14153=VERTEX_POINT('',#53150);
#14154=VERTEX_POINT('',#53151);
#14155=VERTEX_POINT('',#53153);
#14156=VERTEX_POINT('',#53156);
#14157=VERTEX_POINT('',#53160);
#14158=VERTEX_POINT('',#53161);
#14159=VERTEX_POINT('',#53166);
#14160=VERTEX_POINT('',#53169);
#14161=VERTEX_POINT('',#53175);
#14162=VERTEX_POINT('',#53183);
#14163=VERTEX_POINT('',#53189);
#14164=VERTEX_POINT('',#53194);
#14165=VERTEX_POINT('',#53195);
#14166=VERTEX_POINT('',#53197);
#14167=VERTEX_POINT('',#53199);
#14168=VERTEX_POINT('',#53201);
#14169=VERTEX_POINT('',#53203);
#14170=VERTEX_POINT('',#53205);
#14171=VERTEX_POINT('',#53207);
#14172=VERTEX_POINT('',#53209);
#14173=VERTEX_POINT('',#53212);
#14174=VERTEX_POINT('',#53214);
#14175=VERTEX_POINT('',#53216);
#14176=VERTEX_POINT('',#53218);
#14177=VERTEX_POINT('',#53223);
#14178=VERTEX_POINT('',#53230);
#14179=VERTEX_POINT('',#53231);
#14180=VERTEX_POINT('',#53233);
#14181=VERTEX_POINT('',#53235);
#14182=VERTEX_POINT('',#53237);
#14183=VERTEX_POINT('',#53239);
#14184=VERTEX_POINT('',#53241);
#14185=VERTEX_POINT('',#53243);
#14186=VERTEX_POINT('',#53245);
#14187=VERTEX_POINT('',#53247);
#14188=VERTEX_POINT('',#53249);
#14189=VERTEX_POINT('',#53251);
#14190=VERTEX_POINT('',#53253);
#14191=VERTEX_POINT('',#53255);
#14192=VERTEX_POINT('',#53257);
#14193=VERTEX_POINT('',#53259);
#14194=VERTEX_POINT('',#53263);
#14195=VERTEX_POINT('',#53265);
#14196=VERTEX_POINT('',#53269);
#14197=VERTEX_POINT('',#53273);
#14198=VERTEX_POINT('',#53277);
#14199=VERTEX_POINT('',#53281);
#14200=VERTEX_POINT('',#53285);
#14201=VERTEX_POINT('',#53289);
#14202=VERTEX_POINT('',#53293);
#14203=VERTEX_POINT('',#53297);
#14204=VERTEX_POINT('',#53301);
#14205=VERTEX_POINT('',#53305);
#14206=VERTEX_POINT('',#53309);
#14207=VERTEX_POINT('',#53313);
#14208=VERTEX_POINT('',#53317);
#14209=VERTEX_POINT('',#53321);
#14210=VERTEX_POINT('',#53356);
#14211=VERTEX_POINT('',#53357);
#14212=VERTEX_POINT('',#53359);
#14213=VERTEX_POINT('',#53361);
#14214=VERTEX_POINT('',#53365);
#14215=VERTEX_POINT('',#53367);
#14216=VERTEX_POINT('',#53369);
#14217=VERTEX_POINT('',#53371);
#14218=VERTEX_POINT('',#53373);
#14219=VERTEX_POINT('',#53375);
#14220=VERTEX_POINT('',#53377);
#14221=VERTEX_POINT('',#53379);
#14222=VERTEX_POINT('',#53381);
#14223=VERTEX_POINT('',#53383);
#14224=VERTEX_POINT('',#53386);
#14225=VERTEX_POINT('',#53388);
#14226=VERTEX_POINT('',#53390);
#14227=VERTEX_POINT('',#53391);
#14228=VERTEX_POINT('',#53393);
#14229=VERTEX_POINT('',#53395);
#14230=VERTEX_POINT('',#53398);
#14231=VERTEX_POINT('',#53400);
#14232=VERTEX_POINT('',#53403);
#14233=VERTEX_POINT('',#53405);
#14234=VERTEX_POINT('',#53409);
#14235=VERTEX_POINT('',#53411);
#14236=VERTEX_POINT('',#53413);
#14237=VERTEX_POINT('',#53415);
#14238=VERTEX_POINT('',#53417);
#14239=VERTEX_POINT('',#53419);
#14240=VERTEX_POINT('',#53421);
#14241=VERTEX_POINT('',#53423);
#14242=VERTEX_POINT('',#53425);
#14243=VERTEX_POINT('',#53427);
#14244=VERTEX_POINT('',#53429);
#14245=VERTEX_POINT('',#53431);
#14246=VERTEX_POINT('',#53435);
#14247=VERTEX_POINT('',#53437);
#14248=VERTEX_POINT('',#53439);
#14249=VERTEX_POINT('',#53441);
#14250=VERTEX_POINT('',#53460);
#14251=VERTEX_POINT('',#53488);
#14252=VERTEX_POINT('',#53501);
#14253=VERTEX_POINT('',#53503);
#14254=VERTEX_POINT('',#53507);
#14255=VERTEX_POINT('',#53512);
#14256=VERTEX_POINT('',#53514);
#14257=VERTEX_POINT('',#53516);
#14258=VERTEX_POINT('',#53520);
#14259=VERTEX_POINT('',#53522);
#14260=VERTEX_POINT('',#53526);
#14261=VERTEX_POINT('',#53528);
#14262=VERTEX_POINT('',#53532);
#14263=VERTEX_POINT('',#53537);
#14264=VERTEX_POINT('',#53538);
#14265=VERTEX_POINT('',#53540);
#14266=VERTEX_POINT('',#53544);
#14267=VERTEX_POINT('',#53545);
#14268=VERTEX_POINT('',#53550);
#14269=VERTEX_POINT('',#53551);
#14270=VERTEX_POINT('',#53553);
#14271=VERTEX_POINT('',#53557);
#14272=VERTEX_POINT('',#53558);
#14273=VERTEX_POINT('',#53563);
#14274=VERTEX_POINT('',#53564);
#14275=VERTEX_POINT('',#53566);
#14276=VERTEX_POINT('',#53568);
#14277=VERTEX_POINT('',#53572);
#14278=VERTEX_POINT('',#53573);
#14279=VERTEX_POINT('',#53578);
#14280=VERTEX_POINT('',#53579);
#14281=VERTEX_POINT('',#53581);
#14282=VERTEX_POINT('',#53585);
#14283=VERTEX_POINT('',#53586);
#14284=VERTEX_POINT('',#53588);
#14285=VERTEX_POINT('',#53595);
#14286=VERTEX_POINT('',#53596);
#14287=VERTEX_POINT('',#53601);
#14288=VERTEX_POINT('',#53603);
#14289=VERTEX_POINT('',#53612);
#14290=VERTEX_POINT('',#53613);
#14291=VERTEX_POINT('',#53618);
#14292=VERTEX_POINT('',#53657);
#14293=VERTEX_POINT('',#53661);
#14294=VERTEX_POINT('',#53664);
#14295=VERTEX_POINT('',#53668);
#14296=VERTEX_POINT('',#53670);
#14297=VERTEX_POINT('',#53675);
#14298=VERTEX_POINT('',#53677);
#14299=VERTEX_POINT('',#53681);
#14300=VERTEX_POINT('',#53683);
#14301=VERTEX_POINT('',#53685);
#14302=VERTEX_POINT('',#53686);
#14303=VERTEX_POINT('',#53688);
#14304=VERTEX_POINT('',#53690);
#14305=VERTEX_POINT('',#53693);
#14306=VERTEX_POINT('',#53695);
#14307=VERTEX_POINT('',#53702);
#14308=VERTEX_POINT('',#53706);
#14309=VERTEX_POINT('',#53708);
#14310=VERTEX_POINT('',#53712);
#14311=VERTEX_POINT('',#53716);
#14312=VERTEX_POINT('',#53718);
#14313=VERTEX_POINT('',#53722);
#14314=VERTEX_POINT('',#53726);
#14315=VERTEX_POINT('',#53728);
#14316=VERTEX_POINT('',#53732);
#14317=VERTEX_POINT('',#53736);
#14318=VERTEX_POINT('',#53738);
#14319=VERTEX_POINT('',#53753);
#14320=VERTEX_POINT('',#53755);
#14321=VERTEX_POINT('',#53764);
#14322=VERTEX_POINT('',#53783);
#14323=VERTEX_POINT('',#53784);
#14324=VERTEX_POINT('',#53786);
#14325=VERTEX_POINT('',#53788);
#14326=VERTEX_POINT('',#53792);
#14327=VERTEX_POINT('',#53794);
#14328=VERTEX_POINT('',#53798);
#14329=VERTEX_POINT('',#53800);
#14330=VERTEX_POINT('',#53804);
#14331=VERTEX_POINT('',#53806);
#14332=VERTEX_POINT('',#53810);
#14333=VERTEX_POINT('',#53811);
#14334=VERTEX_POINT('',#53813);
#14335=VERTEX_POINT('',#53815);
#14336=VERTEX_POINT('',#53819);
#14337=VERTEX_POINT('',#53821);
#14338=VERTEX_POINT('',#53825);
#14339=VERTEX_POINT('',#53827);
#14340=VERTEX_POINT('',#53831);
#14341=VERTEX_POINT('',#53833);
#14342=VERTEX_POINT('',#53837);
#14343=VERTEX_POINT('',#53839);
#14344=VERTEX_POINT('',#53843);
#14345=VERTEX_POINT('',#53845);
#14346=VERTEX_POINT('',#53849);
#14347=VERTEX_POINT('',#53851);
#14348=VERTEX_POINT('',#53858);
#14349=VERTEX_POINT('',#53860);
#14350=VERTEX_POINT('',#53864);
#14351=VERTEX_POINT('',#53866);
#14352=VERTEX_POINT('',#53870);
#14353=VERTEX_POINT('',#53872);
#14354=VERTEX_POINT('',#53881);
#14355=VERTEX_POINT('',#53882);
#14356=VERTEX_POINT('',#53884);
#14357=VERTEX_POINT('',#53886);
#14358=VERTEX_POINT('',#53890);
#14359=VERTEX_POINT('',#53892);
#14360=VERTEX_POINT('',#53896);
#14361=VERTEX_POINT('',#53898);
#14362=VERTEX_POINT('',#53902);
#14363=VERTEX_POINT('',#53904);
#14364=VERTEX_POINT('',#53908);
#14365=VERTEX_POINT('',#53909);
#14366=VERTEX_POINT('',#53911);
#14367=VERTEX_POINT('',#53913);
#14368=VERTEX_POINT('',#53917);
#14369=VERTEX_POINT('',#53919);
#14370=VERTEX_POINT('',#53923);
#14371=VERTEX_POINT('',#53925);
#14372=VERTEX_POINT('',#53929);
#14373=VERTEX_POINT('',#53931);
#14374=VERTEX_POINT('',#53935);
#14375=VERTEX_POINT('',#53937);
#14376=VERTEX_POINT('',#53941);
#14377=VERTEX_POINT('',#53943);
#14378=VERTEX_POINT('',#53947);
#14379=VERTEX_POINT('',#53949);
#14380=VERTEX_POINT('',#53956);
#14381=VERTEX_POINT('',#53958);
#14382=VERTEX_POINT('',#53962);
#14383=VERTEX_POINT('',#53964);
#14384=VERTEX_POINT('',#53968);
#14385=VERTEX_POINT('',#53970);
#14386=VERTEX_POINT('',#53979);
#14387=VERTEX_POINT('',#53980);
#14388=VERTEX_POINT('',#53982);
#14389=VERTEX_POINT('',#53984);
#14390=VERTEX_POINT('',#53988);
#14391=VERTEX_POINT('',#53990);
#14392=VERTEX_POINT('',#53994);
#14393=VERTEX_POINT('',#53996);
#14394=VERTEX_POINT('',#54000);
#14395=VERTEX_POINT('',#54002);
#14396=VERTEX_POINT('',#54006);
#14397=VERTEX_POINT('',#54007);
#14398=VERTEX_POINT('',#54009);
#14399=VERTEX_POINT('',#54011);
#14400=VERTEX_POINT('',#54015);
#14401=VERTEX_POINT('',#54017);
#14402=VERTEX_POINT('',#54021);
#14403=VERTEX_POINT('',#54023);
#14404=VERTEX_POINT('',#54027);
#14405=VERTEX_POINT('',#54029);
#14406=VERTEX_POINT('',#54033);
#14407=VERTEX_POINT('',#54035);
#14408=VERTEX_POINT('',#54039);
#14409=VERTEX_POINT('',#54041);
#14410=VERTEX_POINT('',#54045);
#14411=VERTEX_POINT('',#54047);
#14412=VERTEX_POINT('',#54054);
#14413=VERTEX_POINT('',#54056);
#14414=VERTEX_POINT('',#54060);
#14415=VERTEX_POINT('',#54062);
#14416=VERTEX_POINT('',#54066);
#14417=VERTEX_POINT('',#54068);
#14418=VERTEX_POINT('',#54077);
#14419=VERTEX_POINT('',#54078);
#14420=VERTEX_POINT('',#54080);
#14421=VERTEX_POINT('',#54082);
#14422=VERTEX_POINT('',#54086);
#14423=VERTEX_POINT('',#54088);
#14424=VERTEX_POINT('',#54092);
#14425=VERTEX_POINT('',#54094);
#14426=VERTEX_POINT('',#54098);
#14427=VERTEX_POINT('',#54100);
#14428=VERTEX_POINT('',#54104);
#14429=VERTEX_POINT('',#54105);
#14430=VERTEX_POINT('',#54107);
#14431=VERTEX_POINT('',#54109);
#14432=VERTEX_POINT('',#54113);
#14433=VERTEX_POINT('',#54115);
#14434=VERTEX_POINT('',#54119);
#14435=VERTEX_POINT('',#54121);
#14436=VERTEX_POINT('',#54125);
#14437=VERTEX_POINT('',#54127);
#14438=VERTEX_POINT('',#54131);
#14439=VERTEX_POINT('',#54133);
#14440=VERTEX_POINT('',#54137);
#14441=VERTEX_POINT('',#54139);
#14442=VERTEX_POINT('',#54143);
#14443=VERTEX_POINT('',#54145);
#14444=VERTEX_POINT('',#54152);
#14445=VERTEX_POINT('',#54154);
#14446=VERTEX_POINT('',#54158);
#14447=VERTEX_POINT('',#54160);
#14448=VERTEX_POINT('',#54164);
#14449=VERTEX_POINT('',#54166);
#14450=VERTEX_POINT('',#54175);
#14451=VERTEX_POINT('',#54176);
#14452=VERTEX_POINT('',#54178);
#14453=VERTEX_POINT('',#54180);
#14454=VERTEX_POINT('',#54182);
#14455=VERTEX_POINT('',#54184);
#14456=VERTEX_POINT('',#54186);
#14457=VERTEX_POINT('',#54188);
#14458=VERTEX_POINT('',#54191);
#14459=VERTEX_POINT('',#54192);
#14460=VERTEX_POINT('',#54194);
#14461=VERTEX_POINT('',#54196);
#14462=VERTEX_POINT('',#54198);
#14463=VERTEX_POINT('',#54200);
#14464=VERTEX_POINT('',#54202);
#14465=VERTEX_POINT('',#54204);
#14466=VERTEX_POINT('',#54208);
#14467=VERTEX_POINT('',#54210);
#14468=VERTEX_POINT('',#54214);
#14469=VERTEX_POINT('',#54218);
#14470=VERTEX_POINT('',#54222);
#14471=VERTEX_POINT('',#54226);
#14472=VERTEX_POINT('',#54228);
#14473=VERTEX_POINT('',#54232);
#14474=VERTEX_POINT('',#54234);
#14475=VERTEX_POINT('',#54238);
#14476=VERTEX_POINT('',#54243);
#14477=VERTEX_POINT('',#54245);
#14478=VERTEX_POINT('',#54247);
#14479=VERTEX_POINT('',#54250);
#14480=VERTEX_POINT('',#54252);
#14481=VERTEX_POINT('',#54254);
#14482=VERTEX_POINT('',#54273);
#14483=VERTEX_POINT('',#54274);
#14484=VERTEX_POINT('',#54276);
#14485=VERTEX_POINT('',#54278);
#14486=VERTEX_POINT('',#54280);
#14487=VERTEX_POINT('',#54282);
#14488=VERTEX_POINT('',#54284);
#14489=VERTEX_POINT('',#54286);
#14490=VERTEX_POINT('',#54289);
#14491=VERTEX_POINT('',#54290);
#14492=VERTEX_POINT('',#54292);
#14493=VERTEX_POINT('',#54294);
#14494=VERTEX_POINT('',#54296);
#14495=VERTEX_POINT('',#54298);
#14496=VERTEX_POINT('',#54300);
#14497=VERTEX_POINT('',#54302);
#14498=VERTEX_POINT('',#54306);
#14499=VERTEX_POINT('',#54308);
#14500=VERTEX_POINT('',#54312);
#14501=VERTEX_POINT('',#54316);
#14502=VERTEX_POINT('',#54320);
#14503=VERTEX_POINT('',#54324);
#14504=VERTEX_POINT('',#54326);
#14505=VERTEX_POINT('',#54330);
#14506=VERTEX_POINT('',#54334);
#14507=VERTEX_POINT('',#54338);
#14508=VERTEX_POINT('',#54342);
#14509=VERTEX_POINT('',#54344);
#14510=VERTEX_POINT('',#54346);
#14511=VERTEX_POINT('',#54349);
#14512=VERTEX_POINT('',#54351);
#14513=VERTEX_POINT('',#54353);
#14514=VERTEX_POINT('',#54371);
#14515=VERTEX_POINT('',#54372);
#14516=VERTEX_POINT('',#54374);
#14517=VERTEX_POINT('',#54376);
#14518=VERTEX_POINT('',#54378);
#14519=VERTEX_POINT('',#54380);
#14520=VERTEX_POINT('',#54382);
#14521=VERTEX_POINT('',#54384);
#14522=VERTEX_POINT('',#54387);
#14523=VERTEX_POINT('',#54388);
#14524=VERTEX_POINT('',#54390);
#14525=VERTEX_POINT('',#54392);
#14526=VERTEX_POINT('',#54394);
#14527=VERTEX_POINT('',#54396);
#14528=VERTEX_POINT('',#54398);
#14529=VERTEX_POINT('',#54400);
#14530=VERTEX_POINT('',#54404);
#14531=VERTEX_POINT('',#54406);
#14532=VERTEX_POINT('',#54410);
#14533=VERTEX_POINT('',#54414);
#14534=VERTEX_POINT('',#54418);
#14535=VERTEX_POINT('',#54422);
#14536=VERTEX_POINT('',#54424);
#14537=VERTEX_POINT('',#54428);
#14538=VERTEX_POINT('',#54432);
#14539=VERTEX_POINT('',#54436);
#14540=VERTEX_POINT('',#54440);
#14541=VERTEX_POINT('',#54442);
#14542=VERTEX_POINT('',#54444);
#14543=VERTEX_POINT('',#54447);
#14544=VERTEX_POINT('',#54449);
#14545=VERTEX_POINT('',#54451);
#14546=VERTEX_POINT('',#54469);
#14547=VERTEX_POINT('',#54470);
#14548=VERTEX_POINT('',#54472);
#14549=VERTEX_POINT('',#54474);
#14550=VERTEX_POINT('',#54476);
#14551=VERTEX_POINT('',#54478);
#14552=VERTEX_POINT('',#54480);
#14553=VERTEX_POINT('',#54482);
#14554=VERTEX_POINT('',#54485);
#14555=VERTEX_POINT('',#54486);
#14556=VERTEX_POINT('',#54488);
#14557=VERTEX_POINT('',#54490);
#14558=VERTEX_POINT('',#54492);
#14559=VERTEX_POINT('',#54494);
#14560=VERTEX_POINT('',#54496);
#14561=VERTEX_POINT('',#54498);
#14562=VERTEX_POINT('',#54502);
#14563=VERTEX_POINT('',#54504);
#14564=VERTEX_POINT('',#54508);
#14565=VERTEX_POINT('',#54512);
#14566=VERTEX_POINT('',#54516);
#14567=VERTEX_POINT('',#54520);
#14568=VERTEX_POINT('',#54522);
#14569=VERTEX_POINT('',#54526);
#14570=VERTEX_POINT('',#54530);
#14571=VERTEX_POINT('',#54534);
#14572=VERTEX_POINT('',#54538);
#14573=VERTEX_POINT('',#54540);
#14574=VERTEX_POINT('',#54542);
#14575=VERTEX_POINT('',#54545);
#14576=VERTEX_POINT('',#54547);
#14577=VERTEX_POINT('',#54549);
#14578=VERTEX_POINT('',#54567);
#14579=VERTEX_POINT('',#54568);
#14580=VERTEX_POINT('',#54570);
#14581=VERTEX_POINT('',#54572);
#14582=VERTEX_POINT('',#54576);
#14583=VERTEX_POINT('',#54578);
#14584=VERTEX_POINT('',#54582);
#14585=VERTEX_POINT('',#54584);
#14586=VERTEX_POINT('',#54588);
#14587=VERTEX_POINT('',#54590);
#14588=VERTEX_POINT('',#54594);
#14589=VERTEX_POINT('',#54595);
#14590=VERTEX_POINT('',#54597);
#14591=VERTEX_POINT('',#54599);
#14592=VERTEX_POINT('',#54603);
#14593=VERTEX_POINT('',#54605);
#14594=VERTEX_POINT('',#54609);
#14595=VERTEX_POINT('',#54611);
#14596=VERTEX_POINT('',#54615);
#14597=VERTEX_POINT('',#54617);
#14598=VERTEX_POINT('',#54621);
#14599=VERTEX_POINT('',#54623);
#14600=VERTEX_POINT('',#54627);
#14601=VERTEX_POINT('',#54629);
#14602=VERTEX_POINT('',#54633);
#14603=VERTEX_POINT('',#54635);
#14604=VERTEX_POINT('',#54642);
#14605=VERTEX_POINT('',#54644);
#14606=VERTEX_POINT('',#54648);
#14607=VERTEX_POINT('',#54650);
#14608=VERTEX_POINT('',#54654);
#14609=VERTEX_POINT('',#54656);
#14610=VERTEX_POINT('',#54665);
#14611=VERTEX_POINT('',#54666);
#14612=VERTEX_POINT('',#54668);
#14613=VERTEX_POINT('',#54670);
#14614=VERTEX_POINT('',#54674);
#14615=VERTEX_POINT('',#54676);
#14616=VERTEX_POINT('',#54680);
#14617=VERTEX_POINT('',#54682);
#14618=VERTEX_POINT('',#54686);
#14619=VERTEX_POINT('',#54688);
#14620=VERTEX_POINT('',#54692);
#14621=VERTEX_POINT('',#54693);
#14622=VERTEX_POINT('',#54695);
#14623=VERTEX_POINT('',#54697);
#14624=VERTEX_POINT('',#54701);
#14625=VERTEX_POINT('',#54703);
#14626=VERTEX_POINT('',#54707);
#14627=VERTEX_POINT('',#54709);
#14628=VERTEX_POINT('',#54713);
#14629=VERTEX_POINT('',#54715);
#14630=VERTEX_POINT('',#54719);
#14631=VERTEX_POINT('',#54721);
#14632=VERTEX_POINT('',#54725);
#14633=VERTEX_POINT('',#54727);
#14634=VERTEX_POINT('',#54731);
#14635=VERTEX_POINT('',#54733);
#14636=VERTEX_POINT('',#54740);
#14637=VERTEX_POINT('',#54742);
#14638=VERTEX_POINT('',#54746);
#14639=VERTEX_POINT('',#54748);
#14640=VERTEX_POINT('',#54752);
#14641=VERTEX_POINT('',#54754);
#14642=VERTEX_POINT('',#54763);
#14643=VERTEX_POINT('',#54764);
#14644=VERTEX_POINT('',#54766);
#14645=VERTEX_POINT('',#54768);
#14646=VERTEX_POINT('',#54772);
#14647=VERTEX_POINT('',#54774);
#14648=VERTEX_POINT('',#54778);
#14649=VERTEX_POINT('',#54780);
#14650=VERTEX_POINT('',#54784);
#14651=VERTEX_POINT('',#54786);
#14652=VERTEX_POINT('',#54790);
#14653=VERTEX_POINT('',#54791);
#14654=VERTEX_POINT('',#54793);
#14655=VERTEX_POINT('',#54795);
#14656=VERTEX_POINT('',#54799);
#14657=VERTEX_POINT('',#54801);
#14658=VERTEX_POINT('',#54805);
#14659=VERTEX_POINT('',#54807);
#14660=VERTEX_POINT('',#54811);
#14661=VERTEX_POINT('',#54813);
#14662=VERTEX_POINT('',#54817);
#14663=VERTEX_POINT('',#54819);
#14664=VERTEX_POINT('',#54823);
#14665=VERTEX_POINT('',#54825);
#14666=VERTEX_POINT('',#54829);
#14667=VERTEX_POINT('',#54831);
#14668=VERTEX_POINT('',#54838);
#14669=VERTEX_POINT('',#54840);
#14670=VERTEX_POINT('',#54844);
#14671=VERTEX_POINT('',#54846);
#14672=VERTEX_POINT('',#54850);
#14673=VERTEX_POINT('',#54852);
#14674=VERTEX_POINT('',#54861);
#14675=VERTEX_POINT('',#54862);
#14676=VERTEX_POINT('',#54864);
#14677=VERTEX_POINT('',#54866);
#14678=VERTEX_POINT('',#54870);
#14679=VERTEX_POINT('',#54872);
#14680=VERTEX_POINT('',#54876);
#14681=VERTEX_POINT('',#54878);
#14682=VERTEX_POINT('',#54882);
#14683=VERTEX_POINT('',#54884);
#14684=VERTEX_POINT('',#54888);
#14685=VERTEX_POINT('',#54890);
#14686=VERTEX_POINT('',#54894);
#14687=VERTEX_POINT('',#54896);
#14688=VERTEX_POINT('',#54900);
#14689=VERTEX_POINT('',#54902);
#14690=VERTEX_POINT('',#54909);
#14691=VERTEX_POINT('',#54910);
#14692=VERTEX_POINT('',#54912);
#14693=VERTEX_POINT('',#54914);
#14694=VERTEX_POINT('',#54918);
#14695=VERTEX_POINT('',#54920);
#14696=VERTEX_POINT('',#54924);
#14697=VERTEX_POINT('',#54926);
#14698=VERTEX_POINT('',#54930);
#14699=VERTEX_POINT('',#54932);
#14700=VERTEX_POINT('',#54936);
#14701=VERTEX_POINT('',#54938);
#14702=VERTEX_POINT('',#54942);
#14703=VERTEX_POINT('',#54944);
#14704=VERTEX_POINT('',#54948);
#14705=VERTEX_POINT('',#54950);
#14706=VERTEX_POINT('',#54959);
#14707=VERTEX_POINT('',#54960);
#14708=VERTEX_POINT('',#54962);
#14709=VERTEX_POINT('',#54964);
#14710=VERTEX_POINT('',#54968);
#14711=VERTEX_POINT('',#54970);
#14712=VERTEX_POINT('',#54974);
#14713=VERTEX_POINT('',#54976);
#14714=VERTEX_POINT('',#54980);
#14715=VERTEX_POINT('',#54982);
#14716=VERTEX_POINT('',#54986);
#14717=VERTEX_POINT('',#54988);
#14718=VERTEX_POINT('',#54992);
#14719=VERTEX_POINT('',#54994);
#14720=VERTEX_POINT('',#54998);
#14721=VERTEX_POINT('',#55000);
#14722=VERTEX_POINT('',#55007);
#14723=VERTEX_POINT('',#55008);
#14724=VERTEX_POINT('',#55010);
#14725=VERTEX_POINT('',#55012);
#14726=VERTEX_POINT('',#55016);
#14727=VERTEX_POINT('',#55018);
#14728=VERTEX_POINT('',#55022);
#14729=VERTEX_POINT('',#55024);
#14730=VERTEX_POINT('',#55028);
#14731=VERTEX_POINT('',#55030);
#14732=VERTEX_POINT('',#55034);
#14733=VERTEX_POINT('',#55036);
#14734=VERTEX_POINT('',#55040);
#14735=VERTEX_POINT('',#55042);
#14736=VERTEX_POINT('',#55046);
#14737=VERTEX_POINT('',#55048);
#14738=VERTEX_POINT('',#55057);
#14739=VERTEX_POINT('',#55058);
#14740=VERTEX_POINT('',#55060);
#14741=VERTEX_POINT('',#55062);
#14742=VERTEX_POINT('',#55066);
#14743=VERTEX_POINT('',#55068);
#14744=VERTEX_POINT('',#55072);
#14745=VERTEX_POINT('',#55074);
#14746=VERTEX_POINT('',#55078);
#14747=VERTEX_POINT('',#55080);
#14748=VERTEX_POINT('',#55084);
#14749=VERTEX_POINT('',#55086);
#14750=VERTEX_POINT('',#55090);
#14751=VERTEX_POINT('',#55092);
#14752=VERTEX_POINT('',#55096);
#14753=VERTEX_POINT('',#55098);
#14754=VERTEX_POINT('',#55105);
#14755=VERTEX_POINT('',#55106);
#14756=VERTEX_POINT('',#55108);
#14757=VERTEX_POINT('',#55110);
#14758=VERTEX_POINT('',#55114);
#14759=VERTEX_POINT('',#55116);
#14760=VERTEX_POINT('',#55120);
#14761=VERTEX_POINT('',#55122);
#14762=VERTEX_POINT('',#55126);
#14763=VERTEX_POINT('',#55128);
#14764=VERTEX_POINT('',#55132);
#14765=VERTEX_POINT('',#55134);
#14766=VERTEX_POINT('',#55138);
#14767=VERTEX_POINT('',#55140);
#14768=VERTEX_POINT('',#55144);
#14769=VERTEX_POINT('',#55146);
#14770=VERTEX_POINT('',#55155);
#14771=VERTEX_POINT('',#55156);
#14772=VERTEX_POINT('',#55158);
#14773=VERTEX_POINT('',#55160);
#14774=VERTEX_POINT('',#55164);
#14775=VERTEX_POINT('',#55166);
#14776=VERTEX_POINT('',#55170);
#14777=VERTEX_POINT('',#55172);
#14778=VERTEX_POINT('',#55176);
#14779=VERTEX_POINT('',#55178);
#14780=VERTEX_POINT('',#55182);
#14781=VERTEX_POINT('',#55184);
#14782=VERTEX_POINT('',#55188);
#14783=VERTEX_POINT('',#55190);
#14784=VERTEX_POINT('',#55194);
#14785=VERTEX_POINT('',#55196);
#14786=VERTEX_POINT('',#55203);
#14787=VERTEX_POINT('',#55204);
#14788=VERTEX_POINT('',#55206);
#14789=VERTEX_POINT('',#55208);
#14790=VERTEX_POINT('',#55212);
#14791=VERTEX_POINT('',#55214);
#14792=VERTEX_POINT('',#55218);
#14793=VERTEX_POINT('',#55220);
#14794=VERTEX_POINT('',#55224);
#14795=VERTEX_POINT('',#55226);
#14796=VERTEX_POINT('',#55230);
#14797=VERTEX_POINT('',#55232);
#14798=VERTEX_POINT('',#55236);
#14799=VERTEX_POINT('',#55238);
#14800=VERTEX_POINT('',#55242);
#14801=VERTEX_POINT('',#55244);
#14802=VERTEX_POINT('',#55255);
#14803=VERTEX_POINT('',#55257);
#14804=VERTEX_POINT('',#55261);
#14805=VERTEX_POINT('',#55263);
#14806=VERTEX_POINT('',#55267);
#14807=VERTEX_POINT('',#55269);
#14808=VERTEX_POINT('',#55273);
#14809=VERTEX_POINT('',#55275);
#14810=VERTEX_POINT('',#55279);
#14811=VERTEX_POINT('',#55281);
#14812=VERTEX_POINT('',#55285);
#14813=VERTEX_POINT('',#55287);
#14814=VERTEX_POINT('',#55291);
#14815=VERTEX_POINT('',#55293);
#14816=VERTEX_POINT('',#55297);
#14817=VERTEX_POINT('',#55299);
#14818=VERTEX_POINT('',#55303);
#14819=VERTEX_POINT('',#55305);
#14820=VERTEX_POINT('',#55309);
#14821=VERTEX_POINT('',#55311);
#14822=VERTEX_POINT('',#55315);
#14823=VERTEX_POINT('',#55317);
#14824=VERTEX_POINT('',#55321);
#14825=VERTEX_POINT('',#55323);
#14826=VERTEX_POINT('',#55327);
#14827=VERTEX_POINT('',#55329);
#14828=VERTEX_POINT('',#55333);
#14829=VERTEX_POINT('',#55335);
#14830=VERTEX_POINT('',#55339);
#14831=VERTEX_POINT('',#55341);
#14832=VERTEX_POINT('',#55345);
#14833=VERTEX_POINT('',#55347);
#14834=VERTEX_POINT('',#55351);
#14835=VERTEX_POINT('',#55352);
#14836=VERTEX_POINT('',#55354);
#14837=VERTEX_POINT('',#55356);
#14838=VERTEX_POINT('',#55360);
#14839=VERTEX_POINT('',#55362);
#14840=VERTEX_POINT('',#55366);
#14841=VERTEX_POINT('',#55368);
#14842=VERTEX_POINT('',#55375);
#14843=VERTEX_POINT('',#55376);
#14844=VERTEX_POINT('',#55378);
#14845=VERTEX_POINT('',#55380);
#14846=VERTEX_POINT('',#55384);
#14847=VERTEX_POINT('',#55386);
#14848=VERTEX_POINT('',#55390);
#14849=VERTEX_POINT('',#55394);
#14850=VERTEX_POINT('',#55402);
#14851=VERTEX_POINT('',#55403);
#14852=VERTEX_POINT('',#55405);
#14853=VERTEX_POINT('',#55407);
#14854=VERTEX_POINT('',#55410);
#14855=VERTEX_POINT('',#55412);
#14856=VERTEX_POINT('',#55414);
#14857=VERTEX_POINT('',#55417);
#14858=VERTEX_POINT('',#55418);
#14859=VERTEX_POINT('',#55420);
#14860=VERTEX_POINT('',#55422);
#14861=VERTEX_POINT('',#55425);
#14862=VERTEX_POINT('',#55427);
#14863=VERTEX_POINT('',#55429);
#14864=VERTEX_POINT('',#55435);
#14865=VERTEX_POINT('',#55436);
#14866=VERTEX_POINT('',#55442);
#14867=VERTEX_POINT('',#55443);
#14868=VERTEX_POINT('',#55449);
#14869=VERTEX_POINT('',#55450);
#14870=VERTEX_POINT('',#55456);
#14871=VERTEX_POINT('',#55457);
#14872=VERTEX_POINT('',#55463);
#14873=VERTEX_POINT('',#55464);
#14874=VERTEX_POINT('',#55470);
#14875=VERTEX_POINT('',#55471);
#14876=VERTEX_POINT('',#55477);
#14877=VERTEX_POINT('',#55479);
#14878=VERTEX_POINT('',#55483);
#14879=VERTEX_POINT('',#55485);
#14880=VERTEX_POINT('',#55489);
#14881=VERTEX_POINT('',#55491);
#14882=VERTEX_POINT('',#55495);
#14883=VERTEX_POINT('',#55497);
#14884=VERTEX_POINT('',#55501);
#14885=VERTEX_POINT('',#55503);
#14886=VERTEX_POINT('',#55507);
#14887=VERTEX_POINT('',#55509);
#14888=VERTEX_POINT('',#55513);
#14889=VERTEX_POINT('',#55515);
#14890=VERTEX_POINT('',#55519);
#14891=VERTEX_POINT('',#55521);
#14892=VERTEX_POINT('',#55525);
#14893=VERTEX_POINT('',#55527);
#14894=VERTEX_POINT('',#55531);
#14895=VERTEX_POINT('',#55533);
#14896=VERTEX_POINT('',#55543);
#14897=VERTEX_POINT('',#55544);
#14898=VERTEX_POINT('',#55546);
#14899=VERTEX_POINT('',#55548);
#14900=VERTEX_POINT('',#55551);
#14901=VERTEX_POINT('',#55553);
#14902=VERTEX_POINT('',#55555);
#14903=VERTEX_POINT('',#55558);
#14904=VERTEX_POINT('',#55559);
#14905=VERTEX_POINT('',#55561);
#14906=VERTEX_POINT('',#55563);
#14907=VERTEX_POINT('',#55566);
#14908=VERTEX_POINT('',#55568);
#14909=VERTEX_POINT('',#55570);
#14910=VERTEX_POINT('',#55576);
#14911=VERTEX_POINT('',#55577);
#14912=VERTEX_POINT('',#55583);
#14913=VERTEX_POINT('',#55584);
#14914=VERTEX_POINT('',#55590);
#14915=VERTEX_POINT('',#55591);
#14916=VERTEX_POINT('',#55597);
#14917=VERTEX_POINT('',#55598);
#14918=VERTEX_POINT('',#55604);
#14919=VERTEX_POINT('',#55605);
#14920=VERTEX_POINT('',#55611);
#14921=VERTEX_POINT('',#55612);
#14922=VERTEX_POINT('',#55618);
#14923=VERTEX_POINT('',#55620);
#14924=VERTEX_POINT('',#55624);
#14925=VERTEX_POINT('',#55626);
#14926=VERTEX_POINT('',#55630);
#14927=VERTEX_POINT('',#55632);
#14928=VERTEX_POINT('',#55636);
#14929=VERTEX_POINT('',#55638);
#14930=VERTEX_POINT('',#55642);
#14931=VERTEX_POINT('',#55644);
#14932=VERTEX_POINT('',#55648);
#14933=VERTEX_POINT('',#55650);
#14934=VERTEX_POINT('',#55654);
#14935=VERTEX_POINT('',#55656);
#14936=VERTEX_POINT('',#55660);
#14937=VERTEX_POINT('',#55662);
#14938=VERTEX_POINT('',#55666);
#14939=VERTEX_POINT('',#55668);
#14940=VERTEX_POINT('',#55672);
#14941=VERTEX_POINT('',#55674);
#14942=VERTEX_POINT('',#55684);
#14943=VERTEX_POINT('',#55686);
#14944=VERTEX_POINT('',#55690);
#14945=VERTEX_POINT('',#55692);
#14946=VERTEX_POINT('',#55696);
#14947=VERTEX_POINT('',#55698);
#14948=VERTEX_POINT('',#55702);
#14949=VERTEX_POINT('',#55704);
#14950=VERTEX_POINT('',#55708);
#14951=VERTEX_POINT('',#55710);
#14952=VERTEX_POINT('',#55714);
#14953=VERTEX_POINT('',#55716);
#14954=VERTEX_POINT('',#55720);
#14955=VERTEX_POINT('',#55721);
#14956=VERTEX_POINT('',#55723);
#14957=VERTEX_POINT('',#55725);
#14958=VERTEX_POINT('',#55729);
#14959=VERTEX_POINT('',#55731);
#14960=VERTEX_POINT('',#55735);
#14961=VERTEX_POINT('',#55737);
#14962=VERTEX_POINT('',#55747);
#14963=VERTEX_POINT('',#55748);
#14964=VERTEX_POINT('',#55750);
#14965=VERTEX_POINT('',#55752);
#14966=VERTEX_POINT('',#55756);
#14967=VERTEX_POINT('',#55758);
#14968=VERTEX_POINT('',#55762);
#14969=VERTEX_POINT('',#55764);
#14970=VERTEX_POINT('',#55766);
#14971=VERTEX_POINT('',#55768);
#14972=VERTEX_POINT('',#55770);
#14973=VERTEX_POINT('',#55774);
#14974=VERTEX_POINT('',#55776);
#14975=VERTEX_POINT('',#55780);
#14976=VERTEX_POINT('',#55783);
#14977=VERTEX_POINT('',#55785);
#14978=VERTEX_POINT('',#55798);
#14979=VERTEX_POINT('',#55800);
#14980=VERTEX_POINT('',#55804);
#14981=VERTEX_POINT('',#55806);
#14982=VERTEX_POINT('',#55810);
#14983=VERTEX_POINT('',#55812);
#14984=VERTEX_POINT('',#55816);
#14985=VERTEX_POINT('',#55818);
#14986=VERTEX_POINT('',#55822);
#14987=VERTEX_POINT('',#55823);
#14988=VERTEX_POINT('',#55825);
#14989=VERTEX_POINT('',#55827);
#14990=VERTEX_POINT('',#55831);
#14991=VERTEX_POINT('',#55833);
#14992=VERTEX_POINT('',#55837);
#14993=VERTEX_POINT('',#55839);
#14994=VERTEX_POINT('',#55846);
#14995=VERTEX_POINT('',#55847);
#14996=VERTEX_POINT('',#55849);
#14997=VERTEX_POINT('',#55851);
#14998=VERTEX_POINT('',#55855);
#14999=VERTEX_POINT('',#55857);
#15000=VERTEX_POINT('',#55861);
#15001=VERTEX_POINT('',#55863);
#15002=VERTEX_POINT('',#55890);
#15003=VERTEX_POINT('',#55891);
#15004=VERTEX_POINT('',#55893);
#15005=VERTEX_POINT('',#55895);
#15006=VERTEX_POINT('',#55906);
#15007=VERTEX_POINT('',#55908);
#15008=VERTEX_POINT('',#55921);
#15009=VERTEX_POINT('',#55922);
#15010=VERTEX_POINT('',#55941);
#15011=VERTEX_POINT('',#55943);
#15012=VERTEX_POINT('',#55947);
#15013=VERTEX_POINT('',#55949);
#15014=VERTEX_POINT('',#55953);
#15015=VERTEX_POINT('',#55955);
#15016=VERTEX_POINT('',#55980);
#15017=VERTEX_POINT('',#55981);
#15018=VERTEX_POINT('',#55984);
#15019=VERTEX_POINT('',#55988);
#15020=VERTEX_POINT('',#55991);
#15021=VERTEX_POINT('',#55995);
#15022=VERTEX_POINT('',#55997);
#15023=VERTEX_POINT('',#55999);
#15024=VERTEX_POINT('',#56003);
#15025=VERTEX_POINT('',#56006);
#15026=VERTEX_POINT('',#56008);
#15027=VERTEX_POINT('',#56012);
#15028=VERTEX_POINT('',#56013);
#15029=VERTEX_POINT('',#56018);
#15030=VERTEX_POINT('',#56019);
#15031=VERTEX_POINT('',#56024);
#15032=VERTEX_POINT('',#56025);
#15033=VERTEX_POINT('',#56030);
#15034=VERTEX_POINT('',#56032);
#15035=VERTEX_POINT('',#56036);
#15036=VERTEX_POINT('',#56041);
#15037=VERTEX_POINT('',#56043);
#15038=VERTEX_POINT('',#56045);
#15039=VERTEX_POINT('',#56058);
#15040=VERTEX_POINT('',#56060);
#15041=VERTEX_POINT('',#56064);
#15042=VERTEX_POINT('',#56084);
#15043=VERTEX_POINT('',#56089);
#15044=VERTEX_POINT('',#56093);
#15045=VERTEX_POINT('',#56098);
#15046=VERTEX_POINT('',#56102);
#15047=VERTEX_POINT('',#56108);
#15048=VERTEX_POINT('',#56109);
#15049=VERTEX_POINT('',#56111);
#15050=VERTEX_POINT('',#56113);
#15051=VERTEX_POINT('',#56124);
#15052=VERTEX_POINT('',#56126);
#15053=VERTEX_POINT('',#56139);
#15054=VERTEX_POINT('',#56140);
#15055=VERTEX_POINT('',#56143);
#15056=VERTEX_POINT('',#56147);
#15057=VERTEX_POINT('',#56150);
#15058=VERTEX_POINT('',#56151);
#15059=VERTEX_POINT('',#56153);
#15060=VERTEX_POINT('',#56172);
#15061=VERTEX_POINT('',#56194);
#15062=VERTEX_POINT('',#56195);
#15063=VERTEX_POINT('',#56198);
#15064=VERTEX_POINT('',#56202);
#15065=VERTEX_POINT('',#56204);
#15066=VERTEX_POINT('',#56209);
#15067=VERTEX_POINT('',#56211);
#15068=VERTEX_POINT('',#56215);
#15069=VERTEX_POINT('',#56219);
#15070=VERTEX_POINT('',#56226);
#15071=VERTEX_POINT('',#56227);
#15072=VERTEX_POINT('',#56230);
#15073=VERTEX_POINT('',#56234);
#15074=VERTEX_POINT('',#56237);
#15075=VERTEX_POINT('',#56238);
#15076=VERTEX_POINT('',#56243);
#15077=VERTEX_POINT('',#56245);
#15078=VERTEX_POINT('',#56249);
#15079=VERTEX_POINT('',#56251);
#15080=VERTEX_POINT('',#56255);
#15081=VERTEX_POINT('',#56259);
#15082=VERTEX_POINT('',#56262);
#15083=VERTEX_POINT('',#56263);
#15084=VERTEX_POINT('',#56268);
#15085=VERTEX_POINT('',#56270);
#15086=VERTEX_POINT('',#56274);
#15087=VERTEX_POINT('',#56279);
#15088=VERTEX_POINT('',#56281);
#15089=VERTEX_POINT('',#56283);
#15090=VERTEX_POINT('',#56296);
#15091=VERTEX_POINT('',#56298);
#15092=VERTEX_POINT('',#56302);
#15093=VERTEX_POINT('',#56322);
#15094=VERTEX_POINT('',#56326);
#15095=VERTEX_POINT('',#56331);
#15096=VERTEX_POINT('',#56335);
#15097=VERTEX_POINT('',#56341);
#15098=VERTEX_POINT('',#56342);
#15099=VERTEX_POINT('',#56344);
#15100=VERTEX_POINT('',#56346);
#15101=VERTEX_POINT('',#56350);
#15102=VERTEX_POINT('',#56352);
#15103=VERTEX_POINT('',#56356);
#15104=VERTEX_POINT('',#56357);
#15105=VERTEX_POINT('',#56362);
#15106=VERTEX_POINT('',#56368);
#15107=VERTEX_POINT('',#56374);
#15108=VERTEX_POINT('',#56376);
#15109=VERTEX_POINT('',#56380);
#15110=VERTEX_POINT('',#56382);
#15111=VERTEX_POINT('',#56406);
#15112=VERTEX_POINT('',#56408);
#15113=VERTEX_POINT('',#56410);
#15114=VERTEX_POINT('',#56414);
#15115=VERTEX_POINT('',#56418);
#15116=VERTEX_POINT('',#56419);
#15117=VERTEX_POINT('',#56421);
#15118=VERTEX_POINT('',#56423);
#15119=VERTEX_POINT('',#56427);
#15120=VERTEX_POINT('',#56431);
#15121=VERTEX_POINT('',#56432);
#15122=VERTEX_POINT('',#56434);
#15123=VERTEX_POINT('',#56436);
#15124=VERTEX_POINT('',#56438);
#15125=VERTEX_POINT('',#56440);
#15126=VERTEX_POINT('',#56442);
#15127=VERTEX_POINT('',#56444);
#15128=VERTEX_POINT('',#56446);
#15129=VERTEX_POINT('',#56448);
#15130=VERTEX_POINT('',#56450);
#15131=VERTEX_POINT('',#56452);
#15132=VERTEX_POINT('',#56454);
#15133=VERTEX_POINT('',#56456);
#15134=VERTEX_POINT('',#56458);
#15135=VERTEX_POINT('',#56460);
#15136=VERTEX_POINT('',#56462);
#15137=VERTEX_POINT('',#56464);
#15138=VERTEX_POINT('',#56466);
#15139=VERTEX_POINT('',#56468);
#15140=VERTEX_POINT('',#56470);
#15141=VERTEX_POINT('',#56472);
#15142=VERTEX_POINT('',#56474);
#15143=VERTEX_POINT('',#56476);
#15144=VERTEX_POINT('',#56478);
#15145=VERTEX_POINT('',#56480);
#15146=VERTEX_POINT('',#56482);
#15147=VERTEX_POINT('',#56484);
#15148=VERTEX_POINT('',#56486);
#15149=VERTEX_POINT('',#56488);
#15150=VERTEX_POINT('',#56490);
#15151=VERTEX_POINT('',#56492);
#15152=VERTEX_POINT('',#56494);
#15153=VERTEX_POINT('',#56496);
#15154=VERTEX_POINT('',#56498);
#15155=VERTEX_POINT('',#56500);
#15156=VERTEX_POINT('',#56502);
#15157=VERTEX_POINT('',#56504);
#15158=VERTEX_POINT('',#56506);
#15159=VERTEX_POINT('',#56508);
#15160=VERTEX_POINT('',#56510);
#15161=VERTEX_POINT('',#56512);
#15162=VERTEX_POINT('',#56514);
#15163=VERTEX_POINT('',#56516);
#15164=VERTEX_POINT('',#56518);
#15165=VERTEX_POINT('',#56520);
#15166=VERTEX_POINT('',#56522);
#15167=VERTEX_POINT('',#56524);
#15168=VERTEX_POINT('',#56526);
#15169=VERTEX_POINT('',#56528);
#15170=VERTEX_POINT('',#56530);
#15171=VERTEX_POINT('',#56532);
#15172=VERTEX_POINT('',#56534);
#15173=VERTEX_POINT('',#56536);
#15174=VERTEX_POINT('',#56538);
#15175=VERTEX_POINT('',#56540);
#15176=VERTEX_POINT('',#56542);
#15177=VERTEX_POINT('',#56544);
#15178=VERTEX_POINT('',#56546);
#15179=VERTEX_POINT('',#56548);
#15180=VERTEX_POINT('',#56550);
#15181=VERTEX_POINT('',#56552);
#15182=VERTEX_POINT('',#56554);
#15183=VERTEX_POINT('',#56556);
#15184=VERTEX_POINT('',#56558);
#15185=VERTEX_POINT('',#56560);
#15186=VERTEX_POINT('',#56562);
#15187=VERTEX_POINT('',#56564);
#15188=VERTEX_POINT('',#56566);
#15189=VERTEX_POINT('',#56568);
#15190=VERTEX_POINT('',#56570);
#15191=VERTEX_POINT('',#56572);
#15192=VERTEX_POINT('',#56574);
#15193=VERTEX_POINT('',#56576);
#15194=VERTEX_POINT('',#56578);
#15195=VERTEX_POINT('',#56580);
#15196=VERTEX_POINT('',#56582);
#15197=VERTEX_POINT('',#56584);
#15198=VERTEX_POINT('',#56586);
#15199=VERTEX_POINT('',#56588);
#15200=VERTEX_POINT('',#56590);
#15201=VERTEX_POINT('',#56592);
#15202=VERTEX_POINT('',#56594);
#15203=VERTEX_POINT('',#56596);
#15204=VERTEX_POINT('',#56598);
#15205=VERTEX_POINT('',#56600);
#15206=VERTEX_POINT('',#56602);
#15207=VERTEX_POINT('',#56604);
#15208=VERTEX_POINT('',#56606);
#15209=VERTEX_POINT('',#56608);
#15210=VERTEX_POINT('',#56610);
#15211=VERTEX_POINT('',#56612);
#15212=VERTEX_POINT('',#56614);
#15213=VERTEX_POINT('',#56616);
#15214=VERTEX_POINT('',#56618);
#15215=VERTEX_POINT('',#56620);
#15216=VERTEX_POINT('',#56622);
#15217=VERTEX_POINT('',#56624);
#15218=VERTEX_POINT('',#56626);
#15219=VERTEX_POINT('',#56628);
#15220=VERTEX_POINT('',#56630);
#15221=VERTEX_POINT('',#56632);
#15222=VERTEX_POINT('',#56634);
#15223=VERTEX_POINT('',#56636);
#15224=VERTEX_POINT('',#56638);
#15225=VERTEX_POINT('',#56640);
#15226=VERTEX_POINT('',#56642);
#15227=VERTEX_POINT('',#56644);
#15228=VERTEX_POINT('',#56646);
#15229=VERTEX_POINT('',#56648);
#15230=VERTEX_POINT('',#56650);
#15231=VERTEX_POINT('',#56652);
#15232=VERTEX_POINT('',#56654);
#15233=VERTEX_POINT('',#56656);
#15234=VERTEX_POINT('',#56658);
#15235=VERTEX_POINT('',#56660);
#15236=VERTEX_POINT('',#56662);
#15237=VERTEX_POINT('',#56664);
#15238=VERTEX_POINT('',#56666);
#15239=VERTEX_POINT('',#56668);
#15240=VERTEX_POINT('',#56670);
#15241=VERTEX_POINT('',#56672);
#15242=VERTEX_POINT('',#56674);
#15243=VERTEX_POINT('',#56676);
#15244=VERTEX_POINT('',#56678);
#15245=VERTEX_POINT('',#56680);
#15246=VERTEX_POINT('',#56682);
#15247=VERTEX_POINT('',#56684);
#15248=VERTEX_POINT('',#56686);
#15249=VERTEX_POINT('',#56688);
#15250=VERTEX_POINT('',#56690);
#15251=VERTEX_POINT('',#56692);
#15252=VERTEX_POINT('',#56694);
#15253=VERTEX_POINT('',#56696);
#15254=VERTEX_POINT('',#56698);
#15255=VERTEX_POINT('',#56700);
#15256=VERTEX_POINT('',#56702);
#15257=VERTEX_POINT('',#56704);
#15258=VERTEX_POINT('',#56706);
#15259=VERTEX_POINT('',#56708);
#15260=VERTEX_POINT('',#56710);
#15261=VERTEX_POINT('',#56712);
#15262=VERTEX_POINT('',#56714);
#15263=VERTEX_POINT('',#56716);
#15264=VERTEX_POINT('',#56718);
#15265=VERTEX_POINT('',#56720);
#15266=VERTEX_POINT('',#56722);
#15267=VERTEX_POINT('',#56724);
#15268=VERTEX_POINT('',#56726);
#15269=VERTEX_POINT('',#56728);
#15270=VERTEX_POINT('',#56730);
#15271=VERTEX_POINT('',#56732);
#15272=VERTEX_POINT('',#56734);
#15273=VERTEX_POINT('',#56736);
#15274=VERTEX_POINT('',#56738);
#15275=VERTEX_POINT('',#56740);
#15276=VERTEX_POINT('',#56742);
#15277=VERTEX_POINT('',#56744);
#15278=VERTEX_POINT('',#56746);
#15279=VERTEX_POINT('',#56748);
#15280=VERTEX_POINT('',#56750);
#15281=VERTEX_POINT('',#56752);
#15282=VERTEX_POINT('',#56754);
#15283=VERTEX_POINT('',#56756);
#15284=VERTEX_POINT('',#56758);
#15285=VERTEX_POINT('',#56760);
#15286=VERTEX_POINT('',#56762);
#15287=VERTEX_POINT('',#56764);
#15288=VERTEX_POINT('',#56766);
#15289=VERTEX_POINT('',#56768);
#15290=VERTEX_POINT('',#56770);
#15291=VERTEX_POINT('',#56772);
#15292=VERTEX_POINT('',#56774);
#15293=VERTEX_POINT('',#56776);
#15294=VERTEX_POINT('',#56778);
#15295=VERTEX_POINT('',#56780);
#15296=VERTEX_POINT('',#56782);
#15297=VERTEX_POINT('',#56784);
#15298=VERTEX_POINT('',#56786);
#15299=VERTEX_POINT('',#56788);
#15300=VERTEX_POINT('',#56790);
#15301=VERTEX_POINT('',#56792);
#15302=VERTEX_POINT('',#56794);
#15303=VERTEX_POINT('',#56796);
#15304=VERTEX_POINT('',#56798);
#15305=VERTEX_POINT('',#56800);
#15306=VERTEX_POINT('',#56802);
#15307=VERTEX_POINT('',#56804);
#15308=VERTEX_POINT('',#56806);
#15309=VERTEX_POINT('',#56808);
#15310=VERTEX_POINT('',#56810);
#15311=VERTEX_POINT('',#56812);
#15312=VERTEX_POINT('',#56816);
#15313=VERTEX_POINT('',#56817);
#15314=VERTEX_POINT('',#56822);
#15315=VERTEX_POINT('',#56826);
#15316=VERTEX_POINT('',#56832);
#15317=VERTEX_POINT('',#56834);
#15318=VERTEX_POINT('',#56838);
#15319=VERTEX_POINT('',#56842);
#15320=VERTEX_POINT('',#56846);
#15321=VERTEX_POINT('',#56848);
#15322=VERTEX_POINT('',#56852);
#15323=VERTEX_POINT('',#56856);
#15324=VERTEX_POINT('',#56860);
#15325=VERTEX_POINT('',#56862);
#15326=VERTEX_POINT('',#56866);
#15327=VERTEX_POINT('',#56870);
#15328=VERTEX_POINT('',#56874);
#15329=VERTEX_POINT('',#56876);
#15330=VERTEX_POINT('',#56880);
#15331=VERTEX_POINT('',#56884);
#15332=VERTEX_POINT('',#56888);
#15333=VERTEX_POINT('',#56890);
#15334=VERTEX_POINT('',#56894);
#15335=VERTEX_POINT('',#56898);
#15336=VERTEX_POINT('',#56902);
#15337=VERTEX_POINT('',#56904);
#15338=VERTEX_POINT('',#56908);
#15339=VERTEX_POINT('',#56912);
#15340=VERTEX_POINT('',#56916);
#15341=VERTEX_POINT('',#56918);
#15342=VERTEX_POINT('',#56922);
#15343=VERTEX_POINT('',#56926);
#15344=VERTEX_POINT('',#56930);
#15345=VERTEX_POINT('',#56932);
#15346=VERTEX_POINT('',#56936);
#15347=VERTEX_POINT('',#56940);
#15348=VERTEX_POINT('',#56944);
#15349=VERTEX_POINT('',#56946);
#15350=VERTEX_POINT('',#56950);
#15351=VERTEX_POINT('',#56954);
#15352=VERTEX_POINT('',#56958);
#15353=VERTEX_POINT('',#56960);
#15354=VERTEX_POINT('',#56964);
#15355=VERTEX_POINT('',#56968);
#15356=VERTEX_POINT('',#56972);
#15357=VERTEX_POINT('',#56974);
#15358=VERTEX_POINT('',#56978);
#15359=VERTEX_POINT('',#56982);
#15360=VERTEX_POINT('',#56986);
#15361=VERTEX_POINT('',#56988);
#15362=VERTEX_POINT('',#56992);
#15363=VERTEX_POINT('',#56996);
#15364=VERTEX_POINT('',#57000);
#15365=VERTEX_POINT('',#57002);
#15366=VERTEX_POINT('',#57006);
#15367=VERTEX_POINT('',#57010);
#15368=VERTEX_POINT('',#57014);
#15369=VERTEX_POINT('',#57016);
#15370=VERTEX_POINT('',#57020);
#15371=VERTEX_POINT('',#57024);
#15372=VERTEX_POINT('',#57028);
#15373=VERTEX_POINT('',#57030);
#15374=VERTEX_POINT('',#57034);
#15375=VERTEX_POINT('',#57038);
#15376=VERTEX_POINT('',#57042);
#15377=VERTEX_POINT('',#57044);
#15378=VERTEX_POINT('',#57048);
#15379=VERTEX_POINT('',#57052);
#15380=VERTEX_POINT('',#57056);
#15381=VERTEX_POINT('',#57058);
#15382=VERTEX_POINT('',#57062);
#15383=VERTEX_POINT('',#57066);
#15384=VERTEX_POINT('',#57070);
#15385=VERTEX_POINT('',#57072);
#15386=VERTEX_POINT('',#57076);
#15387=VERTEX_POINT('',#57080);
#15388=VERTEX_POINT('',#57084);
#15389=VERTEX_POINT('',#57086);
#15390=VERTEX_POINT('',#57090);
#15391=VERTEX_POINT('',#57094);
#15392=VERTEX_POINT('',#57098);
#15393=VERTEX_POINT('',#57100);
#15394=VERTEX_POINT('',#57104);
#15395=VERTEX_POINT('',#57108);
#15396=VERTEX_POINT('',#57112);
#15397=VERTEX_POINT('',#57114);
#15398=VERTEX_POINT('',#57118);
#15399=VERTEX_POINT('',#57122);
#15400=VERTEX_POINT('',#57126);
#15401=VERTEX_POINT('',#57128);
#15402=VERTEX_POINT('',#57132);
#15403=VERTEX_POINT('',#57136);
#15404=VERTEX_POINT('',#57140);
#15405=VERTEX_POINT('',#57142);
#15406=VERTEX_POINT('',#57146);
#15407=VERTEX_POINT('',#57150);
#15408=VERTEX_POINT('',#57154);
#15409=VERTEX_POINT('',#57156);
#15410=VERTEX_POINT('',#57160);
#15411=VERTEX_POINT('',#57164);
#15412=VERTEX_POINT('',#57168);
#15413=VERTEX_POINT('',#57170);
#15414=VERTEX_POINT('',#57174);
#15415=VERTEX_POINT('',#57178);
#15416=VERTEX_POINT('',#57182);
#15417=VERTEX_POINT('',#57184);
#15418=VERTEX_POINT('',#57188);
#15419=VERTEX_POINT('',#57192);
#15420=VERTEX_POINT('',#57196);
#15421=VERTEX_POINT('',#57198);
#15422=VERTEX_POINT('',#57202);
#15423=VERTEX_POINT('',#57206);
#15424=VERTEX_POINT('',#57210);
#15425=VERTEX_POINT('',#57212);
#15426=VERTEX_POINT('',#57216);
#15427=VERTEX_POINT('',#57220);
#15428=VERTEX_POINT('',#57224);
#15429=VERTEX_POINT('',#57226);
#15430=VERTEX_POINT('',#57230);
#15431=VERTEX_POINT('',#57234);
#15432=VERTEX_POINT('',#57238);
#15433=VERTEX_POINT('',#57240);
#15434=VERTEX_POINT('',#57244);
#15435=VERTEX_POINT('',#57248);
#15436=VERTEX_POINT('',#57252);
#15437=VERTEX_POINT('',#57254);
#15438=VERTEX_POINT('',#57258);
#15439=VERTEX_POINT('',#57262);
#15440=VERTEX_POINT('',#57266);
#15441=VERTEX_POINT('',#57268);
#15442=VERTEX_POINT('',#57272);
#15443=VERTEX_POINT('',#57276);
#15444=VERTEX_POINT('',#57280);
#15445=VERTEX_POINT('',#57282);
#15446=VERTEX_POINT('',#57286);
#15447=VERTEX_POINT('',#57290);
#15448=VERTEX_POINT('',#57294);
#15449=VERTEX_POINT('',#57296);
#15450=VERTEX_POINT('',#57300);
#15451=VERTEX_POINT('',#57304);
#15452=VERTEX_POINT('',#57308);
#15453=VERTEX_POINT('',#57310);
#15454=VERTEX_POINT('',#57314);
#15455=VERTEX_POINT('',#57318);
#15456=VERTEX_POINT('',#57322);
#15457=VERTEX_POINT('',#57324);
#15458=VERTEX_POINT('',#57328);
#15459=VERTEX_POINT('',#57332);
#15460=VERTEX_POINT('',#57336);
#15461=VERTEX_POINT('',#57338);
#15462=VERTEX_POINT('',#57342);
#15463=VERTEX_POINT('',#57346);
#15464=VERTEX_POINT('',#57350);
#15465=VERTEX_POINT('',#57352);
#15466=VERTEX_POINT('',#57356);
#15467=VERTEX_POINT('',#57360);
#15468=VERTEX_POINT('',#57364);
#15469=VERTEX_POINT('',#57366);
#15470=VERTEX_POINT('',#57370);
#15471=VERTEX_POINT('',#57374);
#15472=VERTEX_POINT('',#57378);
#15473=VERTEX_POINT('',#57380);
#15474=VERTEX_POINT('',#57384);
#15475=VERTEX_POINT('',#57388);
#15476=VERTEX_POINT('',#57392);
#15477=VERTEX_POINT('',#57394);
#15478=VERTEX_POINT('',#57398);
#15479=VERTEX_POINT('',#57402);
#15480=VERTEX_POINT('',#57406);
#15481=VERTEX_POINT('',#57408);
#15482=VERTEX_POINT('',#57412);
#15483=VERTEX_POINT('',#57416);
#15484=VERTEX_POINT('',#57420);
#15485=VERTEX_POINT('',#57422);
#15486=VERTEX_POINT('',#57426);
#15487=VERTEX_POINT('',#57430);
#15488=VERTEX_POINT('',#57434);
#15489=VERTEX_POINT('',#57436);
#15490=VERTEX_POINT('',#57440);
#15491=VERTEX_POINT('',#57444);
#15492=VERTEX_POINT('',#57448);
#15493=VERTEX_POINT('',#57450);
#15494=VERTEX_POINT('',#57454);
#15495=VERTEX_POINT('',#57458);
#15496=VERTEX_POINT('',#57462);
#15497=VERTEX_POINT('',#57464);
#15498=VERTEX_POINT('',#57468);
#15499=VERTEX_POINT('',#57472);
#15500=VERTEX_POINT('',#57476);
#15501=VERTEX_POINT('',#57478);
#15502=VERTEX_POINT('',#57482);
#15503=VERTEX_POINT('',#57486);
#15504=VERTEX_POINT('',#57490);
#15505=VERTEX_POINT('',#57586);
#15506=VERTEX_POINT('',#57588);
#15507=VERTEX_POINT('',#57592);
#15508=VERTEX_POINT('',#57602);
#15509=VERTEX_POINT('',#57604);
#15510=VERTEX_POINT('',#57606);
#15511=VERTEX_POINT('',#57610);
#15512=VERTEX_POINT('',#57614);
#15513=VERTEX_POINT('',#57615);
#15514=VERTEX_POINT('',#57617);
#15515=VERTEX_POINT('',#57619);
#15516=VERTEX_POINT('',#57623);
#15517=VERTEX_POINT('',#57627);
#15518=VERTEX_POINT('',#57628);
#15519=VERTEX_POINT('',#57630);
#15520=VERTEX_POINT('',#57632);
#15521=VERTEX_POINT('',#57634);
#15522=VERTEX_POINT('',#57636);
#15523=VERTEX_POINT('',#57638);
#15524=VERTEX_POINT('',#57640);
#15525=VERTEX_POINT('',#57642);
#15526=VERTEX_POINT('',#57644);
#15527=VERTEX_POINT('',#57646);
#15528=VERTEX_POINT('',#57648);
#15529=VERTEX_POINT('',#57650);
#15530=VERTEX_POINT('',#57652);
#15531=VERTEX_POINT('',#57654);
#15532=VERTEX_POINT('',#57656);
#15533=VERTEX_POINT('',#57658);
#15534=VERTEX_POINT('',#57660);
#15535=VERTEX_POINT('',#57662);
#15536=VERTEX_POINT('',#57664);
#15537=VERTEX_POINT('',#57666);
#15538=VERTEX_POINT('',#57668);
#15539=VERTEX_POINT('',#57670);
#15540=VERTEX_POINT('',#57672);
#15541=VERTEX_POINT('',#57674);
#15542=VERTEX_POINT('',#57676);
#15543=VERTEX_POINT('',#57678);
#15544=VERTEX_POINT('',#57680);
#15545=VERTEX_POINT('',#57682);
#15546=VERTEX_POINT('',#57684);
#15547=VERTEX_POINT('',#57686);
#15548=VERTEX_POINT('',#57688);
#15549=VERTEX_POINT('',#57690);
#15550=VERTEX_POINT('',#57692);
#15551=VERTEX_POINT('',#57694);
#15552=VERTEX_POINT('',#57696);
#15553=VERTEX_POINT('',#57698);
#15554=VERTEX_POINT('',#57700);
#15555=VERTEX_POINT('',#57702);
#15556=VERTEX_POINT('',#57704);
#15557=VERTEX_POINT('',#57706);
#15558=VERTEX_POINT('',#57708);
#15559=VERTEX_POINT('',#57710);
#15560=VERTEX_POINT('',#57712);
#15561=VERTEX_POINT('',#57714);
#15562=VERTEX_POINT('',#57716);
#15563=VERTEX_POINT('',#57718);
#15564=VERTEX_POINT('',#57720);
#15565=VERTEX_POINT('',#57722);
#15566=VERTEX_POINT('',#57724);
#15567=VERTEX_POINT('',#57726);
#15568=VERTEX_POINT('',#57728);
#15569=VERTEX_POINT('',#57730);
#15570=VERTEX_POINT('',#57732);
#15571=VERTEX_POINT('',#57734);
#15572=VERTEX_POINT('',#57736);
#15573=VERTEX_POINT('',#57738);
#15574=VERTEX_POINT('',#57740);
#15575=VERTEX_POINT('',#57742);
#15576=VERTEX_POINT('',#57744);
#15577=VERTEX_POINT('',#57746);
#15578=VERTEX_POINT('',#57748);
#15579=VERTEX_POINT('',#57750);
#15580=VERTEX_POINT('',#57752);
#15581=VERTEX_POINT('',#57754);
#15582=VERTEX_POINT('',#57756);
#15583=VERTEX_POINT('',#57758);
#15584=VERTEX_POINT('',#57760);
#15585=VERTEX_POINT('',#57762);
#15586=VERTEX_POINT('',#57764);
#15587=VERTEX_POINT('',#57766);
#15588=VERTEX_POINT('',#57768);
#15589=VERTEX_POINT('',#57770);
#15590=VERTEX_POINT('',#57772);
#15591=VERTEX_POINT('',#57774);
#15592=VERTEX_POINT('',#57776);
#15593=VERTEX_POINT('',#57778);
#15594=VERTEX_POINT('',#57780);
#15595=VERTEX_POINT('',#57782);
#15596=VERTEX_POINT('',#57784);
#15597=VERTEX_POINT('',#57786);
#15598=VERTEX_POINT('',#57788);
#15599=VERTEX_POINT('',#57790);
#15600=VERTEX_POINT('',#57792);
#15601=VERTEX_POINT('',#57794);
#15602=VERTEX_POINT('',#57796);
#15603=VERTEX_POINT('',#57798);
#15604=VERTEX_POINT('',#57800);
#15605=VERTEX_POINT('',#57802);
#15606=VERTEX_POINT('',#57804);
#15607=VERTEX_POINT('',#57806);
#15608=VERTEX_POINT('',#57808);
#15609=VERTEX_POINT('',#57810);
#15610=VERTEX_POINT('',#57812);
#15611=VERTEX_POINT('',#57814);
#15612=VERTEX_POINT('',#57816);
#15613=VERTEX_POINT('',#57818);
#15614=VERTEX_POINT('',#57820);
#15615=VERTEX_POINT('',#57822);
#15616=VERTEX_POINT('',#57824);
#15617=VERTEX_POINT('',#57826);
#15618=VERTEX_POINT('',#57828);
#15619=VERTEX_POINT('',#57830);
#15620=VERTEX_POINT('',#57832);
#15621=VERTEX_POINT('',#57834);
#15622=VERTEX_POINT('',#57836);
#15623=VERTEX_POINT('',#57838);
#15624=VERTEX_POINT('',#57840);
#15625=VERTEX_POINT('',#57842);
#15626=VERTEX_POINT('',#57844);
#15627=VERTEX_POINT('',#57846);
#15628=VERTEX_POINT('',#57848);
#15629=VERTEX_POINT('',#57850);
#15630=VERTEX_POINT('',#57852);
#15631=VERTEX_POINT('',#57854);
#15632=VERTEX_POINT('',#57856);
#15633=VERTEX_POINT('',#57858);
#15634=VERTEX_POINT('',#57860);
#15635=VERTEX_POINT('',#57862);
#15636=VERTEX_POINT('',#57864);
#15637=VERTEX_POINT('',#57866);
#15638=VERTEX_POINT('',#57868);
#15639=VERTEX_POINT('',#57870);
#15640=VERTEX_POINT('',#57872);
#15641=VERTEX_POINT('',#57874);
#15642=VERTEX_POINT('',#57876);
#15643=VERTEX_POINT('',#57878);
#15644=VERTEX_POINT('',#57880);
#15645=VERTEX_POINT('',#57882);
#15646=VERTEX_POINT('',#57884);
#15647=VERTEX_POINT('',#57886);
#15648=VERTEX_POINT('',#57888);
#15649=VERTEX_POINT('',#57890);
#15650=VERTEX_POINT('',#57892);
#15651=VERTEX_POINT('',#57894);
#15652=VERTEX_POINT('',#57896);
#15653=VERTEX_POINT('',#57898);
#15654=VERTEX_POINT('',#57900);
#15655=VERTEX_POINT('',#57902);
#15656=VERTEX_POINT('',#57904);
#15657=VERTEX_POINT('',#57906);
#15658=VERTEX_POINT('',#57908);
#15659=VERTEX_POINT('',#57910);
#15660=VERTEX_POINT('',#57912);
#15661=VERTEX_POINT('',#57914);
#15662=VERTEX_POINT('',#57916);
#15663=VERTEX_POINT('',#57918);
#15664=VERTEX_POINT('',#57920);
#15665=VERTEX_POINT('',#57922);
#15666=VERTEX_POINT('',#57924);
#15667=VERTEX_POINT('',#57926);
#15668=VERTEX_POINT('',#57928);
#15669=VERTEX_POINT('',#57930);
#15670=VERTEX_POINT('',#57932);
#15671=VERTEX_POINT('',#57934);
#15672=VERTEX_POINT('',#57936);
#15673=VERTEX_POINT('',#57938);
#15674=VERTEX_POINT('',#57940);
#15675=VERTEX_POINT('',#57942);
#15676=VERTEX_POINT('',#57944);
#15677=VERTEX_POINT('',#57948);
#15678=VERTEX_POINT('',#57949);
#15679=VERTEX_POINT('',#57954);
#15680=VERTEX_POINT('',#57958);
#15681=VERTEX_POINT('',#57964);
#15682=VERTEX_POINT('',#57966);
#15683=VERTEX_POINT('',#57970);
#15684=VERTEX_POINT('',#57974);
#15685=VERTEX_POINT('',#57978);
#15686=VERTEX_POINT('',#57980);
#15687=VERTEX_POINT('',#57984);
#15688=VERTEX_POINT('',#57988);
#15689=VERTEX_POINT('',#57992);
#15690=VERTEX_POINT('',#57994);
#15691=VERTEX_POINT('',#57998);
#15692=VERTEX_POINT('',#58002);
#15693=VERTEX_POINT('',#58006);
#15694=VERTEX_POINT('',#58008);
#15695=VERTEX_POINT('',#58012);
#15696=VERTEX_POINT('',#58016);
#15697=VERTEX_POINT('',#58020);
#15698=VERTEX_POINT('',#58022);
#15699=VERTEX_POINT('',#58026);
#15700=VERTEX_POINT('',#58030);
#15701=VERTEX_POINT('',#58034);
#15702=VERTEX_POINT('',#58036);
#15703=VERTEX_POINT('',#58040);
#15704=VERTEX_POINT('',#58044);
#15705=VERTEX_POINT('',#58048);
#15706=VERTEX_POINT('',#58050);
#15707=VERTEX_POINT('',#58054);
#15708=VERTEX_POINT('',#58058);
#15709=VERTEX_POINT('',#58062);
#15710=VERTEX_POINT('',#58064);
#15711=VERTEX_POINT('',#58068);
#15712=VERTEX_POINT('',#58072);
#15713=VERTEX_POINT('',#58076);
#15714=VERTEX_POINT('',#58078);
#15715=VERTEX_POINT('',#58082);
#15716=VERTEX_POINT('',#58086);
#15717=VERTEX_POINT('',#58090);
#15718=VERTEX_POINT('',#58092);
#15719=VERTEX_POINT('',#58096);
#15720=VERTEX_POINT('',#58100);
#15721=VERTEX_POINT('',#58104);
#15722=VERTEX_POINT('',#58106);
#15723=VERTEX_POINT('',#58110);
#15724=VERTEX_POINT('',#58114);
#15725=VERTEX_POINT('',#58118);
#15726=VERTEX_POINT('',#58120);
#15727=VERTEX_POINT('',#58124);
#15728=VERTEX_POINT('',#58128);
#15729=VERTEX_POINT('',#58132);
#15730=VERTEX_POINT('',#58134);
#15731=VERTEX_POINT('',#58138);
#15732=VERTEX_POINT('',#58142);
#15733=VERTEX_POINT('',#58146);
#15734=VERTEX_POINT('',#58148);
#15735=VERTEX_POINT('',#58152);
#15736=VERTEX_POINT('',#58156);
#15737=VERTEX_POINT('',#58160);
#15738=VERTEX_POINT('',#58162);
#15739=VERTEX_POINT('',#58166);
#15740=VERTEX_POINT('',#58170);
#15741=VERTEX_POINT('',#58174);
#15742=VERTEX_POINT('',#58176);
#15743=VERTEX_POINT('',#58180);
#15744=VERTEX_POINT('',#58184);
#15745=VERTEX_POINT('',#58188);
#15746=VERTEX_POINT('',#58190);
#15747=VERTEX_POINT('',#58194);
#15748=VERTEX_POINT('',#58198);
#15749=VERTEX_POINT('',#58202);
#15750=VERTEX_POINT('',#58204);
#15751=VERTEX_POINT('',#58208);
#15752=VERTEX_POINT('',#58212);
#15753=VERTEX_POINT('',#58216);
#15754=VERTEX_POINT('',#58218);
#15755=VERTEX_POINT('',#58222);
#15756=VERTEX_POINT('',#58226);
#15757=VERTEX_POINT('',#58230);
#15758=VERTEX_POINT('',#58232);
#15759=VERTEX_POINT('',#58236);
#15760=VERTEX_POINT('',#58240);
#15761=VERTEX_POINT('',#58244);
#15762=VERTEX_POINT('',#58246);
#15763=VERTEX_POINT('',#58250);
#15764=VERTEX_POINT('',#58254);
#15765=VERTEX_POINT('',#58258);
#15766=VERTEX_POINT('',#58260);
#15767=VERTEX_POINT('',#58264);
#15768=VERTEX_POINT('',#58268);
#15769=VERTEX_POINT('',#58272);
#15770=VERTEX_POINT('',#58274);
#15771=VERTEX_POINT('',#58278);
#15772=VERTEX_POINT('',#58282);
#15773=VERTEX_POINT('',#58286);
#15774=VERTEX_POINT('',#58288);
#15775=VERTEX_POINT('',#58292);
#15776=VERTEX_POINT('',#58296);
#15777=VERTEX_POINT('',#58300);
#15778=VERTEX_POINT('',#58302);
#15779=VERTEX_POINT('',#58306);
#15780=VERTEX_POINT('',#58310);
#15781=VERTEX_POINT('',#58314);
#15782=VERTEX_POINT('',#58316);
#15783=VERTEX_POINT('',#58320);
#15784=VERTEX_POINT('',#58324);
#15785=VERTEX_POINT('',#58328);
#15786=VERTEX_POINT('',#58330);
#15787=VERTEX_POINT('',#58334);
#15788=VERTEX_POINT('',#58338);
#15789=VERTEX_POINT('',#58342);
#15790=VERTEX_POINT('',#58344);
#15791=VERTEX_POINT('',#58348);
#15792=VERTEX_POINT('',#58352);
#15793=VERTEX_POINT('',#58356);
#15794=VERTEX_POINT('',#58358);
#15795=VERTEX_POINT('',#58362);
#15796=VERTEX_POINT('',#58366);
#15797=VERTEX_POINT('',#58370);
#15798=VERTEX_POINT('',#58372);
#15799=VERTEX_POINT('',#58376);
#15800=VERTEX_POINT('',#58380);
#15801=VERTEX_POINT('',#58384);
#15802=VERTEX_POINT('',#58386);
#15803=VERTEX_POINT('',#58390);
#15804=VERTEX_POINT('',#58394);
#15805=VERTEX_POINT('',#58398);
#15806=VERTEX_POINT('',#58400);
#15807=VERTEX_POINT('',#58404);
#15808=VERTEX_POINT('',#58408);
#15809=VERTEX_POINT('',#58412);
#15810=VERTEX_POINT('',#58414);
#15811=VERTEX_POINT('',#58418);
#15812=VERTEX_POINT('',#58422);
#15813=VERTEX_POINT('',#58426);
#15814=VERTEX_POINT('',#58428);
#15815=VERTEX_POINT('',#58432);
#15816=VERTEX_POINT('',#58436);
#15817=VERTEX_POINT('',#58440);
#15818=VERTEX_POINT('',#58442);
#15819=VERTEX_POINT('',#58446);
#15820=VERTEX_POINT('',#58450);
#15821=VERTEX_POINT('',#58454);
#15822=VERTEX_POINT('',#58456);
#15823=VERTEX_POINT('',#58460);
#15824=VERTEX_POINT('',#58464);
#15825=VERTEX_POINT('',#58468);
#15826=VERTEX_POINT('',#58470);
#15827=VERTEX_POINT('',#58474);
#15828=VERTEX_POINT('',#58478);
#15829=VERTEX_POINT('',#58482);
#15830=VERTEX_POINT('',#58484);
#15831=VERTEX_POINT('',#58488);
#15832=VERTEX_POINT('',#58492);
#15833=VERTEX_POINT('',#58496);
#15834=VERTEX_POINT('',#58498);
#15835=VERTEX_POINT('',#58502);
#15836=VERTEX_POINT('',#58506);
#15837=VERTEX_POINT('',#58510);
#15838=VERTEX_POINT('',#58590);
#15839=VERTEX_POINT('',#58592);
#15840=VERTEX_POINT('',#58596);
#15841=VERTEX_POINT('',#58609);
#15842=VERTEX_POINT('',#58610);
#15843=VERTEX_POINT('',#58613);
#15844=VERTEX_POINT('',#58618);
#15845=VERTEX_POINT('',#58619);
#15846=VERTEX_POINT('',#58621);
#15847=VERTEX_POINT('',#58627);
#15848=VERTEX_POINT('',#58629);
#15849=VERTEX_POINT('',#58633);
#15850=VERTEX_POINT('',#58636);
#15851=VERTEX_POINT('',#58641);
#15852=VERTEX_POINT('',#58642);
#15853=VERTEX_POINT('',#58645);
#15854=VERTEX_POINT('',#58650);
#15855=VERTEX_POINT('',#58651);
#15856=VERTEX_POINT('',#58653);
#15857=VERTEX_POINT('',#58659);
#15858=VERTEX_POINT('',#58661);
#15859=VERTEX_POINT('',#58665);
#15860=VERTEX_POINT('',#58668);
#15861=VERTEX_POINT('',#58673);
#15862=VERTEX_POINT('',#58674);
#15863=VERTEX_POINT('',#58676);
#15864=VERTEX_POINT('',#58682);
#15865=VERTEX_POINT('',#58683);
#15866=VERTEX_POINT('',#58688);
#15867=VERTEX_POINT('',#58691);
#15868=VERTEX_POINT('',#58693);
#15869=VERTEX_POINT('',#58697);
#15870=VERTEX_POINT('',#58700);
#15871=VERTEX_POINT('',#58705);
#15872=VERTEX_POINT('',#58707);
#15873=VERTEX_POINT('',#58711);
#15874=VERTEX_POINT('',#58714);
#15875=VERTEX_POINT('',#58719);
#15876=VERTEX_POINT('',#58720);
#15877=VERTEX_POINT('',#58723);
#15878=VERTEX_POINT('',#58728);
#15879=VERTEX_POINT('',#58729);
#15880=VERTEX_POINT('',#58734);
#15881=VERTEX_POINT('',#58737);
#15882=VERTEX_POINT('',#58739);
#15883=VERTEX_POINT('',#58743);
#15884=VERTEX_POINT('',#58746);
#15885=VERTEX_POINT('',#58751);
#15886=VERTEX_POINT('',#58752);
#15887=VERTEX_POINT('',#58755);
#15888=VERTEX_POINT('',#58760);
#15889=VERTEX_POINT('',#58761);
#15890=VERTEX_POINT('',#58766);
#15891=VERTEX_POINT('',#58769);
#15892=VERTEX_POINT('',#58770);
#15893=VERTEX_POINT('',#58772);
#15894=VERTEX_POINT('',#58774);
#15895=VERTEX_POINT('',#58776);
#15896=VERTEX_POINT('',#58778);
#15897=VERTEX_POINT('',#58782);
#15898=VERTEX_POINT('',#58784);
#15899=VERTEX_POINT('',#58786);
#15900=VERTEX_POINT('',#58788);
#15901=VERTEX_POINT('',#58790);
#15902=VERTEX_POINT('',#58792);
#15903=VERTEX_POINT('',#58794);
#15904=VERTEX_POINT('',#58796);
#15905=VERTEX_POINT('',#58798);
#15906=VERTEX_POINT('',#58800);
#15907=VERTEX_POINT('',#58806);
#15908=VERTEX_POINT('',#58807);
#15909=VERTEX_POINT('',#58809);
#15910=VERTEX_POINT('',#58811);
#15911=VERTEX_POINT('',#58815);
#15912=VERTEX_POINT('',#58817);
#15913=VERTEX_POINT('',#58821);
#15914=VERTEX_POINT('',#58822);
#15915=VERTEX_POINT('',#58824);
#15916=VERTEX_POINT('',#58826);
#15917=VERTEX_POINT('',#58830);
#15918=VERTEX_POINT('',#58832);
#15919=VERTEX_POINT('',#58834);
#15920=VERTEX_POINT('',#58836);
#15921=VERTEX_POINT('',#58840);
#15922=VERTEX_POINT('',#58843);
#15923=VERTEX_POINT('',#58847);
#15924=VERTEX_POINT('',#58849);
#15925=VERTEX_POINT('',#58854);
#15926=VERTEX_POINT('',#58856);
#15927=VERTEX_POINT('',#58858);
#15928=VERTEX_POINT('',#58860);
#15929=VERTEX_POINT('',#58862);
#15930=VERTEX_POINT('',#58866);
#15931=VERTEX_POINT('',#58870);
#15932=VERTEX_POINT('',#58872);
#15933=VERTEX_POINT('',#58874);
#15934=VERTEX_POINT('',#58876);
#15935=VERTEX_POINT('',#58879);
#15936=VERTEX_POINT('',#58881);
#15937=VERTEX_POINT('',#58883);
#15938=VERTEX_POINT('',#58885);
#15939=VERTEX_POINT('',#58888);
#15940=VERTEX_POINT('',#58891);
#15941=VERTEX_POINT('',#58893);
#15942=VERTEX_POINT('',#58895);
#15943=VERTEX_POINT('',#58902);
#15944=VERTEX_POINT('',#58904);
#15945=VERTEX_POINT('',#58906);
#15946=VERTEX_POINT('',#58908);
#15947=VERTEX_POINT('',#58910);
#15948=VERTEX_POINT('',#58913);
#15949=VERTEX_POINT('',#58915);
#15950=VERTEX_POINT('',#58917);
#15951=VERTEX_POINT('',#58920);
#15952=VERTEX_POINT('',#58922);
#15953=VERTEX_POINT('',#58926);
#15954=VERTEX_POINT('',#58930);
#15955=VERTEX_POINT('',#58932);
#15956=VERTEX_POINT('',#58934);
#15957=VERTEX_POINT('',#58936);
#15958=VERTEX_POINT('',#58938);
#15959=VERTEX_POINT('',#58940);
#15960=VERTEX_POINT('',#58942);
#15961=VERTEX_POINT('',#58944);
#15962=VERTEX_POINT('',#58946);
#15963=VERTEX_POINT('',#58950);
#15964=VERTEX_POINT('',#58952);
#15965=VERTEX_POINT('',#58956);
#15966=VERTEX_POINT('',#58960);
#15967=VERTEX_POINT('',#58964);
#15968=VERTEX_POINT('',#58966);
#15969=VERTEX_POINT('',#58970);
#15970=VERTEX_POINT('',#58972);
#15971=VERTEX_POINT('',#58974);
#15972=VERTEX_POINT('',#58980);
#15973=VERTEX_POINT('',#58982);
#15974=VERTEX_POINT('',#58984);
#15975=VERTEX_POINT('',#58986);
#15976=VERTEX_POINT('',#58991);
#15977=VERTEX_POINT('',#58993);
#15978=VERTEX_POINT('',#58995);
#15979=VERTEX_POINT('',#58997);
#15980=VERTEX_POINT('',#58999);
#15981=VERTEX_POINT('',#59001);
#15982=VERTEX_POINT('',#59008);
#15983=VERTEX_POINT('',#59009);
#15984=VERTEX_POINT('',#59011);
#15985=VERTEX_POINT('',#59013);
#15986=VERTEX_POINT('',#59016);
#15987=VERTEX_POINT('',#59018);
#15988=VERTEX_POINT('',#59020);
#15989=VERTEX_POINT('',#59022);
#15990=VERTEX_POINT('',#59026);
#15991=VERTEX_POINT('',#59027);
#15992=VERTEX_POINT('',#59029);
#15993=VERTEX_POINT('',#59032);
#15994=VERTEX_POINT('',#59034);
#15995=VERTEX_POINT('',#59036);
#15996=VERTEX_POINT('',#59038);
#15997=VERTEX_POINT('',#59042);
#15998=VERTEX_POINT('',#59048);
#15999=VERTEX_POINT('',#59049);
#16000=VERTEX_POINT('',#59051);
#16001=VERTEX_POINT('',#59053);
#16002=VERTEX_POINT('',#59057);
#16003=VERTEX_POINT('',#59059);
#16004=VERTEX_POINT('',#59063);
#16005=VERTEX_POINT('',#59065);
#16006=VERTEX_POINT('',#59071);
#16007=VERTEX_POINT('',#59075);
#16008=VERTEX_POINT('',#59082);
#16009=VERTEX_POINT('',#59085);
#16010=VERTEX_POINT('',#59086);
#16011=VERTEX_POINT('',#59089);
#16012=VERTEX_POINT('',#59093);
#16013=VERTEX_POINT('',#59094);
#16014=VERTEX_POINT('',#59097);
#16015=VERTEX_POINT('',#59101);
#16016=VERTEX_POINT('',#59102);
#16017=VERTEX_POINT('',#59105);
#16018=VERTEX_POINT('',#59109);
#16019=VERTEX_POINT('',#59110);
#16020=VERTEX_POINT('',#59113);
#16021=VERTEX_POINT('',#59118);
#16022=VERTEX_POINT('',#59120);
#16023=VERTEX_POINT('',#59122);
#16024=VERTEX_POINT('',#59128);
#16025=VERTEX_POINT('',#59130);
#16026=VERTEX_POINT('',#59135);
#16027=VERTEX_POINT('',#59138);
#16028=VERTEX_POINT('',#59140);
#16029=VERTEX_POINT('',#59144);
#16030=VERTEX_POINT('',#59145);
#16031=VERTEX_POINT('',#59147);
#16032=VERTEX_POINT('',#59149);
#16033=VERTEX_POINT('',#59153);
#16034=VERTEX_POINT('',#59155);
#16035=VERTEX_POINT('',#59160);
#16036=VERTEX_POINT('',#59161);
#16037=VERTEX_POINT('',#59165);
#16038=VERTEX_POINT('',#59167);
#16039=VERTEX_POINT('',#59171);
#16040=VERTEX_POINT('',#59173);
#16041=VERTEX_POINT('',#59177);
#16042=VERTEX_POINT('',#59178);
#16043=VERTEX_POINT('',#59182);
#16044=VERTEX_POINT('',#59187);
#16045=VERTEX_POINT('',#59191);
#16046=VERTEX_POINT('',#59192);
#16047=VERTEX_POINT('',#59196);
#16048=VERTEX_POINT('',#59201);
#16049=VERTEX_POINT('',#59205);
#16050=VERTEX_POINT('',#59206);
#16051=VERTEX_POINT('',#59210);
#16052=VERTEX_POINT('',#59215);
#16053=VERTEX_POINT('',#59219);
#16054=VERTEX_POINT('',#59227);
#16055=VERTEX_POINT('',#59228);
#16056=VERTEX_POINT('',#59232);
#16057=VERTEX_POINT('',#59238);
#16058=VERTEX_POINT('',#59247);
#16059=VERTEX_POINT('',#59257);
#16060=VERTEX_POINT('',#59258);
#16061=VERTEX_POINT('',#59262);
#16062=VERTEX_POINT('',#59264);
#16063=VERTEX_POINT('',#59268);
#16064=VERTEX_POINT('',#59270);
#16065=VERTEX_POINT('',#59274);
#16066=VERTEX_POINT('',#59275);
#16067=VERTEX_POINT('',#59279);
#16068=VERTEX_POINT('',#59284);
#16069=VERTEX_POINT('',#59288);
#16070=VERTEX_POINT('',#59289);
#16071=VERTEX_POINT('',#59293);
#16072=VERTEX_POINT('',#59298);
#16073=VERTEX_POINT('',#59302);
#16074=VERTEX_POINT('',#59303);
#16075=VERTEX_POINT('',#59307);
#16076=VERTEX_POINT('',#59312);
#16077=VERTEX_POINT('',#59316);
#16078=VERTEX_POINT('',#59324);
#16079=VERTEX_POINT('',#59325);
#16080=VERTEX_POINT('',#59329);
#16081=VERTEX_POINT('',#59335);
#16082=VERTEX_POINT('',#59344);
#16083=VERTEX_POINT('',#59354);
#16084=VERTEX_POINT('',#59358);
#16085=VERTEX_POINT('',#59360);
#16086=VERTEX_POINT('',#59364);
#16087=VERTEX_POINT('',#59368);
#16088=VERTEX_POINT('',#59372);
#16089=VERTEX_POINT('',#59376);
#16090=VERTEX_POINT('',#59393);
#16091=VERTEX_POINT('',#59394);
#16092=VERTEX_POINT('',#59396);
#16093=VERTEX_POINT('',#59398);
#16094=VERTEX_POINT('',#59400);
#16095=VERTEX_POINT('',#59402);
#16096=VERTEX_POINT('',#59406);
#16097=VERTEX_POINT('',#59407);
#16098=VERTEX_POINT('',#59412);
#16099=VERTEX_POINT('',#59416);
#16100=VERTEX_POINT('',#59420);
#16101=VERTEX_POINT('',#59424);
#16102=VERTEX_POINT('',#59433);
#16103=VERTEX_POINT('',#59434);
#16104=VERTEX_POINT('',#59436);
#16105=VERTEX_POINT('',#59438);
#16106=VERTEX_POINT('',#59440);
#16107=VERTEX_POINT('',#59442);
#16108=VERTEX_POINT('',#59446);
#16109=VERTEX_POINT('',#59447);
#16110=VERTEX_POINT('',#59452);
#16111=VERTEX_POINT('',#59456);
#16112=VERTEX_POINT('',#59460);
#16113=VERTEX_POINT('',#59464);
#16114=VERTEX_POINT('',#59473);
#16115=VERTEX_POINT('',#59477);
#16116=VERTEX_POINT('',#59483);
#16117=VERTEX_POINT('',#59488);
#16118=VERTEX_POINT('',#59489);
#16119=VERTEX_POINT('',#59491);
#16120=VERTEX_POINT('',#59495);
#16121=VERTEX_POINT('',#59497);
#16122=VERTEX_POINT('',#59501);
#16123=VERTEX_POINT('',#59505);
#16124=VERTEX_POINT('',#59506);
#16125=VERTEX_POINT('',#59508);
#16126=VERTEX_POINT('',#59512);
#16127=VERTEX_POINT('',#59514);
#16128=VERTEX_POINT('',#59518);
#16129=VERTEX_POINT('',#59522);
#16130=VERTEX_POINT('',#59523);
#16131=VERTEX_POINT('',#59525);
#16132=VERTEX_POINT('',#59529);
#16133=VERTEX_POINT('',#59531);
#16134=VERTEX_POINT('',#59535);
#16135=VERTEX_POINT('',#59539);
#16136=VERTEX_POINT('',#59540);
#16137=VERTEX_POINT('',#59543);
#16138=VERTEX_POINT('',#59547);
#16139=VERTEX_POINT('',#59549);
#16140=VERTEX_POINT('',#59553);
#16141=VERTEX_POINT('',#59556);
#16142=VERTEX_POINT('',#59557);
#16143=VERTEX_POINT('',#59560);
#16144=VERTEX_POINT('',#59564);
#16145=VERTEX_POINT('',#59566);
#16146=VERTEX_POINT('',#59570);
#16147=VERTEX_POINT('',#59573);
#16148=VERTEX_POINT('',#59574);
#16149=VERTEX_POINT('',#59577);
#16150=VERTEX_POINT('',#59581);
#16151=VERTEX_POINT('',#59583);
#16152=VERTEX_POINT('',#59587);
#16153=VERTEX_POINT('',#59590);
#16154=VERTEX_POINT('',#59591);
#16155=VERTEX_POINT('',#59594);
#16156=VERTEX_POINT('',#59598);
#16157=VERTEX_POINT('',#59600);
#16158=VERTEX_POINT('',#59604);
#16159=VERTEX_POINT('',#59607);
#16160=VERTEX_POINT('',#59610);
#16161=VERTEX_POINT('',#59613);
#16162=VERTEX_POINT('',#59616);
#16163=VERTEX_POINT('',#59619);
#16164=VERTEX_POINT('',#59622);
#16165=VERTEX_POINT('',#59625);
#16166=VERTEX_POINT('',#59628);
#16167=VERTEX_POINT('',#59631);
#16168=VERTEX_POINT('',#59633);
#16169=VERTEX_POINT('',#59637);
#16170=VERTEX_POINT('',#59641);
#16171=VERTEX_POINT('',#59643);
#16172=VERTEX_POINT('',#59647);
#16173=VERTEX_POINT('',#59651);
#16174=VERTEX_POINT('',#59655);
#16175=VERTEX_POINT('',#59659);
#16176=VERTEX_POINT('',#59665);
#16177=VERTEX_POINT('',#59668);
#16178=VERTEX_POINT('',#59669);
#16179=VERTEX_POINT('',#59671);
#16180=VERTEX_POINT('',#59673);
#16181=VERTEX_POINT('',#59675);
#16182=VERTEX_POINT('',#59677);
#16183=VERTEX_POINT('',#59679);
#16184=VERTEX_POINT('',#59681);
#16185=VERTEX_POINT('',#59685);
#16186=VERTEX_POINT('',#59687);
#16187=VERTEX_POINT('',#59690);
#16188=VERTEX_POINT('',#59694);
#16189=VERTEX_POINT('',#59695);
#16190=VERTEX_POINT('',#59697);
#16191=VERTEX_POINT('',#59705);
#16192=VERTEX_POINT('',#59709);
#16193=VERTEX_POINT('',#59713);
#16194=VERTEX_POINT('',#59717);
#16195=VERTEX_POINT('',#59721);
#16196=VERTEX_POINT('',#59732);
#16197=VERTEX_POINT('',#59733);
#16198=VERTEX_POINT('',#59736);
#16199=VERTEX_POINT('',#59740);
#16200=VERTEX_POINT('',#59742);
#16201=VERTEX_POINT('',#59751);
#16202=VERTEX_POINT('',#59820);
#16203=VERTEX_POINT('',#59829);
#16204=VERTEX_POINT('',#59831);
#16205=VERTEX_POINT('',#59835);
#16206=VERTEX_POINT('',#59836);
#16207=VERTEX_POINT('',#59839);
#16208=VERTEX_POINT('',#59843);
#16209=VERTEX_POINT('',#59844);
#16210=VERTEX_POINT('',#59846);
#16211=VERTEX_POINT('',#59848);
#16212=VERTEX_POINT('',#59850);
#16213=VERTEX_POINT('',#59852);
#16214=VERTEX_POINT('',#59855);
#16215=VERTEX_POINT('',#59856);
#16216=VERTEX_POINT('',#59858);
#16217=VERTEX_POINT('',#59860);
#16218=VERTEX_POINT('',#59862);
#16219=VERTEX_POINT('',#59864);
#16220=VERTEX_POINT('',#59868);
#16221=VERTEX_POINT('',#59871);
#16222=VERTEX_POINT('',#59876);
#16223=VERTEX_POINT('',#59877);
#16224=VERTEX_POINT('',#59880);
#16225=VERTEX_POINT('',#59884);
#16226=VERTEX_POINT('',#59885);
#16227=VERTEX_POINT('',#59888);
#16228=VERTEX_POINT('',#59892);
#16229=VERTEX_POINT('',#59893);
#16230=VERTEX_POINT('',#59895);
#16231=VERTEX_POINT('',#59897);
#16232=VERTEX_POINT('',#59901);
#16233=VERTEX_POINT('',#59902);
#16234=VERTEX_POINT('',#59913);
#16235=VERTEX_POINT('',#59916);
#16236=VERTEX_POINT('',#59918);
#16237=VERTEX_POINT('',#59921);
#16238=VERTEX_POINT('',#59956);
#16239=VERTEX_POINT('',#59992);
#16240=VERTEX_POINT('',#59993);
#16241=VERTEX_POINT('',#59996);
#16242=VERTEX_POINT('',#60003);
#16243=VERTEX_POINT('',#60004);
#16244=VERTEX_POINT('',#60006);
#16245=VERTEX_POINT('',#60008);
#16246=VERTEX_POINT('',#60010);
#16247=VERTEX_POINT('',#60012);
#16248=VERTEX_POINT('',#60016);
#16249=VERTEX_POINT('',#60017);
#16250=VERTEX_POINT('',#60022);
#16251=VERTEX_POINT('',#60026);
#16252=VERTEX_POINT('',#60030);
#16253=VERTEX_POINT('',#60034);
#16254=VERTEX_POINT('',#60040);
#16255=VERTEX_POINT('',#60041);
#16256=VERTEX_POINT('',#60043);
#16257=VERTEX_POINT('',#60045);
#16258=VERTEX_POINT('',#60047);
#16259=VERTEX_POINT('',#60049);
#16260=VERTEX_POINT('',#60053);
#16261=VERTEX_POINT('',#60054);
#16262=VERTEX_POINT('',#60059);
#16263=VERTEX_POINT('',#60063);
#16264=VERTEX_POINT('',#60067);
#16265=VERTEX_POINT('',#60071);
#16266=VERTEX_POINT('',#60077);
#16267=VERTEX_POINT('',#60080);
#16268=VERTEX_POINT('',#60081);
#16269=VERTEX_POINT('',#60086);
#16270=VERTEX_POINT('',#60123);
#16271=VERTEX_POINT('',#60124);
#16272=VERTEX_POINT('',#60127);
#16273=VERTEX_POINT('',#60132);
#16274=VERTEX_POINT('',#60135);
#16275=VERTEX_POINT('',#60136);
#16276=VERTEX_POINT('',#60141);
#16277=VERTEX_POINT('',#60142);
#16278=VERTEX_POINT('',#60144);
#16279=VERTEX_POINT('',#60146);
#16280=VERTEX_POINT('',#60148);
#16281=VERTEX_POINT('',#60150);
#16282=VERTEX_POINT('',#60154);
#16283=VERTEX_POINT('',#60155);
#16284=VERTEX_POINT('',#60160);
#16285=VERTEX_POINT('',#60164);
#16286=VERTEX_POINT('',#60168);
#16287=VERTEX_POINT('',#60172);
#16288=VERTEX_POINT('',#60178);
#16289=VERTEX_POINT('',#60179);
#16290=VERTEX_POINT('',#60181);
#16291=VERTEX_POINT('',#60183);
#16292=VERTEX_POINT('',#60185);
#16293=VERTEX_POINT('',#60187);
#16294=VERTEX_POINT('',#60191);
#16295=VERTEX_POINT('',#60192);
#16296=VERTEX_POINT('',#60197);
#16297=VERTEX_POINT('',#60201);
#16298=VERTEX_POINT('',#60205);
#16299=VERTEX_POINT('',#60209);
#16300=VERTEX_POINT('',#60215);
#16301=VERTEX_POINT('',#60218);
#16302=VERTEX_POINT('',#60219);
#16303=VERTEX_POINT('',#60224);
#16304=VERTEX_POINT('',#60261);
#16305=VERTEX_POINT('',#60262);
#16306=VERTEX_POINT('',#60265);
#16307=VERTEX_POINT('',#60270);
#16308=VERTEX_POINT('',#60273);
#16309=VERTEX_POINT('',#60274);
#16310=VERTEX_POINT('',#60279);
#16311=VERTEX_POINT('',#60316);
#16312=VERTEX_POINT('',#60325);
#16313=VERTEX_POINT('',#60330);
#16314=VERTEX_POINT('',#60367);
#16315=VERTEX_POINT('',#60368);
#16316=VERTEX_POINT('',#60371);
#16317=VERTEX_POINT('',#60388);
#16318=VERTEX_POINT('',#60392);
#16319=VERTEX_POINT('',#60395);
#16320=VERTEX_POINT('',#60400);
#16321=VERTEX_POINT('',#60405);
#16322=VERTEX_POINT('',#60410);
#16323=VERTEX_POINT('',#60411);
#16324=VERTEX_POINT('',#60413);
#16325=VERTEX_POINT('',#60415);
#16326=VERTEX_POINT('',#60417);
#16327=VERTEX_POINT('',#60419);
#16328=VERTEX_POINT('',#60421);
#16329=VERTEX_POINT('',#60423);
#16330=VERTEX_POINT('',#60425);
#16331=VERTEX_POINT('',#60427);
#16332=VERTEX_POINT('',#60429);
#16333=VERTEX_POINT('',#60431);
#16334=VERTEX_POINT('',#60435);
#16335=VERTEX_POINT('',#60443);
#16336=VERTEX_POINT('',#60447);
#16337=VERTEX_POINT('',#60454);
#16338=VERTEX_POINT('',#60463);
#16339=VERTEX_POINT('',#60476);
#16340=VERTEX_POINT('',#60495);
#16341=VERTEX_POINT('',#60496);
#16342=VERTEX_POINT('',#60498);
#16343=VERTEX_POINT('',#60500);
#16344=VERTEX_POINT('',#60502);
#16345=VERTEX_POINT('',#60504);
#16346=VERTEX_POINT('',#60506);
#16347=VERTEX_POINT('',#60508);
#16348=VERTEX_POINT('',#60510);
#16349=VERTEX_POINT('',#60512);
#16350=VERTEX_POINT('',#60514);
#16351=VERTEX_POINT('',#60516);
#16352=VERTEX_POINT('',#60520);
#16353=VERTEX_POINT('',#60528);
#16354=VERTEX_POINT('',#60532);
#16355=VERTEX_POINT('',#60539);
#16356=VERTEX_POINT('',#60548);
#16357=VERTEX_POINT('',#60561);
#16358=VERTEX_POINT('',#60580);
#16359=VERTEX_POINT('',#60583);
#16360=VERTEX_POINT('',#60586);
#16361=VERTEX_POINT('',#60589);
#16362=VERTEX_POINT('',#60591);
#16363=VERTEX_POINT('',#60595);
#16364=VERTEX_POINT('',#60597);
#16365=VERTEX_POINT('',#60601);
#16366=VERTEX_POINT('',#60605);
#16367=VERTEX_POINT('',#60607);
#16368=VERTEX_POINT('',#60611);
#16369=VERTEX_POINT('',#60613);
#16370=VERTEX_POINT('',#60617);
#16371=VERTEX_POINT('',#60619);
#16372=VERTEX_POINT('',#60623);
#16373=VERTEX_POINT('',#60625);
#16374=VERTEX_POINT('',#60629);
#16375=VERTEX_POINT('',#60630);
#16376=VERTEX_POINT('',#60632);
#16377=VERTEX_POINT('',#60634);
#16378=VERTEX_POINT('',#60636);
#16379=VERTEX_POINT('',#60638);
#16380=VERTEX_POINT('',#60640);
#16381=VERTEX_POINT('',#60642);
#16382=VERTEX_POINT('',#60646);
#16383=VERTEX_POINT('',#60647);
#16384=VERTEX_POINT('',#60649);
#16385=VERTEX_POINT('',#60651);
#16386=VERTEX_POINT('',#60655);
#16387=VERTEX_POINT('',#60657);
#16388=VERTEX_POINT('',#60661);
#16389=VERTEX_POINT('',#60663);
#16390=VERTEX_POINT('',#60667);
#16391=VERTEX_POINT('',#60669);
#16392=VERTEX_POINT('',#60673);
#16393=VERTEX_POINT('',#60675);
#16394=VERTEX_POINT('',#60679);
#16395=VERTEX_POINT('',#60681);
#16396=VERTEX_POINT('',#60685);
#16397=VERTEX_POINT('',#60687);
#16398=VERTEX_POINT('',#60695);
#16399=VERTEX_POINT('',#60696);
#16400=VERTEX_POINT('',#60698);
#16401=VERTEX_POINT('',#60700);
#16402=VERTEX_POINT('',#60704);
#16403=VERTEX_POINT('',#60706);
#16404=VERTEX_POINT('',#60710);
#16405=VERTEX_POINT('',#60712);
#16406=VERTEX_POINT('',#60716);
#16407=VERTEX_POINT('',#60718);
#16408=VERTEX_POINT('',#60722);
#16409=VERTEX_POINT('',#60724);
#16410=VERTEX_POINT('',#60728);
#16411=VERTEX_POINT('',#60730);
#16412=VERTEX_POINT('',#60734);
#16413=VERTEX_POINT('',#60736);
#16414=VERTEX_POINT('',#60744);
#16415=VERTEX_POINT('',#60745);
#16416=VERTEX_POINT('',#60747);
#16417=VERTEX_POINT('',#60749);
#16418=VERTEX_POINT('',#60753);
#16419=VERTEX_POINT('',#60755);
#16420=VERTEX_POINT('',#60759);
#16421=VERTEX_POINT('',#60761);
#16422=VERTEX_POINT('',#60765);
#16423=VERTEX_POINT('',#60767);
#16424=VERTEX_POINT('',#60771);
#16425=VERTEX_POINT('',#60773);
#16426=VERTEX_POINT('',#60777);
#16427=VERTEX_POINT('',#60779);
#16428=VERTEX_POINT('',#60783);
#16429=VERTEX_POINT('',#60785);
#16430=VERTEX_POINT('',#60793);
#16431=VERTEX_POINT('',#60797);
#16432=VERTEX_POINT('',#60801);
#16433=VERTEX_POINT('',#60805);
#16434=VERTEX_POINT('',#60806);
#16435=VERTEX_POINT('',#60808);
#16436=VERTEX_POINT('',#60810);
#16437=VERTEX_POINT('',#60816);
#16438=VERTEX_POINT('',#60817);
#16439=VERTEX_POINT('',#60819);
#16440=VERTEX_POINT('',#60821);
#16441=VERTEX_POINT('',#60827);
#16442=VERTEX_POINT('',#60828);
#16443=VERTEX_POINT('',#60830);
#16444=VERTEX_POINT('',#60832);
#16445=VERTEX_POINT('',#60838);
#16446=VERTEX_POINT('',#60839);
#16447=VERTEX_POINT('',#60841);
#16448=VERTEX_POINT('',#60843);
#16449=VERTEX_POINT('',#60845);
#16450=VERTEX_POINT('',#60847);
#16451=VERTEX_POINT('',#60851);
#16452=VERTEX_POINT('',#60852);
#16453=VERTEX_POINT('',#60854);
#16454=VERTEX_POINT('',#60856);
#16455=VERTEX_POINT('',#60858);
#16456=VERTEX_POINT('',#60860);
#16457=VERTEX_POINT('',#60864);
#16458=VERTEX_POINT('',#60865);
#16459=VERTEX_POINT('',#60867);
#16460=VERTEX_POINT('',#60869);
#16461=VERTEX_POINT('',#60871);
#16462=VERTEX_POINT('',#60873);
#16463=VERTEX_POINT('',#60876);
#16464=VERTEX_POINT('',#60879);
#16465=VERTEX_POINT('',#60881);
#16466=VERTEX_POINT('',#60883);
#16467=VERTEX_POINT('',#60887);
#16468=VERTEX_POINT('',#60889);
#16469=VERTEX_POINT('',#60893);
#16470=VERTEX_POINT('',#60895);
#16471=VERTEX_POINT('',#60899);
#16472=VERTEX_POINT('',#60901);
#16473=VERTEX_POINT('',#60905);
#16474=VERTEX_POINT('',#60907);
#16475=VERTEX_POINT('',#60911);
#16476=VERTEX_POINT('',#60913);
#16477=VERTEX_POINT('',#60916);
#16478=VERTEX_POINT('',#60918);
#16479=VERTEX_POINT('',#60923);
#16480=VERTEX_POINT('',#60927);
#16481=VERTEX_POINT('',#60930);
#16482=VERTEX_POINT('',#60932);
#16483=VERTEX_POINT('',#60937);
#16484=VERTEX_POINT('',#60941);
#16485=VERTEX_POINT('',#60944);
#16486=VERTEX_POINT('',#60946);
#16487=VERTEX_POINT('',#60948);
#16488=VERTEX_POINT('',#60950);
#16489=VERTEX_POINT('',#60954);
#16490=VERTEX_POINT('',#60956);
#16491=VERTEX_POINT('',#60960);
#16492=VERTEX_POINT('',#60961);
#16493=VERTEX_POINT('',#60963);
#16494=VERTEX_POINT('',#60965);
#16495=VERTEX_POINT('',#60967);
#16496=VERTEX_POINT('',#60970);
#16497=VERTEX_POINT('',#60972);
#16498=VERTEX_POINT('',#60974);
#16499=VERTEX_POINT('',#60981);
#16500=VERTEX_POINT('',#60983);
#16501=VERTEX_POINT('',#60985);
#16502=VERTEX_POINT('',#60988);
#16503=VERTEX_POINT('',#60990);
#16504=VERTEX_POINT('',#60993);
#16505=VERTEX_POINT('',#60995);
#16506=VERTEX_POINT('',#60998);
#16507=VERTEX_POINT('',#61002);
#16508=VERTEX_POINT('',#61006);
#16509=VERTEX_POINT('',#61032);
#16510=VERTEX_POINT('',#61033);
#16511=VERTEX_POINT('',#61035);
#16512=VERTEX_POINT('',#61037);
#16513=VERTEX_POINT('',#61041);
#16514=VERTEX_POINT('',#61043);
#16515=VERTEX_POINT('',#61047);
#16516=VERTEX_POINT('',#61049);
#16517=VERTEX_POINT('',#61053);
#16518=VERTEX_POINT('',#61055);
#16519=VERTEX_POINT('',#61059);
#16520=VERTEX_POINT('',#61061);
#16521=VERTEX_POINT('',#61065);
#16522=VERTEX_POINT('',#61067);
#16523=VERTEX_POINT('',#61071);
#16524=VERTEX_POINT('',#61073);
#16525=VERTEX_POINT('',#61081);
#16526=VERTEX_POINT('',#61082);
#16527=VERTEX_POINT('',#61084);
#16528=VERTEX_POINT('',#61086);
#16529=VERTEX_POINT('',#61090);
#16530=VERTEX_POINT('',#61092);
#16531=VERTEX_POINT('',#61096);
#16532=VERTEX_POINT('',#61098);
#16533=VERTEX_POINT('',#61102);
#16534=VERTEX_POINT('',#61104);
#16535=VERTEX_POINT('',#61108);
#16536=VERTEX_POINT('',#61110);
#16537=VERTEX_POINT('',#61114);
#16538=VERTEX_POINT('',#61116);
#16539=VERTEX_POINT('',#61120);
#16540=VERTEX_POINT('',#61122);
#16541=VERTEX_POINT('',#61130);
#16542=VERTEX_POINT('',#61131);
#16543=VERTEX_POINT('',#61133);
#16544=VERTEX_POINT('',#61135);
#16545=VERTEX_POINT('',#61139);
#16546=VERTEX_POINT('',#61141);
#16547=VERTEX_POINT('',#61145);
#16548=VERTEX_POINT('',#61147);
#16549=VERTEX_POINT('',#61151);
#16550=VERTEX_POINT('',#61153);
#16551=VERTEX_POINT('',#61157);
#16552=VERTEX_POINT('',#61159);
#16553=VERTEX_POINT('',#61163);
#16554=VERTEX_POINT('',#61165);
#16555=VERTEX_POINT('',#61169);
#16556=VERTEX_POINT('',#61171);
#16557=VERTEX_POINT('',#61179);
#16558=VERTEX_POINT('',#61180);
#16559=VERTEX_POINT('',#61182);
#16560=VERTEX_POINT('',#61184);
#16561=VERTEX_POINT('',#61188);
#16562=VERTEX_POINT('',#61190);
#16563=VERTEX_POINT('',#61194);
#16564=VERTEX_POINT('',#61196);
#16565=VERTEX_POINT('',#61200);
#16566=VERTEX_POINT('',#61202);
#16567=VERTEX_POINT('',#61206);
#16568=VERTEX_POINT('',#61208);
#16569=VERTEX_POINT('',#61212);
#16570=VERTEX_POINT('',#61214);
#16571=VERTEX_POINT('',#61218);
#16572=VERTEX_POINT('',#61220);
#16573=VERTEX_POINT('',#61228);
#16574=VERTEX_POINT('',#61229);
#16575=VERTEX_POINT('',#61234);
#16576=VERTEX_POINT('',#61238);
#16577=VERTEX_POINT('',#61242);
#16578=VERTEX_POINT('',#61246);
#16579=VERTEX_POINT('',#61250);
#16580=VERTEX_POINT('',#61254);
#16581=VERTEX_POINT('',#61260);
#16582=VERTEX_POINT('',#61264);
#16583=VERTEX_POINT('',#61265);
#16584=VERTEX_POINT('',#61267);
#16585=VERTEX_POINT('',#61269);
#16586=VERTEX_POINT('',#61271);
#16587=VERTEX_POINT('',#61273);
#16588=VERTEX_POINT('',#61275);
#16589=VERTEX_POINT('',#61277);
#16590=VERTEX_POINT('',#61299);
#16591=VERTEX_POINT('',#61300);
#16592=VERTEX_POINT('',#61303);
#16593=VERTEX_POINT('',#61307);
#16594=VERTEX_POINT('',#61309);
#16595=VERTEX_POINT('',#61315);
#16596=VERTEX_POINT('',#61316);
#16597=VERTEX_POINT('',#61318);
#16598=VERTEX_POINT('',#61320);
#16599=VERTEX_POINT('',#61324);
#16600=VERTEX_POINT('',#61326);
#16601=VERTEX_POINT('',#61330);
#16602=VERTEX_POINT('',#61332);
#16603=VERTEX_POINT('',#61336);
#16604=VERTEX_POINT('',#61338);
#16605=VERTEX_POINT('',#61342);
#16606=VERTEX_POINT('',#61344);
#16607=VERTEX_POINT('',#61354);
#16608=VERTEX_POINT('',#61356);
#16609=VERTEX_POINT('',#61359);
#16610=VERTEX_POINT('',#61394);
#16611=VERTEX_POINT('',#61430);
#16612=VERTEX_POINT('',#61465);
#16613=VERTEX_POINT('',#61502);
#16614=VERTEX_POINT('',#61537);
#16615=VERTEX_POINT('',#61574);
#16616=VERTEX_POINT('',#61576);
#16617=VERTEX_POINT('',#61614);
#16618=VERTEX_POINT('',#61616);
#16619=VERTEX_POINT('',#61654);
#16620=VERTEX_POINT('',#61657);
#16621=VERTEX_POINT('',#61661);
#16622=VERTEX_POINT('',#61662);
#16623=VERTEX_POINT('',#61665);
#16624=VERTEX_POINT('',#61667);
#16625=VERTEX_POINT('',#61671);
#16626=VERTEX_POINT('',#61676);
#16627=VERTEX_POINT('',#61677);
#16628=VERTEX_POINT('',#61680);
#16629=VERTEX_POINT('',#61684);
#16630=VERTEX_POINT('',#61686);
#16631=EDGE_CURVE('',#13440,#13441,#8346,.T.);
#16632=EDGE_CURVE('',#13440,#13442,#8347,.T.);
#16633=EDGE_CURVE('',#13443,#13442,#8348,.T.);
#16634=EDGE_CURVE('',#13441,#13443,#8349,.T.);
#16635=EDGE_CURVE('',#13444,#13445,#8350,.T.);
#16636=EDGE_CURVE('',#13446,#13444,#8351,.T.);
#16637=EDGE_CURVE('',#13447,#13446,#8352,.T.);
#16638=EDGE_CURVE('',#13445,#13447,#8353,.T.);
#16639=EDGE_CURVE('',#13445,#13440,#8354,.T.);
#16640=EDGE_CURVE('',#13442,#13447,#8355,.T.);
#16641=EDGE_CURVE('',#13448,#13449,#8356,.T.);
#16642=EDGE_CURVE('',#13449,#13450,#8357,.T.);
#16643=EDGE_CURVE('',#13450,#13451,#2236,.T.);
#16644=EDGE_CURVE('',#13451,#13452,#8358,.T.);
#16645=EDGE_CURVE('',#13453,#13452,#2237,.T.);
#16646=EDGE_CURVE('',#13453,#13454,#8359,.T.);
#16647=EDGE_CURVE('',#13454,#13455,#8360,.T.);
#16648=EDGE_CURVE('',#13455,#13456,#2238,.T.);
#16649=EDGE_CURVE('',#13456,#13457,#8361,.T.);
#16650=EDGE_CURVE('',#13458,#13457,#2239,.T.);
#16651=EDGE_CURVE('',#13458,#13459,#8362,.T.);
#16652=EDGE_CURVE('',#13459,#13460,#8363,.T.);
#16653=EDGE_CURVE('',#13460,#13461,#2240,.T.);
#16654=EDGE_CURVE('',#13461,#13462,#8364,.T.);
#16655=EDGE_CURVE('',#13448,#13462,#2241,.T.);
#16656=EDGE_CURVE('',#13446,#13443,#2242,.T.);
#16657=EDGE_CURVE('',#13441,#13444,#2243,.T.);
#16658=EDGE_CURVE('',#13452,#13463,#8365,.T.);
#16659=EDGE_CURVE('',#13451,#13464,#8366,.T.);
#16660=EDGE_CURVE('',#13463,#13464,#8367,.T.);
#16661=EDGE_CURVE('',#13450,#13465,#8368,.T.);
#16662=EDGE_CURVE('',#13464,#13465,#2244,.T.);
#16663=EDGE_CURVE('',#13449,#13466,#8369,.T.);
#16664=EDGE_CURVE('',#13465,#13466,#8370,.T.);
#16665=EDGE_CURVE('',#13467,#13448,#8371,.T.);
#16666=EDGE_CURVE('',#13466,#13467,#8372,.T.);
#16667=EDGE_CURVE('',#13457,#13468,#8373,.T.);
#16668=EDGE_CURVE('',#13456,#13469,#8374,.T.);
#16669=EDGE_CURVE('',#13468,#13469,#8375,.T.);
#16670=EDGE_CURVE('',#13455,#13470,#8376,.T.);
#16671=EDGE_CURVE('',#13469,#13470,#2245,.T.);
#16672=EDGE_CURVE('',#13454,#13471,#8377,.T.);
#16673=EDGE_CURVE('',#13470,#13471,#8378,.T.);
#16674=EDGE_CURVE('',#13472,#13453,#8379,.T.);
#16675=EDGE_CURVE('',#13471,#13472,#8380,.T.);
#16676=EDGE_CURVE('',#13473,#13468,#2246,.T.);
#16677=EDGE_CURVE('',#13473,#13458,#8381,.T.);
#16678=EDGE_CURVE('',#13472,#13463,#2247,.T.);
#16679=EDGE_CURVE('',#13460,#13474,#8382,.T.);
#16680=EDGE_CURVE('',#13475,#13474,#2248,.T.);
#16681=EDGE_CURVE('',#13461,#13475,#8383,.T.);
#16682=EDGE_CURVE('',#13459,#13476,#8384,.T.);
#16683=EDGE_CURVE('',#13474,#13476,#8385,.T.);
#16684=EDGE_CURVE('',#13476,#13473,#8386,.T.);
#16685=EDGE_CURVE('',#13462,#13477,#8387,.T.);
#16686=EDGE_CURVE('',#13477,#13475,#8388,.T.);
#16687=EDGE_CURVE('',#13467,#13477,#2249,.T.);
#16688=EDGE_CURVE('',#13478,#13479,#2250,.T.);
#16689=EDGE_CURVE('',#13479,#13480,#8389,.T.);
#16690=EDGE_CURVE('',#13480,#13481,#2251,.T.);
#16691=EDGE_CURVE('',#13481,#13482,#8390,.T.);
#16692=EDGE_CURVE('',#13482,#13483,#2252,.T.);
#16693=EDGE_CURVE('',#13483,#13484,#8391,.T.);
#16694=EDGE_CURVE('',#13484,#13485,#2253,.T.);
#16695=EDGE_CURVE('',#13485,#13478,#8392,.T.);
#16696=EDGE_CURVE('',#13486,#13486,#2254,.T.);
#16697=EDGE_CURVE('',#13487,#13487,#2255,.T.);
#16698=EDGE_CURVE('',#13488,#13488,#2256,.T.);
#16699=EDGE_CURVE('',#13489,#13489,#2257,.T.);
#16700=EDGE_CURVE('',#13490,#13491,#2258,.T.);
#16701=EDGE_CURVE('',#13492,#13491,#8393,.T.);
#16702=EDGE_CURVE('',#13492,#13493,#2259,.T.);
#16703=EDGE_CURVE('',#13494,#13493,#8394,.T.);
#16704=EDGE_CURVE('',#13494,#13495,#2260,.T.);
#16705=EDGE_CURVE('',#13496,#13495,#8395,.T.);
#16706=EDGE_CURVE('',#13496,#13497,#2261,.T.);
#16707=EDGE_CURVE('',#13490,#13497,#8396,.T.);
#16708=EDGE_CURVE('',#13498,#13499,#2262,.T.);
#16709=EDGE_CURVE('',#13479,#13499,#8397,.T.);
#16710=EDGE_CURVE('',#13478,#13498,#8398,.T.);
#16711=EDGE_CURVE('',#13498,#13500,#2263,.T.);
#16712=EDGE_CURVE('',#13500,#13501,#2264,.T.);
#16713=EDGE_CURVE('',#13499,#13501,#2265,.T.);
#16714=EDGE_CURVE('',#13501,#13502,#8399,.T.);
#16715=EDGE_CURVE('',#13503,#13502,#2266,.T.);
#16716=EDGE_CURVE('',#13499,#13503,#8400,.T.);
#16717=EDGE_CURVE('',#13504,#13505,#2267,.T.);
#16718=EDGE_CURVE('',#13504,#13506,#8401,.T.);
#16719=EDGE_CURVE('',#13507,#13506,#8402,.T.);
#16720=EDGE_CURVE('',#13508,#13507,#2268,.T.);
#16721=EDGE_CURVE('',#13509,#13508,#8403,.T.);
#16722=EDGE_CURVE('',#13509,#13505,#8404,.T.);
#16723=EDGE_CURVE('',#13510,#13510,#2269,.T.);
#16724=EDGE_CURVE('',#13511,#13512,#2270,.T.);
#16725=EDGE_CURVE('',#13511,#13513,#8405,.T.);
#16726=EDGE_CURVE('',#13514,#13513,#8406,.T.);
#16727=EDGE_CURVE('',#13515,#13514,#2271,.T.);
#16728=EDGE_CURVE('',#13516,#13515,#8407,.T.);
#16729=EDGE_CURVE('',#13516,#13512,#8408,.T.);
#16730=EDGE_CURVE('',#13517,#13517,#2272,.T.);
#16731=EDGE_CURVE('',#13518,#13519,#2273,.T.);
#16732=EDGE_CURVE('',#13518,#13502,#8409,.T.);
#16733=EDGE_CURVE('',#13520,#13500,#8410,.T.);
#16734=EDGE_CURVE('',#13520,#13519,#8411,.T.);
#16735=EDGE_CURVE('',#13521,#13521,#2274,.T.);
#16736=EDGE_CURVE('',#13522,#13523,#2275,.T.);
#16737=EDGE_CURVE('',#13522,#13524,#8412,.T.);
#16738=EDGE_CURVE('',#13525,#13524,#8413,.T.);
#16739=EDGE_CURVE('',#13526,#13525,#2276,.T.);
#16740=EDGE_CURVE('',#13527,#13526,#8414,.T.);
#16741=EDGE_CURVE('',#13527,#13523,#8415,.T.);
#16742=EDGE_CURVE('',#13528,#13528,#2277,.T.);
#16743=EDGE_CURVE('',#13486,#13521,#8416,.T.);
#16744=EDGE_CURVE('',#13487,#13517,#8417,.T.);
#16745=EDGE_CURVE('',#13488,#13510,#8418,.T.);
#16746=EDGE_CURVE('',#13489,#13528,#8419,.T.);
#16747=EDGE_CURVE('',#13505,#13529,#2278,.T.);
#16748=EDGE_CURVE('',#13530,#13529,#2279,.T.);
#16749=EDGE_CURVE('',#13504,#13530,#2280,.T.);
#16750=EDGE_CURVE('',#13531,#13530,#743,.T.);
#16751=EDGE_CURVE('',#13532,#13531,#2281,.T.);
#16752=EDGE_CURVE('',#13532,#13504,#744,.T.);
#16753=EDGE_CURVE('',#13533,#13534,#2282,.T.);
#16754=EDGE_CURVE('',#13533,#13535,#8420,.T.);
#16755=EDGE_CURVE('',#13535,#13531,#2283,.T.);
#16756=EDGE_CURVE('',#13529,#13536,#745,.T.);
#16757=EDGE_CURVE('',#13536,#13537,#2284,.T.);
#16758=EDGE_CURVE('',#13537,#13538,#746,.T.);
#16759=EDGE_CURVE('',#13538,#13539,#2285,.T.);
#16760=EDGE_CURVE('',#13539,#13540,#747,.T.);
#16761=EDGE_CURVE('',#13540,#13541,#2286,.T.);
#16762=EDGE_CURVE('',#13541,#13542,#748,.T.);
#16763=EDGE_CURVE('',#13542,#13543,#2287,.T.);
#16764=EDGE_CURVE('',#13543,#13544,#749,.T.);
#16765=EDGE_CURVE('',#13544,#13545,#2288,.T.);
#16766=EDGE_CURVE('',#13545,#13546,#750,.T.);
#16767=EDGE_CURVE('',#13546,#13547,#2289,.T.);
#16768=EDGE_CURVE('',#13547,#13548,#751,.T.);
#16769=EDGE_CURVE('',#13548,#13535,#2290,.T.);
#16770=EDGE_CURVE('',#13534,#13533,#2291,.T.);
#16771=EDGE_CURVE('',#13549,#13550,#2292,.T.);
#16772=EDGE_CURVE('',#13549,#13531,#2293,.T.);
#16773=EDGE_CURVE('',#13550,#13548,#2294,.T.);
#16774=EDGE_CURVE('',#13551,#13550,#8421,.T.);
#16775=EDGE_CURVE('',#13552,#13551,#8422,.T.);
#16776=EDGE_CURVE('',#13549,#13552,#8423,.T.);
#16777=EDGE_CURVE('',#13553,#13554,#2295,.T.);
#16778=EDGE_CURVE('',#13555,#13553,#8424,.T.);
#16779=EDGE_CURVE('',#13556,#13555,#8425,.T.);
#16780=EDGE_CURVE('',#13554,#13556,#8426,.T.);
#16781=EDGE_CURVE('',#13557,#13558,#2296,.T.);
#16782=EDGE_CURVE('',#13559,#13558,#8427,.T.);
#16783=EDGE_CURVE('',#13560,#13559,#8428,.T.);
#16784=EDGE_CURVE('',#13557,#13560,#8429,.T.);
#16785=EDGE_CURVE('',#13561,#13562,#2297,.T.);
#16786=EDGE_CURVE('',#13563,#13561,#8430,.T.);
#16787=EDGE_CURVE('',#13564,#13563,#8431,.T.);
#16788=EDGE_CURVE('',#13562,#13564,#8432,.T.);
#16789=EDGE_CURVE('',#13532,#13549,#2298,.T.);
#16790=EDGE_CURVE('',#13565,#13552,#752,.T.);
#16791=EDGE_CURVE('',#13532,#13565,#8433,.T.);
#16792=EDGE_CURVE('',#13565,#13506,#2299,.T.);
#16793=EDGE_CURVE('',#13566,#13565,#2300,.T.);
#16794=EDGE_CURVE('',#13566,#13506,#2301,.T.);
#16795=EDGE_CURVE('',#13567,#13566,#8434,.T.);
#16796=EDGE_CURVE('',#13567,#13507,#2302,.T.);
#16797=EDGE_CURVE('',#13568,#13567,#2303,.T.);
#16798=EDGE_CURVE('',#13568,#13508,#2304,.T.);
#16799=EDGE_CURVE('',#13483,#13567,#8435,.T.);
#16800=EDGE_CURVE('',#13482,#13568,#8436,.T.);
#16801=EDGE_CURVE('',#13569,#13570,#8437,.T.);
#16802=EDGE_CURVE('',#13570,#13571,#753,.T.);
#16803=EDGE_CURVE('',#13571,#13572,#8438,.T.);
#16804=EDGE_CURVE('',#13572,#13573,#754,.T.);
#16805=EDGE_CURVE('',#13573,#13568,#8439,.T.);
#16806=EDGE_CURVE('',#13481,#13569,#8440,.T.);
#16807=EDGE_CURVE('',#13570,#13513,#2305,.T.);
#16808=EDGE_CURVE('',#13569,#13514,#2306,.T.);
#16809=EDGE_CURVE('',#13574,#13569,#2307,.T.);
#16810=EDGE_CURVE('',#13574,#13515,#2308,.T.);
#16811=EDGE_CURVE('',#13480,#13574,#8441,.T.);
#16812=EDGE_CURVE('',#13575,#13576,#755,.T.);
#16813=EDGE_CURVE('',#13576,#13574,#8442,.T.);
#16814=EDGE_CURVE('',#13503,#13577,#756,.T.);
#16815=EDGE_CURVE('',#13577,#13575,#8443,.T.);
#16816=EDGE_CURVE('',#13559,#13578,#757,.T.);
#16817=EDGE_CURVE('',#13576,#13578,#758,.T.);
#16818=EDGE_CURVE('',#13575,#13559,#2309,.T.);
#16819=EDGE_CURVE('',#13558,#13579,#2310,.T.);
#16820=EDGE_CURVE('',#13578,#13579,#8444,.T.);
#16821=EDGE_CURVE('',#13558,#13540,#2311,.T.);
#16822=EDGE_CURVE('',#13579,#13540,#2312,.T.);
#16823=EDGE_CURVE('',#13512,#13579,#759,.T.);
#16824=EDGE_CURVE('',#13512,#13539,#2313,.T.);
#16825=EDGE_CURVE('',#13516,#13578,#2314,.T.);
#16826=EDGE_CURVE('',#13576,#13516,#2315,.T.);
#16827=EDGE_CURVE('',#13511,#13538,#2316,.T.);
#16828=EDGE_CURVE('',#13580,#13537,#2317,.T.);
#16829=EDGE_CURVE('',#13580,#13511,#760,.T.);
#16830=EDGE_CURVE('',#13580,#13581,#8445,.T.);
#16831=EDGE_CURVE('',#13581,#13513,#2318,.T.);
#16832=EDGE_CURVE('',#13570,#13581,#2319,.T.);
#16833=EDGE_CURVE('',#13581,#13556,#761,.T.);
#16834=EDGE_CURVE('',#13571,#13556,#2320,.T.);
#16835=EDGE_CURVE('',#13572,#13555,#2321,.T.);
#16836=EDGE_CURVE('',#13555,#13582,#762,.T.);
#16837=EDGE_CURVE('',#13573,#13582,#763,.T.);
#16838=EDGE_CURVE('',#13553,#13583,#2322,.T.);
#16839=EDGE_CURVE('',#13582,#13583,#8446,.T.);
#16840=EDGE_CURVE('',#13553,#13536,#2323,.T.);
#16841=EDGE_CURVE('',#13583,#13536,#2324,.T.);
#16842=EDGE_CURVE('',#13505,#13583,#764,.T.);
#16843=EDGE_CURVE('',#13509,#13582,#2325,.T.);
#16844=EDGE_CURVE('',#13573,#13509,#2326,.T.);
#16845=EDGE_CURVE('',#13554,#13537,#2327,.T.);
#16846=EDGE_CURVE('',#13580,#13554,#2328,.T.);
#16847=EDGE_CURVE('',#13557,#13541,#2329,.T.);
#16848=EDGE_CURVE('',#13523,#13584,#765,.T.);
#16849=EDGE_CURVE('',#13584,#13548,#2330,.T.);
#16850=EDGE_CURVE('',#13523,#13547,#2331,.T.);
#16851=EDGE_CURVE('',#13527,#13585,#2332,.T.);
#16852=EDGE_CURVE('',#13585,#13584,#8447,.T.);
#16853=EDGE_CURVE('',#13550,#13584,#2333,.T.);
#16854=EDGE_CURVE('',#13551,#13585,#766,.T.);
#16855=EDGE_CURVE('',#13586,#13585,#767,.T.);
#16856=EDGE_CURVE('',#13587,#13586,#768,.T.);
#16857=EDGE_CURVE('',#13587,#13551,#2334,.T.);
#16858=EDGE_CURVE('',#13588,#13587,#8448,.T.);
#16859=EDGE_CURVE('',#13588,#13552,#2335,.T.);
#16860=EDGE_CURVE('',#13566,#13588,#769,.T.);
#16861=EDGE_CURVE('',#13586,#13589,#8449,.T.);
#16862=EDGE_CURVE('',#13484,#13589,#8450,.T.);
#16863=EDGE_CURVE('',#13589,#13590,#2336,.T.);
#16864=EDGE_CURVE('',#13485,#13590,#8451,.T.);
#16865=EDGE_CURVE('',#13589,#13526,#2337,.T.);
#16866=EDGE_CURVE('',#13590,#13525,#2338,.T.);
#16867=EDGE_CURVE('',#13591,#13524,#2339,.T.);
#16868=EDGE_CURVE('',#13590,#13591,#8452,.T.);
#16869=EDGE_CURVE('',#13591,#13592,#770,.T.);
#16870=EDGE_CURVE('',#13592,#13593,#8453,.T.);
#16871=EDGE_CURVE('',#13593,#13594,#771,.T.);
#16872=EDGE_CURVE('',#13594,#13498,#8454,.T.);
#16873=EDGE_CURVE('',#13594,#13520,#2340,.T.);
#16874=EDGE_CURVE('',#13520,#13595,#2341,.T.);
#16875=EDGE_CURVE('',#13594,#13595,#2342,.T.);
#16876=EDGE_CURVE('',#13519,#13596,#772,.T.);
#16877=EDGE_CURVE('',#13595,#13596,#8455,.T.);
#16878=EDGE_CURVE('',#13596,#13544,#2343,.T.);
#16879=EDGE_CURVE('',#13519,#13543,#2344,.T.);
#16880=EDGE_CURVE('',#13518,#13542,#2345,.T.);
#16881=EDGE_CURVE('',#13597,#13541,#2346,.T.);
#16882=EDGE_CURVE('',#13597,#13518,#773,.T.);
#16883=EDGE_CURVE('',#13597,#13598,#8456,.T.);
#16884=EDGE_CURVE('',#13598,#13502,#2347,.T.);
#16885=EDGE_CURVE('',#13503,#13598,#2348,.T.);
#16886=EDGE_CURVE('',#13598,#13560,#774,.T.);
#16887=EDGE_CURVE('',#13577,#13560,#2349,.T.);
#16888=EDGE_CURVE('',#13597,#13557,#2350,.T.);
#16889=EDGE_CURVE('',#13561,#13596,#2351,.T.);
#16890=EDGE_CURVE('',#13561,#13544,#2352,.T.);
#16891=EDGE_CURVE('',#13563,#13595,#775,.T.);
#16892=EDGE_CURVE('',#13593,#13563,#2353,.T.);
#16893=EDGE_CURVE('',#13592,#13564,#2354,.T.);
#16894=EDGE_CURVE('',#13591,#13599,#2355,.T.);
#16895=EDGE_CURVE('',#13599,#13564,#776,.T.);
#16896=EDGE_CURVE('',#13600,#13562,#2356,.T.);
#16897=EDGE_CURVE('',#13600,#13599,#8457,.T.);
#16898=EDGE_CURVE('',#13600,#13545,#2357,.T.);
#16899=EDGE_CURVE('',#13562,#13545,#2358,.T.);
#16900=EDGE_CURVE('',#13600,#13522,#777,.T.);
#16901=EDGE_CURVE('',#13522,#13546,#2359,.T.);
#16902=EDGE_CURVE('',#13599,#13524,#2360,.T.);
#16903=EDGE_CURVE('',#13586,#13527,#2361,.T.);
#16904=EDGE_CURVE('',#13601,#13601,#2362,.T.);
#16905=EDGE_CURVE('',#13601,#13534,#2363,.T.);
#16906=EDGE_CURVE('',#13602,#13602,#2364,.T.);
#16907=EDGE_CURVE('',#13603,#13604,#2365,.T.);
#16908=EDGE_CURVE('',#13604,#13603,#2366,.T.);
#16909=EDGE_CURVE('',#13604,#13602,#2367,.T.);
#16910=EDGE_CURVE('',#13605,#13605,#2368,.T.);
#16911=EDGE_CURVE('',#13605,#13603,#8458,.T.);
#16912=EDGE_CURVE('',#13606,#13606,#2369,.T.);
#16913=EDGE_CURVE('',#13607,#13607,#2370,.T.);
#16914=EDGE_CURVE('',#13607,#13606,#8459,.T.);
#16915=EDGE_CURVE('',#13608,#13608,#2371,.T.);
#16916=EDGE_CURVE('',#13609,#13609,#2372,.T.);
#16917=EDGE_CURVE('',#13609,#13608,#8460,.T.);
#16918=EDGE_CURVE('',#13610,#13610,#2373,.T.);
#16919=EDGE_CURVE('',#13611,#13611,#2374,.T.);
#16920=EDGE_CURVE('',#13611,#13610,#8461,.T.);
#16921=EDGE_CURVE('',#13612,#13612,#2375,.T.);
#16922=EDGE_CURVE('',#13613,#13613,#2376,.T.);
#16923=EDGE_CURVE('',#13613,#13612,#8462,.T.);
#16924=EDGE_CURVE('',#13614,#13614,#2377,.T.);
#16925=EDGE_CURVE('',#13615,#13615,#2378,.T.);
#16926=EDGE_CURVE('',#13615,#13614,#8463,.T.);
#16927=EDGE_CURVE('',#13616,#13616,#2379,.T.);
#16928=EDGE_CURVE('',#13617,#13617,#2380,.T.);
#16929=EDGE_CURVE('',#13617,#13616,#8464,.T.);
#16930=EDGE_CURVE('',#13618,#13619,#2381,.T.);
#16931=EDGE_CURVE('',#13619,#13620,#8465,.T.);
#16932=EDGE_CURVE('',#13620,#13621,#2382,.T.);
#16933=EDGE_CURVE('',#13621,#13622,#8466,.T.);
#16934=EDGE_CURVE('',#13622,#13623,#2383,.T.);
#16935=EDGE_CURVE('',#13623,#13624,#8467,.T.);
#16936=EDGE_CURVE('',#13624,#13625,#2384,.T.);
#16937=EDGE_CURVE('',#13625,#13618,#8468,.T.);
#16938=EDGE_CURVE('',#13490,#13619,#8469,.T.);
#16939=EDGE_CURVE('',#13491,#13618,#8470,.T.);
#16940=EDGE_CURVE('',#13492,#13625,#8471,.T.);
#16941=EDGE_CURVE('',#13493,#13624,#8472,.T.);
#16942=EDGE_CURVE('',#13494,#13623,#8473,.T.);
#16943=EDGE_CURVE('',#13495,#13622,#8474,.T.);
#16944=EDGE_CURVE('',#13496,#13621,#8475,.T.);
#16945=EDGE_CURVE('',#13497,#13620,#8476,.T.);
#16946=EDGE_CURVE('',#13626,#13627,#2385,.T.);
#16947=EDGE_CURVE('',#13627,#13626,#2386,.T.);
#16948=EDGE_CURVE('',#13626,#13628,#2387,.T.);
#16949=EDGE_CURVE('',#13628,#13628,#2388,.T.);
#16950=EDGE_CURVE('',#13629,#13630,#2389,.T.);
#16951=EDGE_CURVE('',#13630,#13629,#2390,.T.);
#16952=EDGE_CURVE('',#13630,#13627,#8477,.T.);
#16953=EDGE_CURVE('',#13631,#13631,#2391,.T.);
#16954=EDGE_CURVE('',#13629,#13632,#8478,.T.);
#16955=EDGE_CURVE('',#13632,#13632,#2392,.T.);
#16956=EDGE_CURVE('',#13633,#13634,#2393,.T.);
#16957=EDGE_CURVE('',#13634,#13633,#2394,.T.);
#16958=EDGE_CURVE('',#13633,#13635,#2395,.T.);
#16959=EDGE_CURVE('',#13635,#13635,#2396,.T.);
#16960=EDGE_CURVE('',#13636,#13637,#8479,.T.);
#16961=EDGE_CURVE('',#13637,#13638,#8480,.T.);
#16962=EDGE_CURVE('',#13638,#13639,#8481,.T.);
#16963=EDGE_CURVE('',#13639,#13640,#8482,.T.);
#16964=EDGE_CURVE('',#13640,#13641,#8483,.T.);
#16965=EDGE_CURVE('',#13641,#13636,#8484,.T.);
#16966=EDGE_CURVE('',#13631,#13634,#8485,.T.);
#16967=EDGE_CURVE('',#13642,#13643,#476,.T.);
#16968=EDGE_CURVE('',#13642,#13641,#8486,.T.);
#16969=EDGE_CURVE('',#13643,#13640,#8487,.T.);
#16970=EDGE_CURVE('',#13644,#13642,#477,.T.);
#16971=EDGE_CURVE('',#13644,#13636,#8488,.T.);
#16972=EDGE_CURVE('',#13645,#13644,#478,.T.);
#16973=EDGE_CURVE('',#13645,#13637,#8489,.T.);
#16974=EDGE_CURVE('',#13646,#13645,#479,.T.);
#16975=EDGE_CURVE('',#13638,#13646,#8490,.T.);
#16976=EDGE_CURVE('',#13643,#13647,#480,.T.);
#16977=EDGE_CURVE('',#13648,#13639,#8491,.T.);
#16978=EDGE_CURVE('',#13647,#13648,#481,.T.);
#16979=EDGE_CURVE('',#13648,#13646,#482,.T.);
#16980=EDGE_CURVE('',#13649,#13647,#8492,.T.);
#16981=EDGE_CURVE('',#13650,#13651,#2397,.T.);
#16982=EDGE_CURVE('',#13651,#13650,#2398,.T.);
#16983=EDGE_CURVE('',#13650,#13652,#2399,.T.);
#16984=EDGE_CURVE('',#13652,#13652,#2400,.T.);
#16985=EDGE_CURVE('',#13653,#13654,#2401,.T.);
#16986=EDGE_CURVE('',#13654,#13653,#2402,.T.);
#16987=EDGE_CURVE('',#13654,#13651,#8493,.T.);
#16988=EDGE_CURVE('',#13655,#13655,#2403,.T.);
#16989=EDGE_CURVE('',#13653,#13656,#8494,.T.);
#16990=EDGE_CURVE('',#13656,#13656,#2404,.T.);
#16991=EDGE_CURVE('',#13657,#13658,#2405,.T.);
#16992=EDGE_CURVE('',#13658,#13657,#2406,.T.);
#16993=EDGE_CURVE('',#13657,#13659,#2407,.T.);
#16994=EDGE_CURVE('',#13659,#13659,#2408,.T.);
#16995=EDGE_CURVE('',#13660,#13661,#8495,.T.);
#16996=EDGE_CURVE('',#13661,#13662,#8496,.T.);
#16997=EDGE_CURVE('',#13662,#13663,#8497,.T.);
#16998=EDGE_CURVE('',#13663,#13664,#8498,.T.);
#16999=EDGE_CURVE('',#13664,#13665,#8499,.T.);
#17000=EDGE_CURVE('',#13665,#13660,#8500,.T.);
#17001=EDGE_CURVE('',#13655,#13658,#8501,.T.);
#17002=EDGE_CURVE('',#13666,#13667,#483,.T.);
#17003=EDGE_CURVE('',#13666,#13665,#8502,.T.);
#17004=EDGE_CURVE('',#13667,#13664,#8503,.T.);
#17005=EDGE_CURVE('',#13668,#13666,#484,.T.);
#17006=EDGE_CURVE('',#13668,#13660,#8504,.T.);
#17007=EDGE_CURVE('',#13669,#13668,#485,.T.);
#17008=EDGE_CURVE('',#13669,#13661,#8505,.T.);
#17009=EDGE_CURVE('',#13670,#13669,#486,.T.);
#17010=EDGE_CURVE('',#13662,#13670,#8506,.T.);
#17011=EDGE_CURVE('',#13667,#13671,#487,.T.);
#17012=EDGE_CURVE('',#13672,#13663,#8507,.T.);
#17013=EDGE_CURVE('',#13671,#13672,#488,.T.);
#17014=EDGE_CURVE('',#13672,#13670,#489,.T.);
#17015=EDGE_CURVE('',#13673,#13671,#8508,.T.);
#17016=EDGE_CURVE('',#13674,#13675,#2409,.T.);
#17017=EDGE_CURVE('',#13675,#13674,#2410,.T.);
#17018=EDGE_CURVE('',#13674,#13676,#2411,.T.);
#17019=EDGE_CURVE('',#13676,#13676,#2412,.T.);
#17020=EDGE_CURVE('',#13677,#13678,#2413,.T.);
#17021=EDGE_CURVE('',#13678,#13677,#2414,.T.);
#17022=EDGE_CURVE('',#13678,#13675,#8509,.T.);
#17023=EDGE_CURVE('',#13679,#13679,#2415,.T.);
#17024=EDGE_CURVE('',#13677,#13680,#8510,.T.);
#17025=EDGE_CURVE('',#13680,#13680,#2416,.T.);
#17026=EDGE_CURVE('',#13681,#13682,#2417,.T.);
#17027=EDGE_CURVE('',#13682,#13681,#2418,.T.);
#17028=EDGE_CURVE('',#13681,#13683,#2419,.T.);
#17029=EDGE_CURVE('',#13683,#13683,#2420,.T.);
#17030=EDGE_CURVE('',#13684,#13685,#8511,.T.);
#17031=EDGE_CURVE('',#13685,#13686,#8512,.T.);
#17032=EDGE_CURVE('',#13686,#13687,#8513,.T.);
#17033=EDGE_CURVE('',#13687,#13688,#8514,.T.);
#17034=EDGE_CURVE('',#13688,#13689,#8515,.T.);
#17035=EDGE_CURVE('',#13689,#13684,#8516,.T.);
#17036=EDGE_CURVE('',#13679,#13682,#8517,.T.);
#17037=EDGE_CURVE('',#13690,#13691,#490,.T.);
#17038=EDGE_CURVE('',#13690,#13689,#8518,.T.);
#17039=EDGE_CURVE('',#13691,#13688,#8519,.T.);
#17040=EDGE_CURVE('',#13692,#13690,#491,.T.);
#17041=EDGE_CURVE('',#13692,#13684,#8520,.T.);
#17042=EDGE_CURVE('',#13693,#13692,#492,.T.);
#17043=EDGE_CURVE('',#13693,#13685,#8521,.T.);
#17044=EDGE_CURVE('',#13694,#13693,#493,.T.);
#17045=EDGE_CURVE('',#13686,#13694,#8522,.T.);
#17046=EDGE_CURVE('',#13691,#13695,#494,.T.);
#17047=EDGE_CURVE('',#13696,#13687,#8523,.T.);
#17048=EDGE_CURVE('',#13695,#13696,#495,.T.);
#17049=EDGE_CURVE('',#13696,#13694,#496,.T.);
#17050=EDGE_CURVE('',#13697,#13695,#8524,.T.);
#17051=EDGE_CURVE('',#13698,#13699,#2421,.T.);
#17052=EDGE_CURVE('',#13699,#13698,#2422,.T.);
#17053=EDGE_CURVE('',#13698,#13700,#2423,.T.);
#17054=EDGE_CURVE('',#13700,#13700,#2424,.T.);
#17055=EDGE_CURVE('',#13701,#13702,#2425,.T.);
#17056=EDGE_CURVE('',#13702,#13701,#2426,.T.);
#17057=EDGE_CURVE('',#13702,#13699,#8525,.T.);
#17058=EDGE_CURVE('',#13703,#13703,#2427,.T.);
#17059=EDGE_CURVE('',#13701,#13704,#8526,.T.);
#17060=EDGE_CURVE('',#13704,#13704,#2428,.T.);
#17061=EDGE_CURVE('',#13705,#13706,#497,.T.);
#17062=EDGE_CURVE('',#13707,#13705,#2429,.T.);
#17063=EDGE_CURVE('',#13706,#13707,#498,.T.);
#17064=EDGE_CURVE('',#13708,#13709,#499,.T.);
#17065=EDGE_CURVE('',#13707,#13708,#500,.T.);
#17066=EDGE_CURVE('',#13709,#13707,#2430,.T.);
#17067=EDGE_CURVE('',#13710,#13711,#501,.T.);
#17068=EDGE_CURVE('',#13705,#13710,#2431,.T.);
#17069=EDGE_CURVE('',#13711,#13705,#502,.T.);
#17070=EDGE_CURVE('',#13712,#13713,#503,.T.);
#17071=EDGE_CURVE('',#13709,#13712,#504,.T.);
#17072=EDGE_CURVE('',#13713,#13709,#2432,.T.);
#17073=EDGE_CURVE('',#13714,#13715,#505,.T.);
#17074=EDGE_CURVE('',#13710,#13714,#2433,.T.);
#17075=EDGE_CURVE('',#13715,#13710,#506,.T.);
#17076=EDGE_CURVE('',#13716,#13714,#507,.T.);
#17077=EDGE_CURVE('',#13713,#13716,#508,.T.);
#17078=EDGE_CURVE('',#13714,#13713,#2434,.T.);
#17079=EDGE_CURVE('',#13717,#13715,#8527,.T.);
#17080=EDGE_CURVE('',#13718,#13717,#8528,.T.);
#17081=EDGE_CURVE('',#13718,#13716,#8529,.T.);
#17082=EDGE_CURVE('',#13719,#13711,#8530,.T.);
#17083=EDGE_CURVE('',#13717,#13719,#8531,.T.);
#17084=EDGE_CURVE('',#13720,#13706,#8532,.T.);
#17085=EDGE_CURVE('',#13719,#13720,#8533,.T.);
#17086=EDGE_CURVE('',#13720,#13721,#8534,.T.);
#17087=EDGE_CURVE('',#13721,#13722,#8535,.T.);
#17088=EDGE_CURVE('',#13722,#13718,#8536,.T.);
#17089=EDGE_CURVE('',#13723,#13723,#2435,.T.);
#17090=EDGE_CURVE('',#13721,#13708,#8537,.T.);
#17091=EDGE_CURVE('',#13722,#13712,#8538,.T.);
#17092=EDGE_CURVE('',#13703,#13723,#8539,.T.);
#17093=EDGE_CURVE('',#13724,#13725,#8540,.T.);
#17094=EDGE_CURVE('',#13726,#13724,#8541,.T.);
#17095=EDGE_CURVE('',#13727,#13726,#8542,.T.);
#17096=EDGE_CURVE('',#13727,#13725,#8543,.T.);
#17097=EDGE_CURVE('',#13725,#13728,#8544,.T.);
#17098=EDGE_CURVE('',#13729,#13727,#8545,.T.);
#17099=EDGE_CURVE('',#13729,#13728,#8546,.T.);
#17100=EDGE_CURVE('',#13728,#13730,#8547,.T.);
#17101=EDGE_CURVE('',#13731,#13729,#8548,.T.);
#17102=EDGE_CURVE('',#13731,#13730,#8549,.T.);
#17103=EDGE_CURVE('',#13730,#13724,#8550,.T.);
#17104=EDGE_CURVE('',#13726,#13731,#8551,.T.);
#17105=EDGE_CURVE('',#13732,#13733,#8552,.T.);
#17106=EDGE_CURVE('',#13734,#13732,#8553,.T.);
#17107=EDGE_CURVE('',#13735,#13734,#8554,.F.);
#17108=EDGE_CURVE('',#13735,#13733,#8555,.F.);
#17109=EDGE_CURVE('',#13733,#13736,#8556,.T.);
#17110=EDGE_CURVE('',#13737,#13735,#8557,.F.);
#17111=EDGE_CURVE('',#13737,#13736,#8558,.F.);
#17112=EDGE_CURVE('',#13736,#13738,#8559,.T.);
#17113=EDGE_CURVE('',#13739,#13737,#8560,.F.);
#17114=EDGE_CURVE('',#13739,#13738,#8561,.F.);
#17115=EDGE_CURVE('',#13738,#13732,#8562,.T.);
#17116=EDGE_CURVE('',#13734,#13739,#8563,.F.);
#17117=EDGE_CURVE('',#13740,#13741,#8564,.T.);
#17118=EDGE_CURVE('',#13742,#13741,#8565,.T.);
#17119=EDGE_CURVE('',#13742,#13743,#8566,.T.);
#17120=EDGE_CURVE('',#13743,#13740,#8567,.T.);
#17121=EDGE_CURVE('',#13741,#13744,#8568,.T.);
#17122=EDGE_CURVE('',#13745,#13744,#8569,.T.);
#17123=EDGE_CURVE('',#13745,#13742,#8570,.T.);
#17124=EDGE_CURVE('',#13744,#13746,#8571,.T.);
#17125=EDGE_CURVE('',#13747,#13746,#8572,.T.);
#17126=EDGE_CURVE('',#13747,#13745,#8573,.T.);
#17127=EDGE_CURVE('',#13746,#13740,#8574,.T.);
#17128=EDGE_CURVE('',#13743,#13747,#8575,.T.);
#17129=EDGE_CURVE('',#13748,#13748,#2436,.T.);
#17130=EDGE_CURVE('',#13748,#13749,#8576,.T.);
#17131=EDGE_CURVE('',#13749,#13749,#2437,.T.);
#17132=EDGE_CURVE('',#13750,#13750,#2438,.T.);
#17133=EDGE_CURVE('',#13750,#13751,#8577,.T.);
#17134=EDGE_CURVE('',#13751,#13751,#2439,.T.);
#17135=EDGE_CURVE('',#13752,#13752,#2440,.T.);
#17136=EDGE_CURVE('',#13752,#13753,#8578,.T.);
#17137=EDGE_CURVE('',#13753,#13753,#2441,.T.);
#17138=EDGE_CURVE('',#13754,#13754,#2442,.T.);
#17139=EDGE_CURVE('',#13754,#13755,#8579,.T.);
#17140=EDGE_CURVE('',#13755,#13755,#2443,.T.);
#17141=EDGE_CURVE('',#13756,#13756,#2444,.T.);
#17142=EDGE_CURVE('',#13756,#13757,#8580,.T.);
#17143=EDGE_CURVE('',#13757,#13757,#2445,.T.);
#17144=EDGE_CURVE('',#13758,#13758,#2446,.T.);
#17145=EDGE_CURVE('',#13758,#13759,#8581,.T.);
#17146=EDGE_CURVE('',#13759,#13759,#2447,.T.);
#17147=EDGE_CURVE('',#13760,#13761,#8582,.T.);
#17148=EDGE_CURVE('',#13761,#13762,#8583,.T.);
#17149=EDGE_CURVE('',#13762,#13763,#8584,.T.);
#17150=EDGE_CURVE('',#13763,#13760,#8585,.T.);
#17151=EDGE_CURVE('',#13764,#13765,#8586,.T.);
#17152=EDGE_CURVE('',#13766,#13764,#8587,.T.);
#17153=EDGE_CURVE('',#13767,#13766,#8588,.T.);
#17154=EDGE_CURVE('',#13765,#13767,#8589,.T.);
#17155=EDGE_CURVE('',#13768,#13769,#8590,.T.);
#17156=EDGE_CURVE('',#13769,#13760,#8591,.T.);
#17157=EDGE_CURVE('',#13768,#13763,#8592,.T.);
#17158=EDGE_CURVE('',#13770,#13768,#8593,.T.);
#17159=EDGE_CURVE('',#13770,#13762,#8594,.T.);
#17160=EDGE_CURVE('',#13771,#13770,#8595,.T.);
#17161=EDGE_CURVE('',#13771,#13761,#8596,.T.);
#17162=EDGE_CURVE('',#13769,#13771,#8597,.T.);
#17163=EDGE_CURVE('',#13767,#13772,#8598,.T.);
#17164=EDGE_CURVE('',#13772,#13773,#8599,.T.);
#17165=EDGE_CURVE('',#13765,#13773,#8600,.T.);
#17166=EDGE_CURVE('',#13774,#13766,#8601,.T.);
#17167=EDGE_CURVE('',#13775,#13774,#8602,.T.);
#17168=EDGE_CURVE('',#13776,#13775,#8603,.T.);
#17169=EDGE_CURVE('',#13772,#13776,#8604,.T.);
#17170=EDGE_CURVE('',#13777,#13778,#8605,.T.);
#17171=EDGE_CURVE('',#13779,#13777,#8606,.T.);
#17172=EDGE_CURVE('',#13780,#13779,#8607,.T.);
#17173=EDGE_CURVE('',#13780,#13778,#8608,.T.);
#17174=EDGE_CURVE('',#13781,#13778,#8609,.T.);
#17175=EDGE_CURVE('',#13781,#13782,#8610,.F.);
#17176=EDGE_CURVE('',#13782,#13777,#8611,.T.);
#17177=EDGE_CURVE('',#13783,#13784,#8612,.T.);
#17178=EDGE_CURVE('',#13785,#13784,#8613,.T.);
#17179=EDGE_CURVE('',#13786,#13785,#8614,.T.);
#17180=EDGE_CURVE('',#13783,#13786,#8615,.T.);
#17181=EDGE_CURVE('',#13787,#13782,#8616,.T.);
#17182=EDGE_CURVE('',#13788,#13781,#8617,.T.);
#17183=EDGE_CURVE('',#13788,#13787,#8618,.T.);
#17184=EDGE_CURVE('',#13789,#13787,#8619,.T.);
#17185=EDGE_CURVE('',#13790,#13788,#8620,.T.);
#17186=EDGE_CURVE('',#13789,#13790,#8621,.T.);
#17187=EDGE_CURVE('',#13784,#13791,#8622,.T.);
#17188=EDGE_CURVE('',#13792,#13791,#8623,.T.);
#17189=EDGE_CURVE('',#13785,#13792,#8624,.T.);
#17190=EDGE_CURVE('',#13790,#13792,#8625,.T.);
#17191=EDGE_CURVE('',#13786,#13780,#8626,.T.);
#17192=EDGE_CURVE('',#13791,#13789,#8627,.T.);
#17193=EDGE_CURVE('',#13779,#13783,#8628,.T.);
#17194=EDGE_CURVE('',#13793,#13764,#8629,.T.);
#17195=EDGE_CURVE('',#13774,#13793,#8630,.T.);
#17196=EDGE_CURVE('',#13794,#13793,#8631,.T.);
#17197=EDGE_CURVE('',#13775,#13794,#8632,.T.);
#17198=EDGE_CURVE('',#13795,#13794,#8633,.T.);
#17199=EDGE_CURVE('',#13776,#13795,#8634,.T.);
#17200=EDGE_CURVE('',#13773,#13795,#8635,.T.);
#17201=EDGE_CURVE('',#13796,#13797,#778,.F.);
#17202=EDGE_CURVE('',#13797,#13798,#509,.T.);
#17203=EDGE_CURVE('',#13799,#13798,#2448,.T.);
#17204=EDGE_CURVE('',#13798,#13799,#2449,.T.);
#17205=EDGE_CURVE('',#13797,#13800,#779,.F.);
#17206=EDGE_CURVE('',#13800,#13801,#780,.T.);
#17207=EDGE_CURVE('',#13801,#13802,#781,.T.);
#17208=EDGE_CURVE('',#13802,#13803,#782,.T.);
#17209=EDGE_CURVE('',#13803,#13804,#783,.T.);
#17210=EDGE_CURVE('',#13804,#13805,#784,.T.);
#17211=EDGE_CURVE('',#13805,#13806,#785,.T.);
#17212=EDGE_CURVE('',#13806,#13807,#786,.T.);
#17213=EDGE_CURVE('',#13807,#13808,#787,.T.);
#17214=EDGE_CURVE('',#13808,#13809,#788,.T.);
#17215=EDGE_CURVE('',#13809,#13810,#789,.T.);
#17216=EDGE_CURVE('',#13810,#13796,#790,.T.);
#17217=EDGE_CURVE('',#13811,#13801,#8636,.T.);
#17218=EDGE_CURVE('',#13812,#13811,#8637,.T.);
#17219=EDGE_CURVE('',#13812,#13802,#8638,.T.);
#17220=EDGE_CURVE('',#13813,#13812,#8639,.T.);
#17221=EDGE_CURVE('',#13813,#13803,#8640,.T.);
#17222=EDGE_CURVE('',#13814,#13813,#8641,.T.);
#17223=EDGE_CURVE('',#13814,#13804,#8642,.T.);
#17224=EDGE_CURVE('',#13815,#13816,#2450,.T.);
#17225=EDGE_CURVE('',#13816,#13815,#8643,.T.);
#17226=EDGE_CURVE('',#13799,#13817,#8644,.T.);
#17227=EDGE_CURVE('',#13817,#13816,#791,.T.);
#17228=EDGE_CURVE('',#13815,#13817,#792,.T.);
#17229=EDGE_CURVE('',#13818,#13819,#2451,.T.);
#17230=EDGE_CURVE('',#13818,#13820,#793,.T.);
#17231=EDGE_CURVE('',#13820,#13821,#8645,.T.);
#17232=EDGE_CURVE('',#13821,#13822,#2452,.T.);
#17233=EDGE_CURVE('',#13823,#13822,#794,.T.);
#17234=EDGE_CURVE('',#13823,#13824,#2453,.T.);
#17235=EDGE_CURVE('',#13824,#13825,#8646,.T.);
#17236=EDGE_CURVE('',#13825,#13826,#795,.T.);
#17237=EDGE_CURVE('',#13826,#13827,#2454,.T.);
#17238=EDGE_CURVE('',#13819,#13827,#8647,.T.);
#17239=EDGE_CURVE('',#13828,#13829,#796,.T.);
#17240=EDGE_CURVE('',#13830,#13828,#8648,.T.);
#17241=EDGE_CURVE('',#13829,#13830,#797,.T.);
#17242=EDGE_CURVE('',#13831,#13823,#8649,.T.);
#17243=EDGE_CURVE('',#13832,#13822,#8650,.T.);
#17244=EDGE_CURVE('',#13831,#13832,#798,.T.);
#17245=EDGE_CURVE('',#13833,#13834,#799,.T.);
#17246=EDGE_CURVE('',#13835,#13834,#8651,.T.);
#17247=EDGE_CURVE('',#13836,#13835,#800,.T.);
#17248=EDGE_CURVE('',#13836,#13833,#8652,.T.);
#17249=EDGE_CURVE('',#13837,#13838,#8653,.T.);
#17250=EDGE_CURVE('',#13839,#13838,#801,.T.);
#17251=EDGE_CURVE('',#13839,#13840,#8654,.T.);
#17252=EDGE_CURVE('',#13837,#13840,#802,.T.);
#17253=EDGE_CURVE('',#13841,#13839,#8655,.T.);
#17254=EDGE_CURVE('',#13841,#13842,#8656,.T.);
#17255=EDGE_CURVE('',#13840,#13842,#8657,.T.);
#17256=EDGE_CURVE('',#13843,#13821,#8658,.T.);
#17257=EDGE_CURVE('',#13844,#13820,#8659,.T.);
#17258=EDGE_CURVE('',#13843,#13844,#8660,.T.);
#17259=EDGE_CURVE('',#13845,#13846,#2455,.T.);
#17260=EDGE_CURVE('',#13846,#13847,#803,.T.);
#17261=EDGE_CURVE('',#13847,#13848,#8661,.T.);
#17262=EDGE_CURVE('',#13848,#13848,#2456,.T.);
#17263=EDGE_CURVE('',#13847,#13845,#804,.T.);
#17264=EDGE_CURVE('',#13849,#13837,#2457,.T.);
#17265=EDGE_CURVE('',#13842,#13834,#2458,.T.);
#17266=EDGE_CURVE('',#13833,#13850,#2459,.T.);
#17267=EDGE_CURVE('',#13850,#13851,#8662,.T.);
#17268=EDGE_CURVE('',#13851,#13852,#805,.T.);
#17269=EDGE_CURVE('',#13853,#13852,#2460,.T.);
#17270=EDGE_CURVE('',#13853,#13849,#8663,.T.);
#17271=EDGE_CURVE('',#13845,#13846,#8664,.T.);
#17272=EDGE_CURVE('',#13854,#13855,#8665,.T.);
#17273=EDGE_CURVE('',#13856,#13854,#806,.T.);
#17274=EDGE_CURVE('',#13855,#13856,#807,.T.);
#17275=EDGE_CURVE('',#13857,#13858,#2461,.T.);
#17276=EDGE_CURVE('',#13858,#13859,#2462,.T.);
#17277=EDGE_CURVE('',#13859,#13860,#2463,.T.);
#17278=EDGE_CURVE('',#13860,#13861,#2464,.T.);
#17279=EDGE_CURVE('',#13861,#13862,#2465,.T.);
#17280=EDGE_CURVE('',#13862,#13863,#2466,.T.);
#17281=EDGE_CURVE('',#13863,#13864,#2467,.T.);
#17282=EDGE_CURVE('',#13864,#13865,#2468,.T.);
#17283=EDGE_CURVE('',#13865,#13866,#2469,.T.);
#17284=EDGE_CURVE('',#13866,#13867,#2470,.T.);
#17285=EDGE_CURVE('',#13867,#13868,#2471,.T.);
#17286=EDGE_CURVE('',#13868,#13857,#2472,.T.);
#17287=EDGE_CURVE('',#13869,#13870,#2473,.T.);
#17288=EDGE_CURVE('',#13871,#13869,#8666,.T.);
#17289=EDGE_CURVE('',#13872,#13871,#8667,.T.);
#17290=EDGE_CURVE('',#13872,#13870,#8668,.T.);
#17291=EDGE_CURVE('',#13873,#13869,#2474,.T.);
#17292=EDGE_CURVE('',#13874,#13873,#8669,.T.);
#17293=EDGE_CURVE('',#13871,#13874,#8670,.T.);
#17294=EDGE_CURVE('',#13828,#13830,#2475,.T.);
#17295=EDGE_CURVE('',#13875,#13875,#2476,.T.);
#17296=EDGE_CURVE('',#13875,#13829,#8671,.T.);
#17297=EDGE_CURVE('',#13854,#13855,#2477,.T.);
#17298=EDGE_CURVE('',#13856,#13876,#8672,.T.);
#17299=EDGE_CURVE('',#13876,#13876,#2478,.T.);
#17300=EDGE_CURVE('',#13877,#13878,#2479,.T.);
#17301=EDGE_CURVE('',#13879,#13877,#8673,.T.);
#17302=EDGE_CURVE('',#13880,#13879,#8674,.T.);
#17303=EDGE_CURVE('',#13880,#13878,#8675,.T.);
#17304=EDGE_CURVE('',#13881,#13877,#2480,.T.);
#17305=EDGE_CURVE('',#13882,#13881,#8676,.T.);
#17306=EDGE_CURVE('',#13879,#13882,#8677,.T.);
#17307=EDGE_CURVE('',#13883,#13881,#2481,.T.);
#17308=EDGE_CURVE('',#13884,#13883,#8678,.T.);
#17309=EDGE_CURVE('',#13882,#13884,#8679,.T.);
#17310=EDGE_CURVE('',#13885,#13883,#2482,.T.);
#17311=EDGE_CURVE('',#13886,#13885,#8680,.T.);
#17312=EDGE_CURVE('',#13884,#13886,#8681,.T.);
#17313=EDGE_CURVE('',#13887,#13885,#2483,.T.);
#17314=EDGE_CURVE('',#13888,#13887,#8682,.T.);
#17315=EDGE_CURVE('',#13886,#13888,#8683,.T.);
#17316=EDGE_CURVE('',#13889,#13887,#2484,.T.);
#17317=EDGE_CURVE('',#13890,#13889,#8684,.T.);
#17318=EDGE_CURVE('',#13888,#13890,#8685,.T.);
#17319=EDGE_CURVE('',#13891,#13889,#2485,.T.);
#17320=EDGE_CURVE('',#13892,#13891,#8686,.T.);
#17321=EDGE_CURVE('',#13890,#13892,#8687,.T.);
#17322=EDGE_CURVE('',#13893,#13891,#2486,.T.);
#17323=EDGE_CURVE('',#13894,#13893,#8688,.T.);
#17324=EDGE_CURVE('',#13892,#13894,#8689,.T.);
#17325=EDGE_CURVE('',#13895,#13893,#2487,.T.);
#17326=EDGE_CURVE('',#13896,#13895,#8690,.T.);
#17327=EDGE_CURVE('',#13894,#13896,#8691,.T.);
#17328=EDGE_CURVE('',#13897,#13895,#2488,.T.);
#17329=EDGE_CURVE('',#13898,#13897,#8692,.T.);
#17330=EDGE_CURVE('',#13896,#13898,#8693,.T.);
#17331=EDGE_CURVE('',#13899,#13897,#2489,.T.);
#17332=EDGE_CURVE('',#13900,#13899,#8694,.T.);
#17333=EDGE_CURVE('',#13898,#13900,#8695,.T.);
#17334=EDGE_CURVE('',#13878,#13899,#2490,.T.);
#17335=EDGE_CURVE('',#13900,#13880,#8696,.T.);
#17336=EDGE_CURVE('',#13844,#13901,#808,.T.);
#17337=EDGE_CURVE('',#13818,#13901,#8697,.T.);
#17338=EDGE_CURVE('',#13902,#13903,#2491,.T.);
#17339=EDGE_CURVE('',#13904,#13902,#8698,.T.);
#17340=EDGE_CURVE('',#13904,#13905,#2492,.T.);
#17341=EDGE_CURVE('',#13905,#13903,#8699,.T.);
#17342=EDGE_CURVE('',#13903,#13906,#8700,.T.);
#17343=EDGE_CURVE('',#13905,#13907,#8701,.T.);
#17344=EDGE_CURVE('',#13907,#13906,#8702,.T.);
#17345=EDGE_CURVE('',#13906,#13908,#2493,.T.);
#17346=EDGE_CURVE('',#13907,#13909,#2494,.T.);
#17347=EDGE_CURVE('',#13909,#13908,#8703,.T.);
#17348=EDGE_CURVE('',#13908,#13910,#8704,.T.);
#17349=EDGE_CURVE('',#13909,#13911,#8705,.T.);
#17350=EDGE_CURVE('',#13911,#13910,#8706,.T.);
#17351=EDGE_CURVE('',#13910,#13912,#2495,.T.);
#17352=EDGE_CURVE('',#13911,#13913,#2496,.T.);
#17353=EDGE_CURVE('',#13913,#13912,#8707,.T.);
#17354=EDGE_CURVE('',#13912,#13914,#8708,.T.);
#17355=EDGE_CURVE('',#13913,#13915,#8709,.T.);
#17356=EDGE_CURVE('',#13915,#13914,#8710,.T.);
#17357=EDGE_CURVE('',#13914,#13916,#2497,.T.);
#17358=EDGE_CURVE('',#13915,#13917,#2498,.T.);
#17359=EDGE_CURVE('',#13917,#13916,#8711,.T.);
#17360=EDGE_CURVE('',#13916,#13902,#8712,.T.);
#17361=EDGE_CURVE('',#13917,#13904,#8713,.T.);
#17362=EDGE_CURVE('',#13918,#13919,#8714,.T.);
#17363=EDGE_CURVE('',#13919,#13920,#8715,.T.);
#17364=EDGE_CURVE('',#13921,#13920,#8716,.T.);
#17365=EDGE_CURVE('',#13918,#13921,#8717,.T.);
#17366=EDGE_CURVE('',#13922,#13922,#2499,.T.);
#17367=EDGE_CURVE('',#13923,#13923,#2500,.T.);
#17368=EDGE_CURVE('',#13924,#13925,#8718,.T.);
#17369=EDGE_CURVE('',#13925,#13926,#2501,.T.);
#17370=EDGE_CURVE('',#13926,#13927,#8719,.T.);
#17371=EDGE_CURVE('',#13927,#13928,#2502,.T.);
#17372=EDGE_CURVE('',#13928,#13929,#8720,.T.);
#17373=EDGE_CURVE('',#13929,#13930,#2503,.T.);
#17374=EDGE_CURVE('',#13930,#13931,#8721,.T.);
#17375=EDGE_CURVE('',#13931,#13924,#2504,.T.);
#17376=EDGE_CURVE('',#13932,#13925,#8722,.T.);
#17377=EDGE_CURVE('',#13932,#13933,#2505,.T.);
#17378=EDGE_CURVE('',#13933,#13926,#8723,.T.);
#17379=EDGE_CURVE('',#13933,#13934,#8724,.T.);
#17380=EDGE_CURVE('',#13934,#13927,#8725,.T.);
#17381=EDGE_CURVE('',#13934,#13935,#2506,.T.);
#17382=EDGE_CURVE('',#13935,#13928,#8726,.T.);
#17383=EDGE_CURVE('',#13935,#13936,#8727,.T.);
#17384=EDGE_CURVE('',#13936,#13929,#8728,.T.);
#17385=EDGE_CURVE('',#13936,#13937,#2507,.T.);
#17386=EDGE_CURVE('',#13937,#13930,#8729,.T.);
#17387=EDGE_CURVE('',#13937,#13938,#8730,.T.);
#17388=EDGE_CURVE('',#13938,#13931,#8731,.T.);
#17389=EDGE_CURVE('',#13938,#13939,#2508,.T.);
#17390=EDGE_CURVE('',#13939,#13924,#8732,.T.);
#17391=EDGE_CURVE('',#13939,#13932,#8733,.T.);
#17392=EDGE_CURVE('',#13940,#13940,#2509,.T.);
#17393=EDGE_CURVE('',#13941,#13942,#2510,.T.);
#17394=EDGE_CURVE('',#13942,#13943,#2511,.T.);
#17395=EDGE_CURVE('',#13943,#13944,#2512,.T.);
#17396=EDGE_CURVE('',#13944,#13945,#2513,.T.);
#17397=EDGE_CURVE('',#13945,#13946,#2514,.T.);
#17398=EDGE_CURVE('',#13946,#13947,#2515,.T.);
#17399=EDGE_CURVE('',#13947,#13948,#2516,.T.);
#17400=EDGE_CURVE('',#13948,#13949,#2517,.T.);
#17401=EDGE_CURVE('',#13949,#13950,#2518,.T.);
#17402=EDGE_CURVE('',#13950,#13951,#2519,.T.);
#17403=EDGE_CURVE('',#13951,#13952,#2520,.T.);
#17404=EDGE_CURVE('',#13952,#13941,#2521,.T.);
#17405=EDGE_CURVE('',#13940,#13923,#8734,.T.);
#17406=EDGE_CURVE('',#13953,#13953,#2522,.T.);
#17407=EDGE_CURVE('',#13954,#13955,#2523,.T.);
#17408=EDGE_CURVE('',#13955,#13956,#2524,.T.);
#17409=EDGE_CURVE('',#13956,#13957,#2525,.T.);
#17410=EDGE_CURVE('',#13957,#13958,#2526,.T.);
#17411=EDGE_CURVE('',#13958,#13959,#2527,.T.);
#17412=EDGE_CURVE('',#13959,#13960,#2528,.T.);
#17413=EDGE_CURVE('',#13960,#13961,#2529,.T.);
#17414=EDGE_CURVE('',#13961,#13962,#2530,.T.);
#17415=EDGE_CURVE('',#13962,#13963,#2531,.T.);
#17416=EDGE_CURVE('',#13963,#13964,#2532,.T.);
#17417=EDGE_CURVE('',#13964,#13965,#2533,.T.);
#17418=EDGE_CURVE('',#13965,#13954,#2534,.T.);
#17419=EDGE_CURVE('',#13953,#13922,#8735,.T.);
#17420=EDGE_CURVE('',#13966,#13964,#8736,.T.);
#17421=EDGE_CURVE('',#13966,#13967,#8737,.T.);
#17422=EDGE_CURVE('',#13967,#13965,#8738,.T.);
#17423=EDGE_CURVE('',#13967,#13968,#8739,.T.);
#17424=EDGE_CURVE('',#13968,#13954,#8740,.T.);
#17425=EDGE_CURVE('',#13968,#13969,#8741,.T.);
#17426=EDGE_CURVE('',#13969,#13955,#8742,.T.);
#17427=EDGE_CURVE('',#13969,#13970,#8743,.T.);
#17428=EDGE_CURVE('',#13970,#13956,#8744,.T.);
#17429=EDGE_CURVE('',#13970,#13971,#8745,.T.);
#17430=EDGE_CURVE('',#13971,#13957,#8746,.T.);
#17431=EDGE_CURVE('',#13971,#13972,#8747,.T.);
#17432=EDGE_CURVE('',#13972,#13958,#8748,.T.);
#17433=EDGE_CURVE('',#13972,#13973,#8749,.T.);
#17434=EDGE_CURVE('',#13973,#13959,#8750,.T.);
#17435=EDGE_CURVE('',#13973,#13974,#8751,.T.);
#17436=EDGE_CURVE('',#13974,#13960,#8752,.T.);
#17437=EDGE_CURVE('',#13974,#13975,#8753,.T.);
#17438=EDGE_CURVE('',#13975,#13961,#8754,.T.);
#17439=EDGE_CURVE('',#13975,#13976,#8755,.T.);
#17440=EDGE_CURVE('',#13976,#13962,#8756,.T.);
#17441=EDGE_CURVE('',#13976,#13977,#8757,.T.);
#17442=EDGE_CURVE('',#13977,#13963,#8758,.T.);
#17443=EDGE_CURVE('',#13977,#13966,#8759,.T.);
#17444=EDGE_CURVE('',#13978,#13951,#8760,.T.);
#17445=EDGE_CURVE('',#13978,#13979,#8761,.T.);
#17446=EDGE_CURVE('',#13979,#13952,#8762,.T.);
#17447=EDGE_CURVE('',#13979,#13980,#8763,.T.);
#17448=EDGE_CURVE('',#13980,#13941,#8764,.T.);
#17449=EDGE_CURVE('',#13980,#13981,#8765,.T.);
#17450=EDGE_CURVE('',#13981,#13942,#8766,.T.);
#17451=EDGE_CURVE('',#13981,#13982,#8767,.T.);
#17452=EDGE_CURVE('',#13982,#13943,#8768,.T.);
#17453=EDGE_CURVE('',#13982,#13983,#8769,.T.);
#17454=EDGE_CURVE('',#13983,#13944,#8770,.T.);
#17455=EDGE_CURVE('',#13983,#13984,#8771,.T.);
#17456=EDGE_CURVE('',#13984,#13945,#8772,.T.);
#17457=EDGE_CURVE('',#13984,#13985,#8773,.T.);
#17458=EDGE_CURVE('',#13985,#13946,#8774,.T.);
#17459=EDGE_CURVE('',#13985,#13986,#8775,.T.);
#17460=EDGE_CURVE('',#13986,#13947,#8776,.T.);
#17461=EDGE_CURVE('',#13986,#13987,#8777,.T.);
#17462=EDGE_CURVE('',#13987,#13948,#8778,.T.);
#17463=EDGE_CURVE('',#13987,#13988,#8779,.T.);
#17464=EDGE_CURVE('',#13988,#13949,#8780,.T.);
#17465=EDGE_CURVE('',#13988,#13989,#8781,.T.);
#17466=EDGE_CURVE('',#13989,#13950,#8782,.T.);
#17467=EDGE_CURVE('',#13989,#13978,#8783,.T.);
#17468=EDGE_CURVE('',#13811,#13990,#8784,.T.);
#17469=EDGE_CURVE('',#13990,#13991,#8785,.T.);
#17470=EDGE_CURVE('',#13991,#13992,#8786,.T.);
#17471=EDGE_CURVE('',#13992,#13993,#8787,.T.);
#17472=EDGE_CURVE('',#13993,#13994,#8788,.T.);
#17473=EDGE_CURVE('',#13994,#13995,#8789,.T.);
#17474=EDGE_CURVE('',#13995,#13996,#8790,.T.);
#17475=EDGE_CURVE('',#13996,#13997,#8791,.T.);
#17476=EDGE_CURVE('',#13997,#13814,#8792,.T.);
#17477=EDGE_CURVE('',#13997,#13805,#8793,.T.);
#17478=EDGE_CURVE('',#13996,#13806,#8794,.T.);
#17479=EDGE_CURVE('',#13995,#13807,#8795,.T.);
#17480=EDGE_CURVE('',#13994,#13808,#8796,.T.);
#17481=EDGE_CURVE('',#13993,#13809,#8797,.T.);
#17482=EDGE_CURVE('',#13992,#13810,#8798,.T.);
#17483=EDGE_CURVE('',#13991,#13796,#8799,.T.);
#17484=EDGE_CURVE('',#13990,#13800,#8800,.T.);
#17485=EDGE_CURVE('',#13998,#13999,#809,.T.);
#17486=EDGE_CURVE('',#13826,#13998,#8801,.T.);
#17487=EDGE_CURVE('',#13999,#13825,#8802,.T.);
#17488=EDGE_CURVE('',#14000,#13824,#8803,.T.);
#17489=EDGE_CURVE('',#13999,#14000,#8804,.T.);
#17490=EDGE_CURVE('',#14000,#13831,#2535,.T.);
#17491=EDGE_CURVE('',#13832,#13843,#2536,.T.);
#17492=EDGE_CURVE('',#14001,#13851,#8805,.T.);
#17493=EDGE_CURVE('',#14002,#14001,#810,.T.);
#17494=EDGE_CURVE('',#13852,#14002,#8806,.T.);
#17495=EDGE_CURVE('',#13819,#13918,#8807,.T.);
#17496=EDGE_CURVE('',#13921,#13853,#8808,.T.);
#17497=EDGE_CURVE('',#13901,#14002,#2537,.T.);
#17498=EDGE_CURVE('',#13838,#13998,#2538,.T.);
#17499=EDGE_CURVE('',#13920,#13849,#8809,.T.);
#17500=EDGE_CURVE('',#13827,#13919,#8810,.T.);
#17501=EDGE_CURVE('',#13835,#13841,#2539,.T.);
#17502=EDGE_CURVE('',#14003,#13836,#2540,.T.);
#17503=EDGE_CURVE('',#14003,#13850,#8811,.T.);
#17504=EDGE_CURVE('',#14001,#14003,#8812,.T.);
#17505=EDGE_CURVE('',#14004,#14004,#2541,.T.);
#17506=EDGE_CURVE('',#14005,#13867,#8813,.T.);
#17507=EDGE_CURVE('',#14006,#14005,#8814,.T.);
#17508=EDGE_CURVE('',#14006,#13868,#8815,.T.);
#17509=EDGE_CURVE('',#14007,#14006,#8816,.T.);
#17510=EDGE_CURVE('',#14007,#13857,#8817,.T.);
#17511=EDGE_CURVE('',#14008,#13866,#8818,.T.);
#17512=EDGE_CURVE('',#14005,#14008,#8819,.T.);
#17513=EDGE_CURVE('',#14009,#14007,#8820,.T.);
#17514=EDGE_CURVE('',#14009,#13858,#8821,.T.);
#17515=EDGE_CURVE('',#14010,#14009,#8822,.T.);
#17516=EDGE_CURVE('',#14010,#13859,#8823,.T.);
#17517=EDGE_CURVE('',#14011,#14010,#8824,.T.);
#17518=EDGE_CURVE('',#14011,#13860,#8825,.T.);
#17519=EDGE_CURVE('',#14012,#14011,#8826,.T.);
#17520=EDGE_CURVE('',#14012,#13861,#8827,.T.);
#17521=EDGE_CURVE('',#14013,#14012,#8828,.T.);
#17522=EDGE_CURVE('',#14013,#13862,#8829,.T.);
#17523=EDGE_CURVE('',#14014,#14013,#8830,.T.);
#17524=EDGE_CURVE('',#14014,#13863,#8831,.T.);
#17525=EDGE_CURVE('',#14015,#14014,#8832,.T.);
#17526=EDGE_CURVE('',#14015,#13864,#8833,.T.);
#17527=EDGE_CURVE('',#14016,#14015,#8834,.T.);
#17528=EDGE_CURVE('',#14016,#13865,#8835,.T.);
#17529=EDGE_CURVE('',#14004,#14017,#8836,.T.);
#17530=EDGE_CURVE('',#14017,#14017,#2542,.T.);
#17531=EDGE_CURVE('',#14008,#14016,#8837,.T.);
#17532=EDGE_CURVE('',#13870,#14018,#2543,.T.);
#17533=EDGE_CURVE('',#14018,#14019,#2544,.T.);
#17534=EDGE_CURVE('',#14019,#14020,#2545,.T.);
#17535=EDGE_CURVE('',#14020,#14021,#2546,.T.);
#17536=EDGE_CURVE('',#14021,#14022,#2547,.T.);
#17537=EDGE_CURVE('',#14022,#14023,#2548,.T.);
#17538=EDGE_CURVE('',#14023,#14024,#2549,.T.);
#17539=EDGE_CURVE('',#14024,#14025,#2550,.T.);
#17540=EDGE_CURVE('',#14025,#14026,#2551,.T.);
#17541=EDGE_CURVE('',#14026,#13873,#2552,.T.);
#17542=EDGE_CURVE('',#13874,#14027,#8838,.T.);
#17543=EDGE_CURVE('',#14027,#14028,#8839,.T.);
#17544=EDGE_CURVE('',#14028,#14029,#8840,.T.);
#17545=EDGE_CURVE('',#14029,#14030,#8841,.T.);
#17546=EDGE_CURVE('',#14030,#14031,#8842,.T.);
#17547=EDGE_CURVE('',#14031,#14032,#8843,.T.);
#17548=EDGE_CURVE('',#14032,#14033,#8844,.T.);
#17549=EDGE_CURVE('',#14033,#14034,#8845,.T.);
#17550=EDGE_CURVE('',#14034,#14035,#8846,.T.);
#17551=EDGE_CURVE('',#14035,#13872,#8847,.T.);
#17552=EDGE_CURVE('',#14035,#14018,#8848,.T.);
#17553=EDGE_CURVE('',#14034,#14019,#8849,.T.);
#17554=EDGE_CURVE('',#14033,#14020,#8850,.T.);
#17555=EDGE_CURVE('',#14032,#14021,#8851,.T.);
#17556=EDGE_CURVE('',#14031,#14022,#8852,.T.);
#17557=EDGE_CURVE('',#14030,#14023,#8853,.T.);
#17558=EDGE_CURVE('',#14029,#14024,#8854,.T.);
#17559=EDGE_CURVE('',#14028,#14025,#8855,.T.);
#17560=EDGE_CURVE('',#14027,#14026,#8856,.T.);
#17561=EDGE_CURVE('',#14036,#14036,#2553,.T.);
#17562=EDGE_CURVE('',#14037,#14037,#2554,.T.);
#17563=EDGE_CURVE('',#14038,#14039,#811,.T.);
#17564=EDGE_CURVE('',#14039,#14040,#8857,.T.);
#17565=EDGE_CURVE('',#14041,#14040,#2555,.T.);
#17566=EDGE_CURVE('',#14040,#14041,#2556,.T.);
#17567=EDGE_CURVE('',#14039,#14038,#812,.T.);
#17568=EDGE_CURVE('',#14042,#14043,#2557,.T.);
#17569=EDGE_CURVE('',#14043,#14042,#2558,.T.);
#17570=EDGE_CURVE('',#14044,#14045,#813,.T.);
#17571=EDGE_CURVE('',#14045,#14046,#8858,.T.);
#17572=EDGE_CURVE('',#14047,#14046,#2559,.T.);
#17573=EDGE_CURVE('',#14046,#14047,#2560,.T.);
#17574=EDGE_CURVE('',#14045,#14044,#814,.T.);
#17575=EDGE_CURVE('',#14048,#14049,#2561,.T.);
#17576=EDGE_CURVE('',#14050,#14048,#510,.T.);
#17577=EDGE_CURVE('',#14049,#14050,#2562,.T.);
#17578=EDGE_CURVE('',#14051,#14052,#815,.T.);
#17579=EDGE_CURVE('',#14052,#14053,#8859,.T.);
#17580=EDGE_CURVE('',#14053,#14053,#2563,.T.);
#17581=EDGE_CURVE('',#14052,#14051,#816,.T.);
#17582=EDGE_CURVE('',#14049,#14053,#2564,.T.);
#17583=EDGE_CURVE('',#14054,#14055,#2565,.T.);
#17584=EDGE_CURVE('',#14055,#14054,#2566,.T.);
#17585=EDGE_CURVE('',#14055,#14041,#2567,.T.);
#17586=EDGE_CURVE('',#14043,#14047,#2568,.T.);
#17587=EDGE_CURVE('',#14056,#14057,#2569,.T.);
#17588=EDGE_CURVE('',#14057,#14056,#2570,.T.);
#17589=EDGE_CURVE('',#14057,#14058,#2571,.T.);
#17590=EDGE_CURVE('',#14058,#14058,#2572,.T.);
#17591=EDGE_CURVE('',#14056,#14036,#8860,.T.);
#17592=EDGE_CURVE('',#14059,#14059,#2573,.T.);
#17593=EDGE_CURVE('',#14037,#14060,#8861,.T.);
#17594=EDGE_CURVE('',#14061,#14060,#2574,.T.);
#17595=EDGE_CURVE('',#14060,#14061,#2575,.T.);
#17596=EDGE_CURVE('',#14062,#14063,#2576,.T.);
#17597=EDGE_CURVE('',#14064,#14063,#8862,.T.);
#17598=EDGE_CURVE('',#14065,#14064,#8863,.T.);
#17599=EDGE_CURVE('',#14065,#14062,#8864,.T.);
#17600=EDGE_CURVE('',#14064,#14066,#8865,.T.);
#17601=EDGE_CURVE('',#14066,#14067,#8866,.T.);
#17602=EDGE_CURVE('',#14067,#14068,#8867,.T.);
#17603=EDGE_CURVE('',#14068,#14069,#8868,.T.);
#17604=EDGE_CURVE('',#14069,#14070,#8869,.T.);
#17605=EDGE_CURVE('',#14070,#14071,#8870,.T.);
#17606=EDGE_CURVE('',#14071,#14072,#8871,.T.);
#17607=EDGE_CURVE('',#14072,#14073,#8872,.T.);
#17608=EDGE_CURVE('',#14073,#14074,#8873,.T.);
#17609=EDGE_CURVE('',#14074,#14075,#8874,.T.);
#17610=EDGE_CURVE('',#14075,#14076,#8875,.T.);
#17611=EDGE_CURVE('',#14076,#14077,#8876,.T.);
#17612=EDGE_CURVE('',#14077,#14078,#8877,.T.);
#17613=EDGE_CURVE('',#14078,#14079,#8878,.T.);
#17614=EDGE_CURVE('',#14079,#14065,#8879,.T.);
#17615=EDGE_CURVE('',#14080,#14062,#2577,.T.);
#17616=EDGE_CURVE('',#14079,#14080,#8880,.T.);
#17617=EDGE_CURVE('',#14081,#14082,#8881,.T.);
#17618=EDGE_CURVE('',#14081,#14083,#8882,.T.);
#17619=EDGE_CURVE('',#14083,#14084,#8883,.T.);
#17620=EDGE_CURVE('',#14085,#14084,#8884,.T.);
#17621=EDGE_CURVE('',#14085,#14086,#8885,.T.);
#17622=EDGE_CURVE('',#14082,#14086,#8886,.T.);
#17623=EDGE_CURVE('',#14087,#14088,#8887,.T.);
#17624=EDGE_CURVE('',#14088,#14089,#8888,.T.);
#17625=EDGE_CURVE('',#14089,#14090,#8889,.T.);
#17626=EDGE_CURVE('',#14091,#14090,#8890,.T.);
#17627=EDGE_CURVE('',#14092,#14091,#8891,.T.);
#17628=EDGE_CURVE('',#14087,#14092,#8892,.T.);
#17629=EDGE_CURVE('',#14093,#14094,#8893,.T.);
#17630=EDGE_CURVE('',#14094,#14095,#2578,.T.);
#17631=EDGE_CURVE('',#14095,#14096,#8894,.T.);
#17632=EDGE_CURVE('',#14096,#14093,#2579,.T.);
#17633=EDGE_CURVE('',#14097,#14098,#2580,.T.);
#17634=EDGE_CURVE('',#14097,#14099,#8895,.T.);
#17635=EDGE_CURVE('',#14099,#14100,#2581,.T.);
#17636=EDGE_CURVE('',#14100,#14098,#8896,.T.);
#17637=EDGE_CURVE('',#14101,#14102,#2582,.T.);
#17638=EDGE_CURVE('',#14093,#14101,#8897,.T.);
#17639=EDGE_CURVE('',#14096,#14102,#8898,.T.);
#17640=EDGE_CURVE('',#14102,#14103,#8899,.T.);
#17641=EDGE_CURVE('',#14095,#14103,#8900,.T.);
#17642=EDGE_CURVE('',#14103,#14104,#2583,.T.);
#17643=EDGE_CURVE('',#14094,#14104,#8901,.T.);
#17644=EDGE_CURVE('',#14104,#14101,#8902,.T.);
#17645=EDGE_CURVE('',#14105,#14106,#8903,.T.);
#17646=EDGE_CURVE('',#14106,#14107,#2584,.T.);
#17647=EDGE_CURVE('',#14107,#14108,#8904,.T.);
#17648=EDGE_CURVE('',#14108,#14105,#2585,.T.);
#17649=EDGE_CURVE('',#14087,#14084,#2586,.T.);
#17650=EDGE_CURVE('',#14092,#14085,#2587,.T.);
#17651=EDGE_CURVE('',#14109,#14110,#2588,.T.);
#17652=EDGE_CURVE('',#14105,#14109,#8905,.T.);
#17653=EDGE_CURVE('',#14108,#14110,#8906,.T.);
#17654=EDGE_CURVE('',#14110,#14111,#8907,.T.);
#17655=EDGE_CURVE('',#14107,#14111,#8908,.T.);
#17656=EDGE_CURVE('',#14111,#14112,#2589,.T.);
#17657=EDGE_CURVE('',#14106,#14112,#8909,.T.);
#17658=EDGE_CURVE('',#14112,#14109,#8910,.T.);
#17659=EDGE_CURVE('',#14113,#14113,#2590,.T.);
#17660=EDGE_CURVE('',#14113,#14114,#8911,.T.);
#17661=EDGE_CURVE('',#14115,#14114,#2591,.T.);
#17662=EDGE_CURVE('',#14114,#14115,#2592,.T.);
#17663=EDGE_CURVE('',#14115,#14116,#8912,.T.);
#17664=EDGE_CURVE('',#14116,#14116,#2593,.T.);
#17665=EDGE_CURVE('',#14117,#14117,#2594,.T.);
#17666=EDGE_CURVE('',#14117,#14118,#8913,.T.);
#17667=EDGE_CURVE('',#14119,#14118,#2595,.T.);
#17668=EDGE_CURVE('',#14118,#14119,#2596,.T.);
#17669=EDGE_CURVE('',#14119,#14120,#8914,.T.);
#17670=EDGE_CURVE('',#14120,#14120,#2597,.T.);
#17671=EDGE_CURVE('',#14121,#14121,#2598,.T.);
#17672=EDGE_CURVE('',#14121,#14122,#8915,.T.);
#17673=EDGE_CURVE('',#14123,#14122,#2599,.T.);
#17674=EDGE_CURVE('',#14122,#14123,#2600,.T.);
#17675=EDGE_CURVE('',#14123,#14124,#8916,.T.);
#17676=EDGE_CURVE('',#14124,#14124,#2601,.T.);
#17677=EDGE_CURVE('',#14125,#14125,#2602,.T.);
#17678=EDGE_CURVE('',#14125,#14126,#8917,.T.);
#17679=EDGE_CURVE('',#14127,#14126,#2603,.T.);
#17680=EDGE_CURVE('',#14126,#14127,#2604,.T.);
#17681=EDGE_CURVE('',#14127,#14128,#8918,.T.);
#17682=EDGE_CURVE('',#14128,#14128,#2605,.T.);
#17683=EDGE_CURVE('',#14061,#14129,#8919,.T.);
#17684=EDGE_CURVE('',#14129,#14129,#2606,.T.);
#17685=EDGE_CURVE('',#14130,#14130,#2607,.T.);
#17686=EDGE_CURVE('',#14131,#14131,#2608,.T.);
#17687=EDGE_CURVE('',#14132,#14132,#2609,.T.);
#17688=EDGE_CURVE('',#14133,#14133,#2610,.T.);
#17689=EDGE_CURVE('',#14134,#14134,#2611,.T.);
#17690=EDGE_CURVE('',#14134,#14135,#8920,.T.);
#17691=EDGE_CURVE('',#14135,#14135,#2612,.T.);
#17692=EDGE_CURVE('',#14136,#14136,#2613,.T.);
#17693=EDGE_CURVE('',#14136,#14137,#8921,.T.);
#17694=EDGE_CURVE('',#14137,#14137,#2614,.T.);
#17695=EDGE_CURVE('',#14138,#14138,#2615,.T.);
#17696=EDGE_CURVE('',#14138,#14139,#8922,.T.);
#17697=EDGE_CURVE('',#14139,#14139,#2616,.T.);
#17698=EDGE_CURVE('',#14140,#14140,#2617,.T.);
#17699=EDGE_CURVE('',#14140,#14059,#8923,.T.);
#17700=EDGE_CURVE('',#14141,#14141,#2618,.T.);
#17701=EDGE_CURVE('',#14142,#14142,#2619,.T.);
#17702=EDGE_CURVE('',#14130,#14141,#8924,.T.);
#17703=EDGE_CURVE('',#14142,#14143,#8925,.T.);
#17704=EDGE_CURVE('',#14143,#14143,#2620,.T.);
#17705=EDGE_CURVE('',#14144,#14144,#2621,.T.);
#17706=EDGE_CURVE('',#14144,#14133,#8926,.T.);
#17707=EDGE_CURVE('',#14145,#14145,#2622,.T.);
#17708=EDGE_CURVE('',#14146,#14146,#2623,.T.);
#17709=EDGE_CURVE('',#14146,#14145,#8927,.T.);
#17710=EDGE_CURVE('',#14147,#14147,#2624,.T.);
#17711=EDGE_CURVE('',#14148,#14148,#2625,.T.);
#17712=EDGE_CURVE('',#14148,#14147,#8928,.T.);
#17713=EDGE_CURVE('',#14149,#14149,#2626,.T.);
#17714=EDGE_CURVE('',#14132,#14149,#8929,.T.);
#17715=EDGE_CURVE('',#14150,#14150,#2627,.T.);
#17716=EDGE_CURVE('',#14150,#14131,#8930,.T.);
#17717=EDGE_CURVE('',#14151,#14151,#2628,.T.);
#17718=EDGE_CURVE('',#14152,#14152,#2629,.T.);
#17719=EDGE_CURVE('',#14152,#14151,#8931,.T.);
#17720=EDGE_CURVE('',#14153,#14154,#8932,.T.);
#17721=EDGE_CURVE('',#14153,#14155,#8933,.T.);
#17722=EDGE_CURVE('',#14155,#14098,#8934,.T.);
#17723=EDGE_CURVE('',#14100,#14156,#8935,.T.);
#17724=EDGE_CURVE('',#14154,#14156,#8936,.T.);
#17725=EDGE_CURVE('',#14157,#14158,#8937,.T.);
#17726=EDGE_CURVE('',#14157,#14153,#2630,.T.);
#17727=EDGE_CURVE('',#14158,#14154,#2631,.T.);
#17728=EDGE_CURVE('',#14097,#14159,#8938,.T.);
#17729=EDGE_CURVE('',#14159,#14157,#8939,.T.);
#17730=EDGE_CURVE('',#14160,#14158,#8940,.T.);
#17731=EDGE_CURVE('',#14099,#14160,#8941,.T.);
#17732=EDGE_CURVE('',#14086,#14091,#2632,.T.);
#17733=EDGE_CURVE('',#14090,#14082,#2633,.T.);
#17734=EDGE_CURVE('',#14161,#14161,#2634,.T.);
#17735=EDGE_CURVE('',#14089,#14081,#2635,.T.);
#17736=EDGE_CURVE('',#14156,#14160,#2636,.T.);
#17737=EDGE_CURVE('',#14162,#14162,#2637,.T.);
#17738=EDGE_CURVE('',#14098,#14097,#2638,.T.);
#17739=EDGE_CURVE('',#14155,#14159,#2639,.T.);
#17740=EDGE_CURVE('',#14162,#14163,#8942,.T.);
#17741=EDGE_CURVE('',#14163,#14163,#2640,.T.);
#17742=EDGE_CURVE('',#14164,#14165,#2641,.T.);
#17743=EDGE_CURVE('',#14166,#14164,#2642,.T.);
#17744=EDGE_CURVE('',#14167,#14166,#2643,.T.);
#17745=EDGE_CURVE('',#14168,#14167,#2644,.T.);
#17746=EDGE_CURVE('',#14169,#14168,#2645,.T.);
#17747=EDGE_CURVE('',#14170,#14169,#2646,.T.);
#17748=EDGE_CURVE('',#14171,#14170,#2647,.T.);
#17749=EDGE_CURVE('',#14172,#14171,#2648,.T.);
#17750=EDGE_CURVE('',#14063,#14172,#2649,.T.);
#17751=EDGE_CURVE('',#14173,#14080,#2650,.T.);
#17752=EDGE_CURVE('',#14174,#14173,#2651,.T.);
#17753=EDGE_CURVE('',#14175,#14174,#2652,.T.);
#17754=EDGE_CURVE('',#14176,#14175,#2653,.T.);
#17755=EDGE_CURVE('',#14165,#14176,#2654,.T.);
#17756=EDGE_CURVE('',#14083,#14088,#2655,.T.);
#17757=EDGE_CURVE('',#14177,#14177,#2656,.T.);
#17758=EDGE_CURVE('',#14161,#14177,#8943,.T.);
#17759=EDGE_CURVE('',#14084,#14087,#2657,.T.);
#17760=EDGE_CURVE('',#14178,#14179,#2658,.T.);
#17761=EDGE_CURVE('',#14180,#14178,#2659,.T.);
#17762=EDGE_CURVE('',#14181,#14180,#2660,.T.);
#17763=EDGE_CURVE('',#14182,#14181,#2661,.T.);
#17764=EDGE_CURVE('',#14183,#14182,#2662,.T.);
#17765=EDGE_CURVE('',#14184,#14183,#2663,.T.);
#17766=EDGE_CURVE('',#14185,#14184,#2664,.T.);
#17767=EDGE_CURVE('',#14186,#14185,#2665,.T.);
#17768=EDGE_CURVE('',#14187,#14186,#2666,.T.);
#17769=EDGE_CURVE('',#14188,#14187,#2667,.T.);
#17770=EDGE_CURVE('',#14189,#14188,#2668,.T.);
#17771=EDGE_CURVE('',#14190,#14189,#2669,.T.);
#17772=EDGE_CURVE('',#14191,#14190,#2670,.T.);
#17773=EDGE_CURVE('',#14192,#14191,#2671,.T.);
#17774=EDGE_CURVE('',#14193,#14192,#2672,.T.);
#17775=EDGE_CURVE('',#14179,#14193,#2673,.T.);
#17776=EDGE_CURVE('',#14194,#14187,#8944,.T.);
#17777=EDGE_CURVE('',#14195,#14194,#8945,.T.);
#17778=EDGE_CURVE('',#14195,#14188,#8946,.T.);
#17779=EDGE_CURVE('',#14196,#14186,#8947,.T.);
#17780=EDGE_CURVE('',#14194,#14196,#8948,.T.);
#17781=EDGE_CURVE('',#14197,#14185,#8949,.T.);
#17782=EDGE_CURVE('',#14196,#14197,#8950,.T.);
#17783=EDGE_CURVE('',#14198,#14184,#8951,.T.);
#17784=EDGE_CURVE('',#14197,#14198,#8952,.T.);
#17785=EDGE_CURVE('',#14199,#14183,#8953,.T.);
#17786=EDGE_CURVE('',#14198,#14199,#8954,.T.);
#17787=EDGE_CURVE('',#14200,#14182,#8955,.T.);
#17788=EDGE_CURVE('',#14199,#14200,#8956,.T.);
#17789=EDGE_CURVE('',#14201,#14181,#8957,.T.);
#17790=EDGE_CURVE('',#14200,#14201,#8958,.T.);
#17791=EDGE_CURVE('',#14202,#14180,#8959,.T.);
#17792=EDGE_CURVE('',#14201,#14202,#8960,.T.);
#17793=EDGE_CURVE('',#14203,#14178,#8961,.T.);
#17794=EDGE_CURVE('',#14202,#14203,#8962,.T.);
#17795=EDGE_CURVE('',#14204,#14179,#8963,.T.);
#17796=EDGE_CURVE('',#14203,#14204,#8964,.T.);
#17797=EDGE_CURVE('',#14205,#14193,#8965,.T.);
#17798=EDGE_CURVE('',#14204,#14205,#8966,.T.);
#17799=EDGE_CURVE('',#14206,#14192,#8967,.T.);
#17800=EDGE_CURVE('',#14205,#14206,#8968,.T.);
#17801=EDGE_CURVE('',#14207,#14191,#8969,.T.);
#17802=EDGE_CURVE('',#14206,#14207,#8970,.T.);
#17803=EDGE_CURVE('',#14208,#14190,#8971,.T.);
#17804=EDGE_CURVE('',#14207,#14208,#8972,.T.);
#17805=EDGE_CURVE('',#14209,#14189,#8973,.T.);
#17806=EDGE_CURVE('',#14208,#14209,#8974,.T.);
#17807=EDGE_CURVE('',#14209,#14195,#8975,.T.);
#17808=EDGE_CURVE('',#14066,#14172,#8976,.T.);
#17809=EDGE_CURVE('',#14067,#14171,#8977,.T.);
#17810=EDGE_CURVE('',#14068,#14170,#8978,.T.);
#17811=EDGE_CURVE('',#14069,#14169,#8979,.T.);
#17812=EDGE_CURVE('',#14070,#14168,#8980,.T.);
#17813=EDGE_CURVE('',#14071,#14167,#8981,.T.);
#17814=EDGE_CURVE('',#14072,#14166,#8982,.T.);
#17815=EDGE_CURVE('',#14073,#14164,#8983,.T.);
#17816=EDGE_CURVE('',#14074,#14165,#8984,.T.);
#17817=EDGE_CURVE('',#14075,#14176,#8985,.T.);
#17818=EDGE_CURVE('',#14076,#14175,#8986,.T.);
#17819=EDGE_CURVE('',#14077,#14174,#8987,.T.);
#17820=EDGE_CURVE('',#14078,#14173,#8988,.T.);
#17821=EDGE_CURVE('',#14210,#14211,#2674,.F.);
#17822=EDGE_CURVE('',#14211,#14212,#8989,.T.);
#17823=EDGE_CURVE('',#14212,#14213,#2675,.F.);
#17824=EDGE_CURVE('',#14213,#14210,#8990,.T.);
#17825=EDGE_CURVE('',#14211,#14214,#8991,.T.);
#17826=EDGE_CURVE('',#14214,#14215,#8992,.T.);
#17827=EDGE_CURVE('',#14216,#14215,#8993,.T.);
#17828=EDGE_CURVE('',#14216,#14217,#8994,.T.);
#17829=EDGE_CURVE('',#14217,#14218,#8995,.T.);
#17830=EDGE_CURVE('',#14219,#14218,#8996,.T.);
#17831=EDGE_CURVE('',#14219,#14220,#8997,.T.);
#17832=EDGE_CURVE('',#14220,#14221,#8998,.T.);
#17833=EDGE_CURVE('',#14222,#14221,#8999,.T.);
#17834=EDGE_CURVE('',#14222,#14223,#9000,.T.);
#17835=EDGE_CURVE('',#14223,#14212,#9001,.T.);
#17836=EDGE_CURVE('',#14224,#14224,#2676,.T.);
#17837=EDGE_CURVE('',#14225,#14225,#2677,.T.);
#17838=EDGE_CURVE('',#14226,#14227,#9002,.T.);
#17839=EDGE_CURVE('',#14227,#14228,#9003,.T.);
#17840=EDGE_CURVE('',#14228,#14229,#9004,.T.);
#17841=EDGE_CURVE('',#14229,#14226,#9005,.T.);
#17842=EDGE_CURVE('',#14230,#14230,#2678,.T.);
#17843=EDGE_CURVE('',#14231,#14231,#2679,.T.);
#17844=EDGE_CURVE('',#14221,#14232,#2680,.F.);
#17845=EDGE_CURVE('',#14232,#14233,#9006,.T.);
#17846=EDGE_CURVE('',#14233,#14222,#2681,.F.);
#17847=EDGE_CURVE('',#14233,#14234,#9007,.T.);
#17848=EDGE_CURVE('',#14232,#14235,#9008,.T.);
#17849=EDGE_CURVE('',#14235,#14236,#9009,.T.);
#17850=EDGE_CURVE('',#14237,#14236,#9010,.T.);
#17851=EDGE_CURVE('',#14238,#14237,#9011,.T.);
#17852=EDGE_CURVE('',#14239,#14238,#9012,.T.);
#17853=EDGE_CURVE('',#14240,#14239,#9013,.T.);
#17854=EDGE_CURVE('',#14241,#14240,#9014,.T.);
#17855=EDGE_CURVE('',#14242,#14241,#2682,.T.);
#17856=EDGE_CURVE('',#14243,#14242,#9015,.T.);
#17857=EDGE_CURVE('',#14244,#14243,#9016,.T.);
#17858=EDGE_CURVE('',#14245,#14244,#9017,.T.);
#17859=EDGE_CURVE('',#14245,#14234,#9018,.T.);
#17860=EDGE_CURVE('',#14219,#14246,#2683,.T.);
#17861=EDGE_CURVE('',#14247,#14218,#2684,.T.);
#17862=EDGE_CURVE('',#14247,#14248,#2685,.T.);
#17863=EDGE_CURVE('',#14248,#14249,#9019,.T.);
#17864=EDGE_CURVE('',#14249,#14246,#2686,.T.);
#17865=EDGE_CURVE('',#14250,#14247,#817,.T.);
#17866=EDGE_CURVE('',#14250,#14248,#390,.T.);
#17867=EDGE_CURVE('',#14246,#14251,#818,.T.);
#17868=EDGE_CURVE('',#14249,#14251,#391,.T.);
#17869=EDGE_CURVE('',#14246,#14252,#9020,.T.);
#17870=EDGE_CURVE('',#14252,#14253,#9021,.T.);
#17871=EDGE_CURVE('',#14220,#14253,#9022,.T.);
#17872=EDGE_CURVE('',#14251,#14254,#9023,.T.);
#17873=EDGE_CURVE('',#14237,#14254,#392,.F.);
#17874=EDGE_CURVE('',#14236,#14252,#9024,.T.);
#17875=EDGE_CURVE('',#14255,#14250,#9025,.T.);
#17876=EDGE_CURVE('',#14256,#14255,#9026,.T.);
#17877=EDGE_CURVE('',#14257,#14256,#9027,.T.);
#17878=EDGE_CURVE('',#14254,#14257,#9028,.T.);
#17879=EDGE_CURVE('',#14258,#14216,#2687,.F.);
#17880=EDGE_CURVE('',#14215,#14259,#2688,.F.);
#17881=EDGE_CURVE('',#14259,#14258,#9029,.T.);
#17882=EDGE_CURVE('',#14260,#14256,#2689,.F.);
#17883=EDGE_CURVE('',#14261,#14260,#2690,.F.);
#17884=EDGE_CURVE('',#14256,#14261,#2691,.F.);
#17885=EDGE_CURVE('',#14262,#14257,#2692,.F.);
#17886=EDGE_CURVE('',#14238,#14262,#2693,.F.);
#17887=EDGE_CURVE('',#14257,#14238,#2694,.F.);
#17888=EDGE_CURVE('',#14263,#14264,#2695,.F.);
#17889=EDGE_CURVE('',#14265,#14263,#2696,.F.);
#17890=EDGE_CURVE('',#14264,#14265,#2697,.F.);
#17891=EDGE_CURVE('',#14266,#14267,#2698,.F.);
#17892=EDGE_CURVE('',#14239,#14266,#2699,.F.);
#17893=EDGE_CURVE('',#14267,#14239,#2700,.F.);
#17894=EDGE_CURVE('',#14268,#14269,#2701,.F.);
#17895=EDGE_CURVE('',#14270,#14268,#2702,.F.);
#17896=EDGE_CURVE('',#14269,#14270,#2703,.F.);
#17897=EDGE_CURVE('',#14271,#14272,#2704,.F.);
#17898=EDGE_CURVE('',#14240,#14271,#2705,.F.);
#17899=EDGE_CURVE('',#14272,#14240,#2706,.F.);
#17900=EDGE_CURVE('',#14273,#14274,#2707,.T.);
#17901=EDGE_CURVE('',#14275,#14274,#2708,.T.);
#17902=EDGE_CURVE('',#14276,#14275,#2709,.F.);
#17903=EDGE_CURVE('',#14273,#14276,#2710,.T.);
#17904=EDGE_CURVE('',#14277,#14278,#2711,.F.);
#17905=EDGE_CURVE('',#14242,#14277,#2712,.T.);
#17906=EDGE_CURVE('',#14278,#14241,#2713,.T.);
#17907=EDGE_CURVE('',#14279,#14280,#2714,.F.);
#17908=EDGE_CURVE('',#14281,#14279,#2715,.F.);
#17909=EDGE_CURVE('',#14280,#14281,#2716,.F.);
#17910=EDGE_CURVE('',#14282,#14283,#2717,.F.);
#17911=EDGE_CURVE('',#14284,#14282,#2718,.F.);
#17912=EDGE_CURVE('',#14283,#14284,#2719,.F.);
#17913=EDGE_CURVE('',#14279,#14284,#9030,.T.);
#17914=EDGE_CURVE('',#14282,#14281,#9031,.T.);
#17915=EDGE_CURVE('',#14285,#14286,#2720,.T.);
#17916=EDGE_CURVE('',#14286,#14283,#9032,.T.);
#17917=EDGE_CURVE('',#14284,#14285,#9033,.T.);
#17918=EDGE_CURVE('',#14243,#14287,#2721,.F.);
#17919=EDGE_CURVE('',#14288,#14243,#2722,.F.);
#17920=EDGE_CURVE('',#14287,#14288,#2723,.F.);
#17921=EDGE_CURVE('',#14277,#14288,#9034,.T.);
#17922=EDGE_CURVE('',#14288,#14280,#9035,.T.);
#17923=EDGE_CURVE('',#14281,#14287,#9036,.T.);
#17924=EDGE_CURVE('',#14289,#14290,#2724,.F.);
#17925=EDGE_CURVE('',#14244,#14289,#2725,.F.);
#17926=EDGE_CURVE('',#14290,#14244,#2726,.F.);
#17927=EDGE_CURVE('',#14291,#14245,#2727,.T.);
#17928=EDGE_CURVE('',#14289,#14291,#9037,.T.);
#17929=EDGE_CURVE('',#14287,#14290,#9038,.T.);
#17930=EDGE_CURVE('',#14290,#14282,#9039,.T.);
#17931=EDGE_CURVE('',#14283,#14289,#9040,.T.);
#17932=EDGE_CURVE('',#14274,#14279,#9041,.T.);
#17933=EDGE_CURVE('',#14280,#14275,#9042,.T.);
#17934=EDGE_CURVE('',#14271,#14278,#9043,.T.);
#17935=EDGE_CURVE('',#14278,#14276,#9044,.T.);
#17936=EDGE_CURVE('',#14275,#14277,#9045,.T.);
#17937=EDGE_CURVE('',#14268,#14273,#9046,.T.);
#17938=EDGE_CURVE('',#14276,#14270,#9047,.T.);
#17939=EDGE_CURVE('',#14266,#14272,#9048,.T.);
#17940=EDGE_CURVE('',#14272,#14269,#9049,.T.);
#17941=EDGE_CURVE('',#14270,#14271,#9050,.T.);
#17942=EDGE_CURVE('',#14263,#14268,#9051,.T.);
#17943=EDGE_CURVE('',#14269,#14265,#9052,.T.);
#17944=EDGE_CURVE('',#14262,#14267,#9053,.T.);
#17945=EDGE_CURVE('',#14267,#14264,#9054,.T.);
#17946=EDGE_CURVE('',#14265,#14266,#9055,.T.);
#17947=EDGE_CURVE('',#14260,#14263,#9056,.T.);
#17948=EDGE_CURVE('',#14264,#14261,#9057,.T.);
#17949=EDGE_CURVE('',#14261,#14262,#9058,.T.);
#17950=EDGE_CURVE('',#14255,#14292,#393,.F.);
#17951=EDGE_CURVE('',#14292,#14260,#9059,.T.);
#17952=EDGE_CURVE('',#14213,#14293,#9060,.T.);
#17953=EDGE_CURVE('',#14293,#14291,#9061,.T.);
#17954=EDGE_CURVE('',#14286,#14294,#9062,.T.);
#17955=EDGE_CURVE('',#14210,#14294,#9063,.T.);
#17956=EDGE_CURVE('',#14295,#14285,#9064,.T.);
#17957=EDGE_CURVE('',#14296,#14295,#9065,.T.);
#17958=EDGE_CURVE('',#14294,#14296,#9066,.T.);
#17959=EDGE_CURVE('',#14259,#14295,#9067,.T.);
#17960=EDGE_CURVE('',#14292,#14297,#9068,.T.);
#17961=EDGE_CURVE('',#14297,#14298,#9069,.T.);
#17962=EDGE_CURVE('',#14258,#14298,#9070,.T.);
#17963=EDGE_CURVE('',#14299,#14299,#2728,.T.);
#17964=EDGE_CURVE('',#14300,#14300,#2729,.T.);
#17965=EDGE_CURVE('',#14301,#14302,#9071,.T.);
#17966=EDGE_CURVE('',#14302,#14303,#9072,.T.);
#17967=EDGE_CURVE('',#14303,#14304,#9073,.T.);
#17968=EDGE_CURVE('',#14304,#14301,#9074,.T.);
#17969=EDGE_CURVE('',#14305,#14305,#2730,.T.);
#17970=EDGE_CURVE('',#14306,#14306,#2731,.T.);
#17971=EDGE_CURVE('',#14307,#14307,#2732,.T.);
#17972=EDGE_CURVE('',#14307,#14299,#9075,.T.);
#17973=EDGE_CURVE('',#14307,#14308,#9076,.T.);
#17974=EDGE_CURVE('',#14309,#14308,#2733,.T.);
#17975=EDGE_CURVE('',#14308,#14309,#2734,.T.);
#17976=EDGE_CURVE('',#14310,#14310,#2735,.T.);
#17977=EDGE_CURVE('',#14310,#14306,#9077,.T.);
#17978=EDGE_CURVE('',#14310,#14311,#9078,.T.);
#17979=EDGE_CURVE('',#14312,#14311,#2736,.T.);
#17980=EDGE_CURVE('',#14311,#14312,#2737,.T.);
#17981=EDGE_CURVE('',#14313,#14313,#2738,.T.);
#17982=EDGE_CURVE('',#14313,#14300,#9079,.T.);
#17983=EDGE_CURVE('',#14313,#14314,#9080,.T.);
#17984=EDGE_CURVE('',#14315,#14314,#2739,.T.);
#17985=EDGE_CURVE('',#14314,#14315,#2740,.T.);
#17986=EDGE_CURVE('',#14316,#14316,#2741,.T.);
#17987=EDGE_CURVE('',#14316,#14305,#9081,.T.);
#17988=EDGE_CURVE('',#14316,#14317,#9082,.T.);
#17989=EDGE_CURVE('',#14318,#14317,#2742,.T.);
#17990=EDGE_CURVE('',#14317,#14318,#2743,.T.);
#17991=EDGE_CURVE('',#14309,#14231,#9083,.T.);
#17992=EDGE_CURVE('',#14312,#14224,#9084,.T.);
#17993=EDGE_CURVE('',#14315,#14230,#9085,.T.);
#17994=EDGE_CURVE('',#14318,#14225,#9086,.T.);
#17995=EDGE_CURVE('',#14214,#14296,#9087,.T.);
#17996=EDGE_CURVE('',#14319,#14297,#9088,.T.);
#17997=EDGE_CURVE('',#14320,#14319,#9089,.T.);
#17998=EDGE_CURVE('',#14298,#14320,#9090,.T.);
#17999=EDGE_CURVE('',#14217,#14320,#9091,.T.);
#18000=EDGE_CURVE('',#14247,#14319,#9092,.T.);
#18001=EDGE_CURVE('',#14321,#14293,#9093,.T.);
#18002=EDGE_CURVE('',#14223,#14321,#9094,.T.);
#18003=EDGE_CURVE('',#14234,#14321,#9095,.T.);
#18004=EDGE_CURVE('',#14253,#14235,#9096,.T.);
#18005=EDGE_CURVE('',#14228,#14304,#9097,.T.);
#18006=EDGE_CURVE('',#14303,#14229,#9098,.T.);
#18007=EDGE_CURVE('',#14226,#14302,#9099,.T.);
#18008=EDGE_CURVE('',#14227,#14301,#9100,.T.);
#18009=EDGE_CURVE('',#14322,#14323,#9101,.T.);
#18010=EDGE_CURVE('',#14324,#14323,#9102,.T.);
#18011=EDGE_CURVE('',#14325,#14324,#9103,.T.);
#18012=EDGE_CURVE('',#14325,#14322,#9104,.T.);
#18013=EDGE_CURVE('',#14323,#14326,#2744,.T.);
#18014=EDGE_CURVE('',#14327,#14326,#9105,.T.);
#18015=EDGE_CURVE('',#14324,#14327,#2745,.T.);
#18016=EDGE_CURVE('',#14326,#14328,#9106,.T.);
#18017=EDGE_CURVE('',#14329,#14328,#9107,.T.);
#18018=EDGE_CURVE('',#14327,#14329,#9108,.T.);
#18019=EDGE_CURVE('',#14328,#14330,#2746,.T.);
#18020=EDGE_CURVE('',#14331,#14330,#9109,.T.);
#18021=EDGE_CURVE('',#14329,#14331,#2747,.T.);
#18022=EDGE_CURVE('',#14332,#14333,#9110,.T.);
#18023=EDGE_CURVE('',#14334,#14333,#9111,.T.);
#18024=EDGE_CURVE('',#14335,#14334,#9112,.T.);
#18025=EDGE_CURVE('',#14335,#14332,#9113,.T.);
#18026=EDGE_CURVE('',#14333,#14336,#2748,.T.);
#18027=EDGE_CURVE('',#14337,#14336,#9114,.T.);
#18028=EDGE_CURVE('',#14334,#14337,#2749,.T.);
#18029=EDGE_CURVE('',#14336,#14338,#9115,.T.);
#18030=EDGE_CURVE('',#14339,#14338,#9116,.T.);
#18031=EDGE_CURVE('',#14337,#14339,#9117,.T.);
#18032=EDGE_CURVE('',#14338,#14340,#2750,.T.);
#18033=EDGE_CURVE('',#14341,#14340,#9118,.T.);
#18034=EDGE_CURVE('',#14339,#14341,#2751,.T.);
#18035=EDGE_CURVE('',#14330,#14342,#9119,.T.);
#18036=EDGE_CURVE('',#14343,#14342,#9120,.T.);
#18037=EDGE_CURVE('',#14331,#14343,#9121,.T.);
#18038=EDGE_CURVE('',#14344,#14322,#2752,.T.);
#18039=EDGE_CURVE('',#14345,#14325,#2753,.T.);
#18040=EDGE_CURVE('',#14345,#14344,#9122,.T.);
#18041=EDGE_CURVE('',#14346,#14344,#9123,.T.);
#18042=EDGE_CURVE('',#14347,#14345,#9124,.T.);
#18043=EDGE_CURVE('',#14347,#14346,#9125,.T.);
#18044=EDGE_CURVE('',#14342,#14346,#2754,.T.);
#18045=EDGE_CURVE('',#14343,#14347,#2755,.T.);
#18046=EDGE_CURVE('',#14340,#14348,#9126,.T.);
#18047=EDGE_CURVE('',#14349,#14348,#9127,.T.);
#18048=EDGE_CURVE('',#14341,#14349,#9128,.T.);
#18049=EDGE_CURVE('',#14348,#14350,#2756,.T.);
#18050=EDGE_CURVE('',#14351,#14350,#9129,.T.);
#18051=EDGE_CURVE('',#14349,#14351,#2757,.T.);
#18052=EDGE_CURVE('',#14350,#14352,#9130,.T.);
#18053=EDGE_CURVE('',#14353,#14352,#9131,.T.);
#18054=EDGE_CURVE('',#14351,#14353,#9132,.T.);
#18055=EDGE_CURVE('',#14352,#14332,#2758,.T.);
#18056=EDGE_CURVE('',#14353,#14335,#2759,.T.);
#18057=EDGE_CURVE('',#14354,#14355,#9133,.T.);
#18058=EDGE_CURVE('',#14356,#14355,#9134,.T.);
#18059=EDGE_CURVE('',#14357,#14356,#9135,.T.);
#18060=EDGE_CURVE('',#14357,#14354,#9136,.T.);
#18061=EDGE_CURVE('',#14355,#14358,#2760,.T.);
#18062=EDGE_CURVE('',#14359,#14358,#9137,.T.);
#18063=EDGE_CURVE('',#14356,#14359,#2761,.T.);
#18064=EDGE_CURVE('',#14358,#14360,#9138,.T.);
#18065=EDGE_CURVE('',#14361,#14360,#9139,.T.);
#18066=EDGE_CURVE('',#14359,#14361,#9140,.T.);
#18067=EDGE_CURVE('',#14360,#14362,#2762,.T.);
#18068=EDGE_CURVE('',#14363,#14362,#9141,.T.);
#18069=EDGE_CURVE('',#14361,#14363,#2763,.T.);
#18070=EDGE_CURVE('',#14364,#14365,#9142,.T.);
#18071=EDGE_CURVE('',#14366,#14365,#9143,.T.);
#18072=EDGE_CURVE('',#14367,#14366,#9144,.T.);
#18073=EDGE_CURVE('',#14367,#14364,#9145,.T.);
#18074=EDGE_CURVE('',#14365,#14368,#2764,.T.);
#18075=EDGE_CURVE('',#14369,#14368,#9146,.T.);
#18076=EDGE_CURVE('',#14366,#14369,#2765,.T.);
#18077=EDGE_CURVE('',#14368,#14370,#9147,.T.);
#18078=EDGE_CURVE('',#14371,#14370,#9148,.T.);
#18079=EDGE_CURVE('',#14369,#14371,#9149,.T.);
#18080=EDGE_CURVE('',#14370,#14372,#2766,.T.);
#18081=EDGE_CURVE('',#14373,#14372,#9150,.T.);
#18082=EDGE_CURVE('',#14371,#14373,#2767,.T.);
#18083=EDGE_CURVE('',#14362,#14374,#9151,.T.);
#18084=EDGE_CURVE('',#14375,#14374,#9152,.T.);
#18085=EDGE_CURVE('',#14363,#14375,#9153,.T.);
#18086=EDGE_CURVE('',#14376,#14354,#2768,.T.);
#18087=EDGE_CURVE('',#14377,#14357,#2769,.T.);
#18088=EDGE_CURVE('',#14377,#14376,#9154,.T.);
#18089=EDGE_CURVE('',#14378,#14376,#9155,.T.);
#18090=EDGE_CURVE('',#14379,#14377,#9156,.T.);
#18091=EDGE_CURVE('',#14379,#14378,#9157,.T.);
#18092=EDGE_CURVE('',#14374,#14378,#2770,.T.);
#18093=EDGE_CURVE('',#14375,#14379,#2771,.T.);
#18094=EDGE_CURVE('',#14372,#14380,#9158,.T.);
#18095=EDGE_CURVE('',#14381,#14380,#9159,.T.);
#18096=EDGE_CURVE('',#14373,#14381,#9160,.T.);
#18097=EDGE_CURVE('',#14380,#14382,#2772,.T.);
#18098=EDGE_CURVE('',#14383,#14382,#9161,.T.);
#18099=EDGE_CURVE('',#14381,#14383,#2773,.T.);
#18100=EDGE_CURVE('',#14382,#14384,#9162,.T.);
#18101=EDGE_CURVE('',#14385,#14384,#9163,.T.);
#18102=EDGE_CURVE('',#14383,#14385,#9164,.T.);
#18103=EDGE_CURVE('',#14384,#14364,#2774,.T.);
#18104=EDGE_CURVE('',#14385,#14367,#2775,.T.);
#18105=EDGE_CURVE('',#14386,#14387,#9165,.T.);
#18106=EDGE_CURVE('',#14388,#14387,#9166,.T.);
#18107=EDGE_CURVE('',#14389,#14388,#9167,.T.);
#18108=EDGE_CURVE('',#14389,#14386,#9168,.T.);
#18109=EDGE_CURVE('',#14387,#14390,#2776,.T.);
#18110=EDGE_CURVE('',#14391,#14390,#9169,.T.);
#18111=EDGE_CURVE('',#14388,#14391,#2777,.T.);
#18112=EDGE_CURVE('',#14390,#14392,#9170,.T.);
#18113=EDGE_CURVE('',#14393,#14392,#9171,.T.);
#18114=EDGE_CURVE('',#14391,#14393,#9172,.T.);
#18115=EDGE_CURVE('',#14392,#14394,#2778,.T.);
#18116=EDGE_CURVE('',#14395,#14394,#9173,.T.);
#18117=EDGE_CURVE('',#14393,#14395,#2779,.T.);
#18118=EDGE_CURVE('',#14396,#14397,#9174,.T.);
#18119=EDGE_CURVE('',#14398,#14397,#9175,.T.);
#18120=EDGE_CURVE('',#14399,#14398,#9176,.T.);
#18121=EDGE_CURVE('',#14399,#14396,#9177,.T.);
#18122=EDGE_CURVE('',#14397,#14400,#2780,.T.);
#18123=EDGE_CURVE('',#14401,#14400,#9178,.T.);
#18124=EDGE_CURVE('',#14398,#14401,#2781,.T.);
#18125=EDGE_CURVE('',#14400,#14402,#9179,.T.);
#18126=EDGE_CURVE('',#14403,#14402,#9180,.T.);
#18127=EDGE_CURVE('',#14401,#14403,#9181,.T.);
#18128=EDGE_CURVE('',#14402,#14404,#2782,.T.);
#18129=EDGE_CURVE('',#14405,#14404,#9182,.T.);
#18130=EDGE_CURVE('',#14403,#14405,#2783,.T.);
#18131=EDGE_CURVE('',#14394,#14406,#9183,.T.);
#18132=EDGE_CURVE('',#14407,#14406,#9184,.T.);
#18133=EDGE_CURVE('',#14395,#14407,#9185,.T.);
#18134=EDGE_CURVE('',#14408,#14386,#2784,.T.);
#18135=EDGE_CURVE('',#14409,#14389,#2785,.T.);
#18136=EDGE_CURVE('',#14409,#14408,#9186,.T.);
#18137=EDGE_CURVE('',#14410,#14408,#9187,.T.);
#18138=EDGE_CURVE('',#14411,#14409,#9188,.T.);
#18139=EDGE_CURVE('',#14411,#14410,#9189,.T.);
#18140=EDGE_CURVE('',#14406,#14410,#2786,.T.);
#18141=EDGE_CURVE('',#14407,#14411,#2787,.T.);
#18142=EDGE_CURVE('',#14404,#14412,#9190,.T.);
#18143=EDGE_CURVE('',#14413,#14412,#9191,.T.);
#18144=EDGE_CURVE('',#14405,#14413,#9192,.T.);
#18145=EDGE_CURVE('',#14412,#14414,#2788,.T.);
#18146=EDGE_CURVE('',#14415,#14414,#9193,.T.);
#18147=EDGE_CURVE('',#14413,#14415,#2789,.T.);
#18148=EDGE_CURVE('',#14414,#14416,#9194,.T.);
#18149=EDGE_CURVE('',#14417,#14416,#9195,.T.);
#18150=EDGE_CURVE('',#14415,#14417,#9196,.T.);
#18151=EDGE_CURVE('',#14416,#14396,#2790,.T.);
#18152=EDGE_CURVE('',#14417,#14399,#2791,.T.);
#18153=EDGE_CURVE('',#14418,#14419,#9197,.T.);
#18154=EDGE_CURVE('',#14420,#14419,#9198,.T.);
#18155=EDGE_CURVE('',#14421,#14420,#9199,.T.);
#18156=EDGE_CURVE('',#14421,#14418,#9200,.T.);
#18157=EDGE_CURVE('',#14419,#14422,#2792,.T.);
#18158=EDGE_CURVE('',#14423,#14422,#9201,.T.);
#18159=EDGE_CURVE('',#14420,#14423,#2793,.T.);
#18160=EDGE_CURVE('',#14422,#14424,#9202,.T.);
#18161=EDGE_CURVE('',#14425,#14424,#9203,.T.);
#18162=EDGE_CURVE('',#14423,#14425,#9204,.T.);
#18163=EDGE_CURVE('',#14424,#14426,#2794,.T.);
#18164=EDGE_CURVE('',#14427,#14426,#9205,.T.);
#18165=EDGE_CURVE('',#14425,#14427,#2795,.T.);
#18166=EDGE_CURVE('',#14428,#14429,#9206,.T.);
#18167=EDGE_CURVE('',#14430,#14429,#9207,.T.);
#18168=EDGE_CURVE('',#14431,#14430,#9208,.T.);
#18169=EDGE_CURVE('',#14431,#14428,#9209,.T.);
#18170=EDGE_CURVE('',#14429,#14432,#2796,.T.);
#18171=EDGE_CURVE('',#14433,#14432,#9210,.T.);
#18172=EDGE_CURVE('',#14430,#14433,#2797,.T.);
#18173=EDGE_CURVE('',#14432,#14434,#9211,.T.);
#18174=EDGE_CURVE('',#14435,#14434,#9212,.T.);
#18175=EDGE_CURVE('',#14433,#14435,#9213,.T.);
#18176=EDGE_CURVE('',#14434,#14436,#2798,.T.);
#18177=EDGE_CURVE('',#14437,#14436,#9214,.T.);
#18178=EDGE_CURVE('',#14435,#14437,#2799,.T.);
#18179=EDGE_CURVE('',#14426,#14438,#9215,.T.);
#18180=EDGE_CURVE('',#14439,#14438,#9216,.T.);
#18181=EDGE_CURVE('',#14427,#14439,#9217,.T.);
#18182=EDGE_CURVE('',#14440,#14418,#2800,.T.);
#18183=EDGE_CURVE('',#14441,#14421,#2801,.T.);
#18184=EDGE_CURVE('',#14441,#14440,#9218,.T.);
#18185=EDGE_CURVE('',#14442,#14440,#9219,.T.);
#18186=EDGE_CURVE('',#14443,#14441,#9220,.T.);
#18187=EDGE_CURVE('',#14443,#14442,#9221,.T.);
#18188=EDGE_CURVE('',#14438,#14442,#2802,.T.);
#18189=EDGE_CURVE('',#14439,#14443,#2803,.T.);
#18190=EDGE_CURVE('',#14436,#14444,#9222,.T.);
#18191=EDGE_CURVE('',#14445,#14444,#9223,.T.);
#18192=EDGE_CURVE('',#14437,#14445,#9224,.T.);
#18193=EDGE_CURVE('',#14444,#14446,#2804,.T.);
#18194=EDGE_CURVE('',#14447,#14446,#9225,.T.);
#18195=EDGE_CURVE('',#14445,#14447,#2805,.T.);
#18196=EDGE_CURVE('',#14446,#14448,#9226,.T.);
#18197=EDGE_CURVE('',#14449,#14448,#9227,.T.);
#18198=EDGE_CURVE('',#14447,#14449,#9228,.T.);
#18199=EDGE_CURVE('',#14448,#14428,#2806,.T.);
#18200=EDGE_CURVE('',#14449,#14431,#2807,.T.);
#18201=EDGE_CURVE('',#14450,#14451,#394,.T.);
#18202=EDGE_CURVE('',#14452,#14450,#9229,.T.);
#18203=EDGE_CURVE('',#14453,#14452,#395,.T.);
#18204=EDGE_CURVE('',#14453,#14454,#9230,.T.);
#18205=EDGE_CURVE('',#14455,#14454,#396,.T.);
#18206=EDGE_CURVE('',#14456,#14455,#9231,.T.);
#18207=EDGE_CURVE('',#14457,#14456,#397,.T.);
#18208=EDGE_CURVE('',#14451,#14457,#9232,.T.);
#18209=EDGE_CURVE('',#14458,#14459,#9233,.T.);
#18210=EDGE_CURVE('',#14460,#14458,#398,.T.);
#18211=EDGE_CURVE('',#14461,#14460,#9234,.T.);
#18212=EDGE_CURVE('',#14462,#14461,#399,.T.);
#18213=EDGE_CURVE('',#14463,#14462,#9235,.T.);
#18214=EDGE_CURVE('',#14464,#14463,#400,.T.);
#18215=EDGE_CURVE('',#14465,#14464,#9236,.T.);
#18216=EDGE_CURVE('',#14459,#14465,#401,.T.);
#18217=EDGE_CURVE('',#14462,#14466,#9237,.T.);
#18218=EDGE_CURVE('',#14466,#14467,#9238,.T.);
#18219=EDGE_CURVE('',#14463,#14467,#9239,.T.);
#18220=EDGE_CURVE('',#14461,#14468,#9240,.T.);
#18221=EDGE_CURVE('',#14468,#14466,#402,.T.);
#18222=EDGE_CURVE('',#14460,#14469,#9241,.T.);
#18223=EDGE_CURVE('',#14469,#14468,#9242,.T.);
#18224=EDGE_CURVE('',#14458,#14470,#9243,.T.);
#18225=EDGE_CURVE('',#14470,#14469,#403,.T.);
#18226=EDGE_CURVE('',#14454,#14471,#9244,.T.);
#18227=EDGE_CURVE('',#14471,#14472,#404,.T.);
#18228=EDGE_CURVE('',#14455,#14472,#9245,.T.);
#18229=EDGE_CURVE('',#14452,#14473,#9246,.T.);
#18230=EDGE_CURVE('',#14473,#14474,#405,.T.);
#18231=EDGE_CURVE('',#14453,#14474,#9247,.T.);
#18232=EDGE_CURVE('',#14450,#14475,#9248,.T.);
#18233=EDGE_CURVE('',#14475,#14473,#9249,.T.);
#18234=EDGE_CURVE('',#14474,#14471,#9250,.T.);
#18235=EDGE_CURVE('',#14476,#14475,#406,.T.);
#18236=EDGE_CURVE('',#14477,#14476,#9251,.T.);
#18237=EDGE_CURVE('',#14478,#14477,#407,.T.);
#18238=EDGE_CURVE('',#14472,#14478,#9252,.T.);
#18239=EDGE_CURVE('',#14479,#14470,#9253,.T.);
#18240=EDGE_CURVE('',#14480,#14479,#408,.T.);
#18241=EDGE_CURVE('',#14481,#14480,#9254,.T.);
#18242=EDGE_CURVE('',#14467,#14481,#409,.T.);
#18243=EDGE_CURVE('',#14459,#14479,#9255,.T.);
#18244=EDGE_CURVE('',#14451,#14476,#9256,.T.);
#18245=EDGE_CURVE('',#14464,#14481,#9257,.T.);
#18246=EDGE_CURVE('',#14465,#14480,#9258,.T.);
#18247=EDGE_CURVE('',#14456,#14478,#9259,.T.);
#18248=EDGE_CURVE('',#14457,#14477,#9260,.T.);
#18249=EDGE_CURVE('',#14482,#14483,#410,.T.);
#18250=EDGE_CURVE('',#14484,#14482,#9261,.T.);
#18251=EDGE_CURVE('',#14485,#14484,#411,.T.);
#18252=EDGE_CURVE('',#14486,#14485,#9262,.T.);
#18253=EDGE_CURVE('',#14487,#14486,#412,.T.);
#18254=EDGE_CURVE('',#14488,#14487,#9263,.T.);
#18255=EDGE_CURVE('',#14489,#14488,#413,.T.);
#18256=EDGE_CURVE('',#14489,#14483,#9264,.T.);
#18257=EDGE_CURVE('',#14490,#14491,#9265,.T.);
#18258=EDGE_CURVE('',#14492,#14490,#414,.T.);
#18259=EDGE_CURVE('',#14493,#14492,#9266,.T.);
#18260=EDGE_CURVE('',#14494,#14493,#415,.T.);
#18261=EDGE_CURVE('',#14495,#14494,#9267,.T.);
#18262=EDGE_CURVE('',#14496,#14495,#416,.T.);
#18263=EDGE_CURVE('',#14497,#14496,#9268,.T.);
#18264=EDGE_CURVE('',#14491,#14497,#417,.T.);
#18265=EDGE_CURVE('',#14494,#14498,#9269,.T.);
#18266=EDGE_CURVE('',#14498,#14499,#9270,.T.);
#18267=EDGE_CURVE('',#14495,#14499,#9271,.T.);
#18268=EDGE_CURVE('',#14493,#14500,#9272,.T.);
#18269=EDGE_CURVE('',#14500,#14498,#418,.T.);
#18270=EDGE_CURVE('',#14492,#14501,#9273,.T.);
#18271=EDGE_CURVE('',#14501,#14500,#9274,.T.);
#18272=EDGE_CURVE('',#14490,#14502,#9275,.T.);
#18273=EDGE_CURVE('',#14502,#14501,#419,.T.);
#18274=EDGE_CURVE('',#14486,#14503,#9276,.T.);
#18275=EDGE_CURVE('',#14503,#14504,#420,.T.);
#18276=EDGE_CURVE('',#14487,#14504,#9277,.T.);
#18277=EDGE_CURVE('',#14485,#14505,#9278,.T.);
#18278=EDGE_CURVE('',#14505,#14503,#9279,.T.);
#18279=EDGE_CURVE('',#14484,#14506,#9280,.T.);
#18280=EDGE_CURVE('',#14506,#14505,#421,.T.);
#18281=EDGE_CURVE('',#14482,#14507,#9281,.T.);
#18282=EDGE_CURVE('',#14507,#14506,#9282,.T.);
#18283=EDGE_CURVE('',#14508,#14507,#422,.T.);
#18284=EDGE_CURVE('',#14509,#14508,#9283,.T.);
#18285=EDGE_CURVE('',#14510,#14509,#423,.T.);
#18286=EDGE_CURVE('',#14504,#14510,#9284,.T.);
#18287=EDGE_CURVE('',#14511,#14502,#9285,.T.);
#18288=EDGE_CURVE('',#14512,#14511,#424,.T.);
#18289=EDGE_CURVE('',#14513,#14512,#9286,.T.);
#18290=EDGE_CURVE('',#14499,#14513,#425,.T.);
#18291=EDGE_CURVE('',#14491,#14511,#9287,.T.);
#18292=EDGE_CURVE('',#14483,#14508,#9288,.T.);
#18293=EDGE_CURVE('',#14496,#14513,#9289,.T.);
#18294=EDGE_CURVE('',#14497,#14512,#9290,.T.);
#18295=EDGE_CURVE('',#14488,#14510,#9291,.T.);
#18296=EDGE_CURVE('',#14489,#14509,#9292,.T.);
#18297=EDGE_CURVE('',#14514,#14515,#9293,.T.);
#18298=EDGE_CURVE('',#14516,#14514,#426,.T.);
#18299=EDGE_CURVE('',#14517,#14516,#9294,.T.);
#18300=EDGE_CURVE('',#14518,#14517,#427,.T.);
#18301=EDGE_CURVE('',#14519,#14518,#9295,.T.);
#18302=EDGE_CURVE('',#14520,#14519,#428,.T.);
#18303=EDGE_CURVE('',#14521,#14520,#9296,.T.);
#18304=EDGE_CURVE('',#14515,#14521,#429,.T.);
#18305=EDGE_CURVE('',#14522,#14523,#9297,.T.);
#18306=EDGE_CURVE('',#14524,#14522,#430,.T.);
#18307=EDGE_CURVE('',#14525,#14524,#9298,.T.);
#18308=EDGE_CURVE('',#14526,#14525,#431,.T.);
#18309=EDGE_CURVE('',#14527,#14526,#9299,.T.);
#18310=EDGE_CURVE('',#14528,#14527,#432,.T.);
#18311=EDGE_CURVE('',#14529,#14528,#9300,.T.);
#18312=EDGE_CURVE('',#14523,#14529,#433,.T.);
#18313=EDGE_CURVE('',#14526,#14530,#9301,.T.);
#18314=EDGE_CURVE('',#14530,#14531,#9302,.T.);
#18315=EDGE_CURVE('',#14527,#14531,#9303,.T.);
#18316=EDGE_CURVE('',#14525,#14532,#9304,.T.);
#18317=EDGE_CURVE('',#14532,#14530,#434,.T.);
#18318=EDGE_CURVE('',#14524,#14533,#9305,.T.);
#18319=EDGE_CURVE('',#14533,#14532,#9306,.T.);
#18320=EDGE_CURVE('',#14522,#14534,#9307,.T.);
#18321=EDGE_CURVE('',#14534,#14533,#435,.T.);
#18322=EDGE_CURVE('',#14518,#14535,#9308,.T.);
#18323=EDGE_CURVE('',#14535,#14536,#9309,.T.);
#18324=EDGE_CURVE('',#14519,#14536,#9310,.T.);
#18325=EDGE_CURVE('',#14517,#14537,#9311,.T.);
#18326=EDGE_CURVE('',#14537,#14535,#436,.T.);
#18327=EDGE_CURVE('',#14538,#14516,#9312,.T.);
#18328=EDGE_CURVE('',#14538,#14537,#9313,.T.);
#18329=EDGE_CURVE('',#14514,#14539,#9314,.T.);
#18330=EDGE_CURVE('',#14539,#14538,#437,.T.);
#18331=EDGE_CURVE('',#14540,#14539,#9315,.T.);
#18332=EDGE_CURVE('',#14541,#14540,#438,.T.);
#18333=EDGE_CURVE('',#14541,#14542,#9316,.T.);
#18334=EDGE_CURVE('',#14536,#14542,#439,.T.);
#18335=EDGE_CURVE('',#14543,#14534,#9317,.T.);
#18336=EDGE_CURVE('',#14544,#14543,#440,.T.);
#18337=EDGE_CURVE('',#14545,#14544,#9318,.T.);
#18338=EDGE_CURVE('',#14531,#14545,#441,.T.);
#18339=EDGE_CURVE('',#14523,#14543,#9319,.T.);
#18340=EDGE_CURVE('',#14515,#14540,#9320,.T.);
#18341=EDGE_CURVE('',#14528,#14545,#9321,.T.);
#18342=EDGE_CURVE('',#14544,#14529,#9322,.T.);
#18343=EDGE_CURVE('',#14521,#14541,#9323,.T.);
#18344=EDGE_CURVE('',#14520,#14542,#9324,.T.);
#18345=EDGE_CURVE('',#14546,#14547,#9325,.T.);
#18346=EDGE_CURVE('',#14548,#14546,#442,.T.);
#18347=EDGE_CURVE('',#14549,#14548,#9326,.T.);
#18348=EDGE_CURVE('',#14550,#14549,#443,.T.);
#18349=EDGE_CURVE('',#14551,#14550,#9327,.T.);
#18350=EDGE_CURVE('',#14552,#14551,#444,.T.);
#18351=EDGE_CURVE('',#14552,#14553,#9328,.T.);
#18352=EDGE_CURVE('',#14547,#14553,#445,.T.);
#18353=EDGE_CURVE('',#14554,#14555,#9329,.T.);
#18354=EDGE_CURVE('',#14556,#14554,#446,.T.);
#18355=EDGE_CURVE('',#14557,#14556,#9330,.T.);
#18356=EDGE_CURVE('',#14558,#14557,#447,.T.);
#18357=EDGE_CURVE('',#14559,#14558,#9331,.T.);
#18358=EDGE_CURVE('',#14560,#14559,#448,.T.);
#18359=EDGE_CURVE('',#14561,#14560,#9332,.T.);
#18360=EDGE_CURVE('',#14555,#14561,#449,.T.);
#18361=EDGE_CURVE('',#14558,#14562,#9333,.T.);
#18362=EDGE_CURVE('',#14562,#14563,#9334,.T.);
#18363=EDGE_CURVE('',#14559,#14563,#9335,.T.);
#18364=EDGE_CURVE('',#14557,#14564,#9336,.T.);
#18365=EDGE_CURVE('',#14564,#14562,#450,.T.);
#18366=EDGE_CURVE('',#14556,#14565,#9337,.T.);
#18367=EDGE_CURVE('',#14565,#14564,#9338,.T.);
#18368=EDGE_CURVE('',#14554,#14566,#9339,.T.);
#18369=EDGE_CURVE('',#14566,#14565,#451,.T.);
#18370=EDGE_CURVE('',#14550,#14567,#9340,.T.);
#18371=EDGE_CURVE('',#14567,#14568,#9341,.T.);
#18372=EDGE_CURVE('',#14551,#14568,#9342,.T.);
#18373=EDGE_CURVE('',#14549,#14569,#9343,.T.);
#18374=EDGE_CURVE('',#14569,#14567,#452,.T.);
#18375=EDGE_CURVE('',#14548,#14570,#9344,.T.);
#18376=EDGE_CURVE('',#14570,#14569,#9345,.T.);
#18377=EDGE_CURVE('',#14546,#14571,#9346,.T.);
#18378=EDGE_CURVE('',#14571,#14570,#453,.T.);
#18379=EDGE_CURVE('',#14572,#14571,#9347,.T.);
#18380=EDGE_CURVE('',#14573,#14572,#454,.T.);
#18381=EDGE_CURVE('',#14574,#14573,#9348,.T.);
#18382=EDGE_CURVE('',#14568,#14574,#455,.T.);
#18383=EDGE_CURVE('',#14575,#14566,#9349,.T.);
#18384=EDGE_CURVE('',#14576,#14575,#456,.T.);
#18385=EDGE_CURVE('',#14577,#14576,#9350,.T.);
#18386=EDGE_CURVE('',#14563,#14577,#457,.T.);
#18387=EDGE_CURVE('',#14555,#14575,#9351,.T.);
#18388=EDGE_CURVE('',#14547,#14572,#9352,.T.);
#18389=EDGE_CURVE('',#14560,#14577,#9353,.T.);
#18390=EDGE_CURVE('',#14561,#14576,#9354,.T.);
#18391=EDGE_CURVE('',#14552,#14574,#9355,.T.);
#18392=EDGE_CURVE('',#14553,#14573,#9356,.T.);
#18393=EDGE_CURVE('',#14578,#14579,#9357,.T.);
#18394=EDGE_CURVE('',#14580,#14579,#9358,.T.);
#18395=EDGE_CURVE('',#14581,#14580,#9359,.T.);
#18396=EDGE_CURVE('',#14581,#14578,#9360,.T.);
#18397=EDGE_CURVE('',#14579,#14582,#2808,.T.);
#18398=EDGE_CURVE('',#14583,#14582,#9361,.T.);
#18399=EDGE_CURVE('',#14580,#14583,#2809,.T.);
#18400=EDGE_CURVE('',#14582,#14584,#9362,.T.);
#18401=EDGE_CURVE('',#14585,#14584,#9363,.T.);
#18402=EDGE_CURVE('',#14583,#14585,#9364,.T.);
#18403=EDGE_CURVE('',#14584,#14586,#2810,.T.);
#18404=EDGE_CURVE('',#14587,#14586,#9365,.T.);
#18405=EDGE_CURVE('',#14585,#14587,#2811,.T.);
#18406=EDGE_CURVE('',#14588,#14589,#9366,.T.);
#18407=EDGE_CURVE('',#14590,#14589,#9367,.T.);
#18408=EDGE_CURVE('',#14591,#14590,#9368,.T.);
#18409=EDGE_CURVE('',#14591,#14588,#9369,.T.);
#18410=EDGE_CURVE('',#14589,#14592,#2812,.T.);
#18411=EDGE_CURVE('',#14593,#14592,#9370,.T.);
#18412=EDGE_CURVE('',#14590,#14593,#2813,.T.);
#18413=EDGE_CURVE('',#14592,#14594,#9371,.T.);
#18414=EDGE_CURVE('',#14595,#14594,#9372,.T.);
#18415=EDGE_CURVE('',#14593,#14595,#9373,.T.);
#18416=EDGE_CURVE('',#14594,#14596,#2814,.T.);
#18417=EDGE_CURVE('',#14597,#14596,#9374,.T.);
#18418=EDGE_CURVE('',#14595,#14597,#2815,.T.);
#18419=EDGE_CURVE('',#14586,#14598,#9375,.T.);
#18420=EDGE_CURVE('',#14599,#14598,#9376,.T.);
#18421=EDGE_CURVE('',#14587,#14599,#9377,.T.);
#18422=EDGE_CURVE('',#14600,#14578,#2816,.T.);
#18423=EDGE_CURVE('',#14601,#14581,#2817,.T.);
#18424=EDGE_CURVE('',#14601,#14600,#9378,.T.);
#18425=EDGE_CURVE('',#14602,#14600,#9379,.T.);
#18426=EDGE_CURVE('',#14603,#14601,#9380,.T.);
#18427=EDGE_CURVE('',#14603,#14602,#9381,.T.);
#18428=EDGE_CURVE('',#14598,#14602,#2818,.T.);
#18429=EDGE_CURVE('',#14599,#14603,#2819,.T.);
#18430=EDGE_CURVE('',#14596,#14604,#9382,.T.);
#18431=EDGE_CURVE('',#14605,#14604,#9383,.T.);
#18432=EDGE_CURVE('',#14597,#14605,#9384,.T.);
#18433=EDGE_CURVE('',#14604,#14606,#2820,.T.);
#18434=EDGE_CURVE('',#14607,#14606,#9385,.T.);
#18435=EDGE_CURVE('',#14605,#14607,#2821,.T.);
#18436=EDGE_CURVE('',#14606,#14608,#9386,.T.);
#18437=EDGE_CURVE('',#14609,#14608,#9387,.T.);
#18438=EDGE_CURVE('',#14607,#14609,#9388,.T.);
#18439=EDGE_CURVE('',#14608,#14588,#2822,.T.);
#18440=EDGE_CURVE('',#14609,#14591,#2823,.T.);
#18441=EDGE_CURVE('',#14610,#14611,#9389,.T.);
#18442=EDGE_CURVE('',#14612,#14611,#9390,.T.);
#18443=EDGE_CURVE('',#14613,#14612,#9391,.T.);
#18444=EDGE_CURVE('',#14613,#14610,#9392,.T.);
#18445=EDGE_CURVE('',#14611,#14614,#2824,.T.);
#18446=EDGE_CURVE('',#14615,#14614,#9393,.T.);
#18447=EDGE_CURVE('',#14612,#14615,#2825,.T.);
#18448=EDGE_CURVE('',#14614,#14616,#9394,.T.);
#18449=EDGE_CURVE('',#14617,#14616,#9395,.T.);
#18450=EDGE_CURVE('',#14615,#14617,#9396,.T.);
#18451=EDGE_CURVE('',#14616,#14618,#2826,.T.);
#18452=EDGE_CURVE('',#14619,#14618,#9397,.T.);
#18453=EDGE_CURVE('',#14617,#14619,#2827,.T.);
#18454=EDGE_CURVE('',#14620,#14621,#9398,.T.);
#18455=EDGE_CURVE('',#14622,#14621,#9399,.T.);
#18456=EDGE_CURVE('',#14623,#14622,#9400,.T.);
#18457=EDGE_CURVE('',#14623,#14620,#9401,.T.);
#18458=EDGE_CURVE('',#14621,#14624,#2828,.T.);
#18459=EDGE_CURVE('',#14625,#14624,#9402,.T.);
#18460=EDGE_CURVE('',#14622,#14625,#2829,.T.);
#18461=EDGE_CURVE('',#14624,#14626,#9403,.T.);
#18462=EDGE_CURVE('',#14627,#14626,#9404,.T.);
#18463=EDGE_CURVE('',#14625,#14627,#9405,.T.);
#18464=EDGE_CURVE('',#14626,#14628,#2830,.T.);
#18465=EDGE_CURVE('',#14629,#14628,#9406,.T.);
#18466=EDGE_CURVE('',#14627,#14629,#2831,.T.);
#18467=EDGE_CURVE('',#14618,#14630,#9407,.T.);
#18468=EDGE_CURVE('',#14631,#14630,#9408,.T.);
#18469=EDGE_CURVE('',#14619,#14631,#9409,.T.);
#18470=EDGE_CURVE('',#14632,#14610,#2832,.T.);
#18471=EDGE_CURVE('',#14633,#14613,#2833,.T.);
#18472=EDGE_CURVE('',#14633,#14632,#9410,.T.);
#18473=EDGE_CURVE('',#14634,#14632,#9411,.T.);
#18474=EDGE_CURVE('',#14635,#14633,#9412,.T.);
#18475=EDGE_CURVE('',#14635,#14634,#9413,.T.);
#18476=EDGE_CURVE('',#14630,#14634,#2834,.T.);
#18477=EDGE_CURVE('',#14631,#14635,#2835,.T.);
#18478=EDGE_CURVE('',#14628,#14636,#9414,.T.);
#18479=EDGE_CURVE('',#14637,#14636,#9415,.T.);
#18480=EDGE_CURVE('',#14629,#14637,#9416,.T.);
#18481=EDGE_CURVE('',#14636,#14638,#2836,.T.);
#18482=EDGE_CURVE('',#14639,#14638,#9417,.T.);
#18483=EDGE_CURVE('',#14637,#14639,#2837,.T.);
#18484=EDGE_CURVE('',#14638,#14640,#9418,.T.);
#18485=EDGE_CURVE('',#14641,#14640,#9419,.T.);
#18486=EDGE_CURVE('',#14639,#14641,#9420,.T.);
#18487=EDGE_CURVE('',#14640,#14620,#2838,.T.);
#18488=EDGE_CURVE('',#14641,#14623,#2839,.T.);
#18489=EDGE_CURVE('',#14642,#14643,#9421,.T.);
#18490=EDGE_CURVE('',#14644,#14643,#9422,.T.);
#18491=EDGE_CURVE('',#14645,#14644,#9423,.T.);
#18492=EDGE_CURVE('',#14645,#14642,#9424,.T.);
#18493=EDGE_CURVE('',#14643,#14646,#2840,.T.);
#18494=EDGE_CURVE('',#14647,#14646,#9425,.T.);
#18495=EDGE_CURVE('',#14644,#14647,#2841,.T.);
#18496=EDGE_CURVE('',#14646,#14648,#9426,.T.);
#18497=EDGE_CURVE('',#14649,#14648,#9427,.T.);
#18498=EDGE_CURVE('',#14647,#14649,#9428,.T.);
#18499=EDGE_CURVE('',#14648,#14650,#2842,.T.);
#18500=EDGE_CURVE('',#14651,#14650,#9429,.T.);
#18501=EDGE_CURVE('',#14649,#14651,#2843,.T.);
#18502=EDGE_CURVE('',#14652,#14653,#9430,.T.);
#18503=EDGE_CURVE('',#14654,#14653,#9431,.T.);
#18504=EDGE_CURVE('',#14655,#14654,#9432,.T.);
#18505=EDGE_CURVE('',#14655,#14652,#9433,.T.);
#18506=EDGE_CURVE('',#14653,#14656,#2844,.T.);
#18507=EDGE_CURVE('',#14657,#14656,#9434,.T.);
#18508=EDGE_CURVE('',#14654,#14657,#2845,.T.);
#18509=EDGE_CURVE('',#14656,#14658,#9435,.T.);
#18510=EDGE_CURVE('',#14659,#14658,#9436,.T.);
#18511=EDGE_CURVE('',#14657,#14659,#9437,.T.);
#18512=EDGE_CURVE('',#14658,#14660,#2846,.T.);
#18513=EDGE_CURVE('',#14661,#14660,#9438,.T.);
#18514=EDGE_CURVE('',#14659,#14661,#2847,.T.);
#18515=EDGE_CURVE('',#14650,#14662,#9439,.T.);
#18516=EDGE_CURVE('',#14663,#14662,#9440,.T.);
#18517=EDGE_CURVE('',#14651,#14663,#9441,.T.);
#18518=EDGE_CURVE('',#14664,#14642,#2848,.T.);
#18519=EDGE_CURVE('',#14665,#14645,#2849,.T.);
#18520=EDGE_CURVE('',#14665,#14664,#9442,.T.);
#18521=EDGE_CURVE('',#14666,#14664,#9443,.T.);
#18522=EDGE_CURVE('',#14667,#14665,#9444,.T.);
#18523=EDGE_CURVE('',#14667,#14666,#9445,.T.);
#18524=EDGE_CURVE('',#14662,#14666,#2850,.T.);
#18525=EDGE_CURVE('',#14663,#14667,#2851,.T.);
#18526=EDGE_CURVE('',#14660,#14668,#9446,.T.);
#18527=EDGE_CURVE('',#14669,#14668,#9447,.T.);
#18528=EDGE_CURVE('',#14661,#14669,#9448,.T.);
#18529=EDGE_CURVE('',#14668,#14670,#2852,.T.);
#18530=EDGE_CURVE('',#14671,#14670,#9449,.T.);
#18531=EDGE_CURVE('',#14669,#14671,#2853,.T.);
#18532=EDGE_CURVE('',#14670,#14672,#9450,.T.);
#18533=EDGE_CURVE('',#14673,#14672,#9451,.T.);
#18534=EDGE_CURVE('',#14671,#14673,#9452,.T.);
#18535=EDGE_CURVE('',#14672,#14652,#2854,.T.);
#18536=EDGE_CURVE('',#14673,#14655,#2855,.T.);
#18537=EDGE_CURVE('',#14674,#14675,#2856,.T.);
#18538=EDGE_CURVE('',#14674,#14676,#9453,.T.);
#18539=EDGE_CURVE('',#14677,#14676,#2857,.T.);
#18540=EDGE_CURVE('',#14675,#14677,#9454,.T.);
#18541=EDGE_CURVE('',#14678,#14674,#9455,.T.);
#18542=EDGE_CURVE('',#14678,#14679,#9456,.T.);
#18543=EDGE_CURVE('',#14676,#14679,#9457,.T.);
#18544=EDGE_CURVE('',#14680,#14678,#2858,.T.);
#18545=EDGE_CURVE('',#14680,#14681,#9458,.T.);
#18546=EDGE_CURVE('',#14679,#14681,#2859,.T.);
#18547=EDGE_CURVE('',#14682,#14680,#9459,.T.);
#18548=EDGE_CURVE('',#14682,#14683,#9460,.T.);
#18549=EDGE_CURVE('',#14681,#14683,#9461,.T.);
#18550=EDGE_CURVE('',#14684,#14682,#2860,.T.);
#18551=EDGE_CURVE('',#14684,#14685,#9462,.T.);
#18552=EDGE_CURVE('',#14683,#14685,#2861,.T.);
#18553=EDGE_CURVE('',#14686,#14684,#9463,.T.);
#18554=EDGE_CURVE('',#14686,#14687,#9464,.T.);
#18555=EDGE_CURVE('',#14685,#14687,#9465,.T.);
#18556=EDGE_CURVE('',#14688,#14686,#2862,.T.);
#18557=EDGE_CURVE('',#14688,#14689,#9466,.T.);
#18558=EDGE_CURVE('',#14687,#14689,#2863,.T.);
#18559=EDGE_CURVE('',#14675,#14688,#9467,.T.);
#18560=EDGE_CURVE('',#14689,#14677,#9468,.T.);
#18561=EDGE_CURVE('',#14690,#14691,#2864,.T.);
#18562=EDGE_CURVE('',#14690,#14692,#9469,.T.);
#18563=EDGE_CURVE('',#14693,#14692,#2865,.T.);
#18564=EDGE_CURVE('',#14691,#14693,#9470,.T.);
#18565=EDGE_CURVE('',#14691,#14694,#9471,.T.);
#18566=EDGE_CURVE('',#14695,#14693,#9472,.T.);
#18567=EDGE_CURVE('',#14694,#14695,#9473,.T.);
#18568=EDGE_CURVE('',#14694,#14696,#2866,.T.);
#18569=EDGE_CURVE('',#14697,#14695,#2867,.T.);
#18570=EDGE_CURVE('',#14696,#14697,#9474,.T.);
#18571=EDGE_CURVE('',#14696,#14698,#9475,.T.);
#18572=EDGE_CURVE('',#14699,#14697,#9476,.T.);
#18573=EDGE_CURVE('',#14698,#14699,#9477,.T.);
#18574=EDGE_CURVE('',#14698,#14700,#2868,.T.);
#18575=EDGE_CURVE('',#14701,#14699,#2869,.T.);
#18576=EDGE_CURVE('',#14700,#14701,#9478,.T.);
#18577=EDGE_CURVE('',#14700,#14702,#9479,.T.);
#18578=EDGE_CURVE('',#14703,#14701,#9480,.T.);
#18579=EDGE_CURVE('',#14702,#14703,#9481,.T.);
#18580=EDGE_CURVE('',#14702,#14704,#2870,.T.);
#18581=EDGE_CURVE('',#14705,#14703,#2871,.T.);
#18582=EDGE_CURVE('',#14704,#14705,#9482,.T.);
#18583=EDGE_CURVE('',#14704,#14690,#9483,.T.);
#18584=EDGE_CURVE('',#14692,#14705,#9484,.T.);
#18585=EDGE_CURVE('',#14706,#14707,#2872,.T.);
#18586=EDGE_CURVE('',#14706,#14708,#9485,.T.);
#18587=EDGE_CURVE('',#14709,#14708,#2873,.T.);
#18588=EDGE_CURVE('',#14707,#14709,#9486,.T.);
#18589=EDGE_CURVE('',#14710,#14706,#9487,.T.);
#18590=EDGE_CURVE('',#14710,#14711,#9488,.T.);
#18591=EDGE_CURVE('',#14708,#14711,#9489,.T.);
#18592=EDGE_CURVE('',#14712,#14710,#2874,.T.);
#18593=EDGE_CURVE('',#14712,#14713,#9490,.T.);
#18594=EDGE_CURVE('',#14711,#14713,#2875,.T.);
#18595=EDGE_CURVE('',#14714,#14712,#9491,.T.);
#18596=EDGE_CURVE('',#14714,#14715,#9492,.T.);
#18597=EDGE_CURVE('',#14713,#14715,#9493,.T.);
#18598=EDGE_CURVE('',#14716,#14714,#2876,.T.);
#18599=EDGE_CURVE('',#14716,#14717,#9494,.T.);
#18600=EDGE_CURVE('',#14715,#14717,#2877,.T.);
#18601=EDGE_CURVE('',#14718,#14716,#9495,.T.);
#18602=EDGE_CURVE('',#14718,#14719,#9496,.T.);
#18603=EDGE_CURVE('',#14717,#14719,#9497,.T.);
#18604=EDGE_CURVE('',#14720,#14718,#2878,.T.);
#18605=EDGE_CURVE('',#14720,#14721,#9498,.T.);
#18606=EDGE_CURVE('',#14719,#14721,#2879,.T.);
#18607=EDGE_CURVE('',#14707,#14720,#9499,.T.);
#18608=EDGE_CURVE('',#14721,#14709,#9500,.T.);
#18609=EDGE_CURVE('',#14722,#14723,#2880,.T.);
#18610=EDGE_CURVE('',#14722,#14724,#9501,.T.);
#18611=EDGE_CURVE('',#14725,#14724,#2881,.T.);
#18612=EDGE_CURVE('',#14723,#14725,#9502,.T.);
#18613=EDGE_CURVE('',#14723,#14726,#9503,.T.);
#18614=EDGE_CURVE('',#14727,#14725,#9504,.T.);
#18615=EDGE_CURVE('',#14726,#14727,#9505,.T.);
#18616=EDGE_CURVE('',#14726,#14728,#2882,.T.);
#18617=EDGE_CURVE('',#14729,#14727,#2883,.T.);
#18618=EDGE_CURVE('',#14728,#14729,#9506,.T.);
#18619=EDGE_CURVE('',#14728,#14730,#9507,.T.);
#18620=EDGE_CURVE('',#14731,#14729,#9508,.T.);
#18621=EDGE_CURVE('',#14730,#14731,#9509,.T.);
#18622=EDGE_CURVE('',#14730,#14732,#2884,.T.);
#18623=EDGE_CURVE('',#14733,#14731,#2885,.T.);
#18624=EDGE_CURVE('',#14732,#14733,#9510,.T.);
#18625=EDGE_CURVE('',#14732,#14734,#9511,.T.);
#18626=EDGE_CURVE('',#14735,#14733,#9512,.T.);
#18627=EDGE_CURVE('',#14734,#14735,#9513,.T.);
#18628=EDGE_CURVE('',#14734,#14736,#2886,.T.);
#18629=EDGE_CURVE('',#14737,#14735,#2887,.T.);
#18630=EDGE_CURVE('',#14736,#14737,#9514,.T.);
#18631=EDGE_CURVE('',#14736,#14722,#9515,.T.);
#18632=EDGE_CURVE('',#14724,#14737,#9516,.T.);
#18633=EDGE_CURVE('',#14738,#14739,#2888,.T.);
#18634=EDGE_CURVE('',#14738,#14740,#9517,.T.);
#18635=EDGE_CURVE('',#14741,#14740,#2889,.T.);
#18636=EDGE_CURVE('',#14739,#14741,#9518,.T.);
#18637=EDGE_CURVE('',#14742,#14738,#9519,.T.);
#18638=EDGE_CURVE('',#14742,#14743,#9520,.T.);
#18639=EDGE_CURVE('',#14740,#14743,#9521,.T.);
#18640=EDGE_CURVE('',#14744,#14742,#2890,.T.);
#18641=EDGE_CURVE('',#14744,#14745,#9522,.T.);
#18642=EDGE_CURVE('',#14743,#14745,#2891,.T.);
#18643=EDGE_CURVE('',#14746,#14744,#9523,.T.);
#18644=EDGE_CURVE('',#14746,#14747,#9524,.T.);
#18645=EDGE_CURVE('',#14745,#14747,#9525,.T.);
#18646=EDGE_CURVE('',#14748,#14746,#2892,.T.);
#18647=EDGE_CURVE('',#14748,#14749,#9526,.T.);
#18648=EDGE_CURVE('',#14747,#14749,#2893,.T.);
#18649=EDGE_CURVE('',#14750,#14748,#9527,.T.);
#18650=EDGE_CURVE('',#14750,#14751,#9528,.T.);
#18651=EDGE_CURVE('',#14749,#14751,#9529,.T.);
#18652=EDGE_CURVE('',#14752,#14750,#2894,.T.);
#18653=EDGE_CURVE('',#14752,#14753,#9530,.T.);
#18654=EDGE_CURVE('',#14751,#14753,#2895,.T.);
#18655=EDGE_CURVE('',#14739,#14752,#9531,.T.);
#18656=EDGE_CURVE('',#14753,#14741,#9532,.T.);
#18657=EDGE_CURVE('',#14754,#14755,#2896,.T.);
#18658=EDGE_CURVE('',#14754,#14756,#9533,.T.);
#18659=EDGE_CURVE('',#14757,#14756,#2897,.T.);
#18660=EDGE_CURVE('',#14755,#14757,#9534,.T.);
#18661=EDGE_CURVE('',#14755,#14758,#9535,.T.);
#18662=EDGE_CURVE('',#14759,#14757,#9536,.T.);
#18663=EDGE_CURVE('',#14758,#14759,#9537,.T.);
#18664=EDGE_CURVE('',#14758,#14760,#2898,.T.);
#18665=EDGE_CURVE('',#14761,#14759,#2899,.T.);
#18666=EDGE_CURVE('',#14760,#14761,#9538,.T.);
#18667=EDGE_CURVE('',#14760,#14762,#9539,.T.);
#18668=EDGE_CURVE('',#14763,#14761,#9540,.T.);
#18669=EDGE_CURVE('',#14762,#14763,#9541,.T.);
#18670=EDGE_CURVE('',#14762,#14764,#2900,.T.);
#18671=EDGE_CURVE('',#14765,#14763,#2901,.T.);
#18672=EDGE_CURVE('',#14764,#14765,#9542,.T.);
#18673=EDGE_CURVE('',#14764,#14766,#9543,.T.);
#18674=EDGE_CURVE('',#14767,#14765,#9544,.T.);
#18675=EDGE_CURVE('',#14766,#14767,#9545,.T.);
#18676=EDGE_CURVE('',#14766,#14768,#2902,.T.);
#18677=EDGE_CURVE('',#14769,#14767,#2903,.T.);
#18678=EDGE_CURVE('',#14768,#14769,#9546,.T.);
#18679=EDGE_CURVE('',#14768,#14754,#9547,.T.);
#18680=EDGE_CURVE('',#14756,#14769,#9548,.T.);
#18681=EDGE_CURVE('',#14770,#14771,#2904,.T.);
#18682=EDGE_CURVE('',#14770,#14772,#9549,.T.);
#18683=EDGE_CURVE('',#14773,#14772,#2905,.T.);
#18684=EDGE_CURVE('',#14771,#14773,#9550,.T.);
#18685=EDGE_CURVE('',#14774,#14770,#9551,.T.);
#18686=EDGE_CURVE('',#14774,#14775,#9552,.T.);
#18687=EDGE_CURVE('',#14772,#14775,#9553,.T.);
#18688=EDGE_CURVE('',#14776,#14774,#2906,.T.);
#18689=EDGE_CURVE('',#14776,#14777,#9554,.T.);
#18690=EDGE_CURVE('',#14775,#14777,#2907,.T.);
#18691=EDGE_CURVE('',#14778,#14776,#9555,.T.);
#18692=EDGE_CURVE('',#14778,#14779,#9556,.T.);
#18693=EDGE_CURVE('',#14777,#14779,#9557,.T.);
#18694=EDGE_CURVE('',#14780,#14778,#2908,.T.);
#18695=EDGE_CURVE('',#14780,#14781,#9558,.T.);
#18696=EDGE_CURVE('',#14779,#14781,#2909,.T.);
#18697=EDGE_CURVE('',#14782,#14780,#9559,.T.);
#18698=EDGE_CURVE('',#14782,#14783,#9560,.T.);
#18699=EDGE_CURVE('',#14781,#14783,#9561,.T.);
#18700=EDGE_CURVE('',#14784,#14782,#2910,.T.);
#18701=EDGE_CURVE('',#14784,#14785,#9562,.T.);
#18702=EDGE_CURVE('',#14783,#14785,#2911,.T.);
#18703=EDGE_CURVE('',#14771,#14784,#9563,.T.);
#18704=EDGE_CURVE('',#14785,#14773,#9564,.T.);
#18705=EDGE_CURVE('',#14786,#14787,#2912,.T.);
#18706=EDGE_CURVE('',#14786,#14788,#9565,.T.);
#18707=EDGE_CURVE('',#14789,#14788,#2913,.T.);
#18708=EDGE_CURVE('',#14787,#14789,#9566,.T.);
#18709=EDGE_CURVE('',#14787,#14790,#9567,.T.);
#18710=EDGE_CURVE('',#14791,#14789,#9568,.T.);
#18711=EDGE_CURVE('',#14790,#14791,#9569,.T.);
#18712=EDGE_CURVE('',#14790,#14792,#2914,.T.);
#18713=EDGE_CURVE('',#14793,#14791,#2915,.T.);
#18714=EDGE_CURVE('',#14792,#14793,#9570,.T.);
#18715=EDGE_CURVE('',#14792,#14794,#9571,.T.);
#18716=EDGE_CURVE('',#14795,#14793,#9572,.T.);
#18717=EDGE_CURVE('',#14794,#14795,#9573,.T.);
#18718=EDGE_CURVE('',#14794,#14796,#2916,.T.);
#18719=EDGE_CURVE('',#14797,#14795,#2917,.T.);
#18720=EDGE_CURVE('',#14796,#14797,#9574,.T.);
#18721=EDGE_CURVE('',#14796,#14798,#9575,.T.);
#18722=EDGE_CURVE('',#14799,#14797,#9576,.T.);
#18723=EDGE_CURVE('',#14798,#14799,#9577,.T.);
#18724=EDGE_CURVE('',#14798,#14800,#2918,.T.);
#18725=EDGE_CURVE('',#14801,#14799,#2919,.T.);
#18726=EDGE_CURVE('',#14800,#14801,#9578,.T.);
#18727=EDGE_CURVE('',#14800,#14786,#9579,.T.);
#18728=EDGE_CURVE('',#14788,#14801,#9580,.T.);
#18729=EDGE_CURVE('',#14802,#14802,#2920,.T.);
#18730=EDGE_CURVE('',#14802,#14803,#9581,.T.);
#18731=EDGE_CURVE('',#14803,#14803,#2921,.T.);
#18732=EDGE_CURVE('',#14804,#14804,#2922,.T.);
#18733=EDGE_CURVE('',#14804,#14805,#9582,.T.);
#18734=EDGE_CURVE('',#14805,#14805,#2923,.T.);
#18735=EDGE_CURVE('',#14806,#14806,#2924,.T.);
#18736=EDGE_CURVE('',#14806,#14807,#9583,.T.);
#18737=EDGE_CURVE('',#14807,#14807,#2925,.T.);
#18738=EDGE_CURVE('',#14808,#14808,#2926,.T.);
#18739=EDGE_CURVE('',#14808,#14809,#9584,.T.);
#18740=EDGE_CURVE('',#14809,#14809,#2927,.T.);
#18741=EDGE_CURVE('',#14810,#14810,#2928,.T.);
#18742=EDGE_CURVE('',#14810,#14811,#9585,.T.);
#18743=EDGE_CURVE('',#14811,#14811,#2929,.T.);
#18744=EDGE_CURVE('',#14812,#14812,#2930,.T.);
#18745=EDGE_CURVE('',#14812,#14813,#9586,.T.);
#18746=EDGE_CURVE('',#14813,#14813,#2931,.T.);
#18747=EDGE_CURVE('',#14814,#14814,#2932,.T.);
#18748=EDGE_CURVE('',#14814,#14815,#9587,.T.);
#18749=EDGE_CURVE('',#14815,#14815,#2933,.T.);
#18750=EDGE_CURVE('',#14816,#14816,#2934,.T.);
#18751=EDGE_CURVE('',#14816,#14817,#9588,.T.);
#18752=EDGE_CURVE('',#14817,#14817,#2935,.T.);
#18753=EDGE_CURVE('',#14818,#14818,#2936,.T.);
#18754=EDGE_CURVE('',#14818,#14819,#9589,.T.);
#18755=EDGE_CURVE('',#14819,#14819,#2937,.T.);
#18756=EDGE_CURVE('',#14820,#14820,#2938,.T.);
#18757=EDGE_CURVE('',#14820,#14821,#9590,.T.);
#18758=EDGE_CURVE('',#14821,#14821,#2939,.T.);
#18759=EDGE_CURVE('',#14822,#14822,#2940,.T.);
#18760=EDGE_CURVE('',#14822,#14823,#9591,.T.);
#18761=EDGE_CURVE('',#14823,#14823,#2941,.T.);
#18762=EDGE_CURVE('',#14824,#14824,#2942,.T.);
#18763=EDGE_CURVE('',#14824,#14825,#9592,.T.);
#18764=EDGE_CURVE('',#14825,#14825,#2943,.T.);
#18765=EDGE_CURVE('',#14826,#14826,#2944,.T.);
#18766=EDGE_CURVE('',#14826,#14827,#9593,.T.);
#18767=EDGE_CURVE('',#14827,#14827,#2945,.T.);
#18768=EDGE_CURVE('',#14828,#14828,#2946,.T.);
#18769=EDGE_CURVE('',#14828,#14829,#9594,.T.);
#18770=EDGE_CURVE('',#14829,#14829,#2947,.T.);
#18771=EDGE_CURVE('',#14830,#14830,#2948,.T.);
#18772=EDGE_CURVE('',#14830,#14831,#9595,.T.);
#18773=EDGE_CURVE('',#14831,#14831,#2949,.T.);
#18774=EDGE_CURVE('',#14832,#14832,#2950,.T.);
#18775=EDGE_CURVE('',#14832,#14833,#9596,.T.);
#18776=EDGE_CURVE('',#14833,#14833,#2951,.T.);
#18777=EDGE_CURVE('',#14834,#14835,#9597,.T.);
#18778=EDGE_CURVE('',#14836,#14835,#9598,.T.);
#18779=EDGE_CURVE('',#14836,#14837,#9599,.T.);
#18780=EDGE_CURVE('',#14834,#14837,#9600,.T.);
#18781=EDGE_CURVE('',#14838,#14836,#9601,.T.);
#18782=EDGE_CURVE('',#14838,#14839,#9602,.T.);
#18783=EDGE_CURVE('',#14837,#14839,#9603,.T.);
#18784=EDGE_CURVE('',#14840,#14838,#9604,.T.);
#18785=EDGE_CURVE('',#14840,#14841,#9605,.T.);
#18786=EDGE_CURVE('',#14839,#14841,#9606,.T.);
#18787=EDGE_CURVE('',#14835,#14840,#9607,.T.);
#18788=EDGE_CURVE('',#14841,#14834,#9608,.T.);
#18789=EDGE_CURVE('',#14842,#14843,#9609,.T.);
#18790=EDGE_CURVE('',#14843,#14844,#9610,.T.);
#18791=EDGE_CURVE('',#14844,#14845,#9611,.T.);
#18792=EDGE_CURVE('',#14845,#14842,#9612,.T.);
#18793=EDGE_CURVE('',#14846,#14843,#9613,.T.);
#18794=EDGE_CURVE('',#14847,#14846,#9614,.T.);
#18795=EDGE_CURVE('',#14844,#14847,#9615,.T.);
#18796=EDGE_CURVE('',#14848,#14847,#9616,.T.);
#18797=EDGE_CURVE('',#14845,#14848,#9617,.T.);
#18798=EDGE_CURVE('',#14849,#14848,#9618,.T.);
#18799=EDGE_CURVE('',#14842,#14849,#9619,.T.);
#18800=EDGE_CURVE('',#14846,#14849,#9620,.T.);
#18801=EDGE_CURVE('',#14850,#14851,#9621,.T.);
#18802=EDGE_CURVE('',#14852,#14850,#9622,.T.);
#18803=EDGE_CURVE('',#14853,#14852,#9623,.T.);
#18804=EDGE_CURVE('',#14851,#14853,#9624,.T.);
#18805=EDGE_CURVE('',#14854,#14854,#2952,.T.);
#18806=EDGE_CURVE('',#14855,#14855,#2953,.T.);
#18807=EDGE_CURVE('',#14856,#14856,#2954,.T.);
#18808=EDGE_CURVE('',#14857,#14858,#9625,.T.);
#18809=EDGE_CURVE('',#14859,#14857,#9626,.T.);
#18810=EDGE_CURVE('',#14860,#14859,#9627,.T.);
#18811=EDGE_CURVE('',#14858,#14860,#9628,.T.);
#18812=EDGE_CURVE('',#14861,#14861,#2955,.T.);
#18813=EDGE_CURVE('',#14862,#14862,#2956,.T.);
#18814=EDGE_CURVE('',#14863,#14863,#2957,.T.);
#18815=EDGE_CURVE('',#14858,#14850,#9629,.T.);
#18816=EDGE_CURVE('',#14852,#14860,#9630,.T.);
#18817=EDGE_CURVE('',#14864,#14865,#9631,.T.);
#18818=EDGE_CURVE('',#14865,#14865,#2958,.T.);
#18819=EDGE_CURVE('',#14861,#14865,#9632,.T.);
#18820=EDGE_CURVE('',#14866,#14867,#9633,.T.);
#18821=EDGE_CURVE('',#14867,#14867,#2959,.T.);
#18822=EDGE_CURVE('',#14862,#14867,#9634,.T.);
#18823=EDGE_CURVE('',#14868,#14869,#9635,.T.);
#18824=EDGE_CURVE('',#14869,#14869,#2960,.T.);
#18825=EDGE_CURVE('',#14863,#14869,#9636,.T.);
#18826=EDGE_CURVE('',#14870,#14871,#9637,.T.);
#18827=EDGE_CURVE('',#14871,#14871,#2961,.T.);
#18828=EDGE_CURVE('',#14871,#14854,#9638,.T.);
#18829=EDGE_CURVE('',#14872,#14873,#9639,.T.);
#18830=EDGE_CURVE('',#14873,#14873,#2962,.T.);
#18831=EDGE_CURVE('',#14873,#14855,#9640,.T.);
#18832=EDGE_CURVE('',#14874,#14875,#9641,.T.);
#18833=EDGE_CURVE('',#14875,#14875,#2963,.T.);
#18834=EDGE_CURVE('',#14875,#14856,#9642,.T.);
#18835=EDGE_CURVE('',#14876,#14876,#2964,.T.);
#18836=EDGE_CURVE('',#14876,#14877,#9643,.T.);
#18837=EDGE_CURVE('',#14877,#14877,#2965,.T.);
#18838=EDGE_CURVE('',#14878,#14878,#2966,.T.);
#18839=EDGE_CURVE('',#14878,#14879,#9644,.T.);
#18840=EDGE_CURVE('',#14879,#14879,#2967,.T.);
#18841=EDGE_CURVE('',#14880,#14880,#2968,.T.);
#18842=EDGE_CURVE('',#14880,#14881,#9645,.T.);
#18843=EDGE_CURVE('',#14881,#14881,#2969,.T.);
#18844=EDGE_CURVE('',#14882,#14882,#2970,.T.);
#18845=EDGE_CURVE('',#14882,#14883,#9646,.T.);
#18846=EDGE_CURVE('',#14883,#14883,#2971,.T.);
#18847=EDGE_CURVE('',#14884,#14884,#2972,.T.);
#18848=EDGE_CURVE('',#14884,#14885,#9647,.T.);
#18849=EDGE_CURVE('',#14885,#14885,#2973,.T.);
#18850=EDGE_CURVE('',#14886,#14886,#2974,.T.);
#18851=EDGE_CURVE('',#14886,#14887,#9648,.T.);
#18852=EDGE_CURVE('',#14887,#14887,#2975,.T.);
#18853=EDGE_CURVE('',#14888,#14888,#2976,.T.);
#18854=EDGE_CURVE('',#14888,#14889,#9649,.T.);
#18855=EDGE_CURVE('',#14889,#14889,#2977,.T.);
#18856=EDGE_CURVE('',#14890,#14890,#2978,.T.);
#18857=EDGE_CURVE('',#14890,#14891,#9650,.T.);
#18858=EDGE_CURVE('',#14891,#14891,#2979,.T.);
#18859=EDGE_CURVE('',#14892,#14892,#2980,.T.);
#18860=EDGE_CURVE('',#14892,#14893,#9651,.T.);
#18861=EDGE_CURVE('',#14893,#14893,#2981,.T.);
#18862=EDGE_CURVE('',#14894,#14894,#2982,.T.);
#18863=EDGE_CURVE('',#14894,#14895,#9652,.T.);
#18864=EDGE_CURVE('',#14895,#14895,#2983,.T.);
#18865=EDGE_CURVE('',#14851,#14857,#9653,.T.);
#18866=EDGE_CURVE('',#14859,#14853,#9654,.T.);
#18867=EDGE_CURVE('',#14896,#14897,#9655,.T.);
#18868=EDGE_CURVE('',#14898,#14896,#9656,.T.);
#18869=EDGE_CURVE('',#14899,#14898,#9657,.T.);
#18870=EDGE_CURVE('',#14897,#14899,#9658,.T.);
#18871=EDGE_CURVE('',#14900,#14900,#2984,.T.);
#18872=EDGE_CURVE('',#14901,#14901,#2985,.T.);
#18873=EDGE_CURVE('',#14902,#14902,#2986,.T.);
#18874=EDGE_CURVE('',#14903,#14904,#9659,.T.);
#18875=EDGE_CURVE('',#14905,#14903,#9660,.T.);
#18876=EDGE_CURVE('',#14906,#14905,#9661,.T.);
#18877=EDGE_CURVE('',#14904,#14906,#9662,.T.);
#18878=EDGE_CURVE('',#14907,#14907,#2987,.T.);
#18879=EDGE_CURVE('',#14908,#14908,#2988,.T.);
#18880=EDGE_CURVE('',#14909,#14909,#2989,.T.);
#18881=EDGE_CURVE('',#14904,#14896,#9663,.T.);
#18882=EDGE_CURVE('',#14898,#14906,#9664,.T.);
#18883=EDGE_CURVE('',#14910,#14911,#9665,.T.);
#18884=EDGE_CURVE('',#14911,#14911,#2990,.T.);
#18885=EDGE_CURVE('',#14900,#14911,#9666,.T.);
#18886=EDGE_CURVE('',#14912,#14913,#9667,.T.);
#18887=EDGE_CURVE('',#14913,#14913,#2991,.T.);
#18888=EDGE_CURVE('',#14901,#14913,#9668,.T.);
#18889=EDGE_CURVE('',#14914,#14915,#9669,.T.);
#18890=EDGE_CURVE('',#14915,#14915,#2992,.T.);
#18891=EDGE_CURVE('',#14902,#14915,#9670,.T.);
#18892=EDGE_CURVE('',#14916,#14917,#9671,.T.);
#18893=EDGE_CURVE('',#14917,#14917,#2993,.T.);
#18894=EDGE_CURVE('',#14917,#14909,#9672,.T.);
#18895=EDGE_CURVE('',#14918,#14919,#9673,.T.);
#18896=EDGE_CURVE('',#14919,#14919,#2994,.T.);
#18897=EDGE_CURVE('',#14919,#14908,#9674,.T.);
#18898=EDGE_CURVE('',#14920,#14921,#9675,.T.);
#18899=EDGE_CURVE('',#14921,#14921,#2995,.T.);
#18900=EDGE_CURVE('',#14921,#14907,#9676,.T.);
#18901=EDGE_CURVE('',#14922,#14922,#2996,.T.);
#18902=EDGE_CURVE('',#14922,#14923,#9677,.T.);
#18903=EDGE_CURVE('',#14923,#14923,#2997,.T.);
#18904=EDGE_CURVE('',#14924,#14924,#2998,.T.);
#18905=EDGE_CURVE('',#14924,#14925,#9678,.T.);
#18906=EDGE_CURVE('',#14925,#14925,#2999,.T.);
#18907=EDGE_CURVE('',#14926,#14926,#3000,.T.);
#18908=EDGE_CURVE('',#14926,#14927,#9679,.T.);
#18909=EDGE_CURVE('',#14927,#14927,#3001,.T.);
#18910=EDGE_CURVE('',#14928,#14928,#3002,.T.);
#18911=EDGE_CURVE('',#14928,#14929,#9680,.T.);
#18912=EDGE_CURVE('',#14929,#14929,#3003,.T.);
#18913=EDGE_CURVE('',#14930,#14930,#3004,.T.);
#18914=EDGE_CURVE('',#14930,#14931,#9681,.T.);
#18915=EDGE_CURVE('',#14931,#14931,#3005,.T.);
#18916=EDGE_CURVE('',#14932,#14932,#3006,.T.);
#18917=EDGE_CURVE('',#14932,#14933,#9682,.T.);
#18918=EDGE_CURVE('',#14933,#14933,#3007,.T.);
#18919=EDGE_CURVE('',#14934,#14934,#3008,.T.);
#18920=EDGE_CURVE('',#14934,#14935,#9683,.T.);
#18921=EDGE_CURVE('',#14935,#14935,#3009,.T.);
#18922=EDGE_CURVE('',#14936,#14936,#3010,.T.);
#18923=EDGE_CURVE('',#14936,#14937,#9684,.T.);
#18924=EDGE_CURVE('',#14937,#14937,#3011,.T.);
#18925=EDGE_CURVE('',#14938,#14938,#3012,.T.);
#18926=EDGE_CURVE('',#14938,#14939,#9685,.T.);
#18927=EDGE_CURVE('',#14939,#14939,#3013,.T.);
#18928=EDGE_CURVE('',#14940,#14940,#3014,.T.);
#18929=EDGE_CURVE('',#14940,#14941,#9686,.T.);
#18930=EDGE_CURVE('',#14941,#14941,#3015,.T.);
#18931=EDGE_CURVE('',#14897,#14903,#9687,.T.);
#18932=EDGE_CURVE('',#14905,#14899,#9688,.T.);
#18933=EDGE_CURVE('',#14942,#14942,#3016,.T.);
#18934=EDGE_CURVE('',#14942,#14943,#9689,.T.);
#18935=EDGE_CURVE('',#14943,#14943,#3017,.T.);
#18936=EDGE_CURVE('',#14944,#14944,#3018,.T.);
#18937=EDGE_CURVE('',#14944,#14945,#9690,.T.);
#18938=EDGE_CURVE('',#14945,#14945,#3019,.T.);
#18939=EDGE_CURVE('',#14946,#14946,#3020,.T.);
#18940=EDGE_CURVE('',#14946,#14947,#9691,.T.);
#18941=EDGE_CURVE('',#14947,#14947,#3021,.T.);
#18942=EDGE_CURVE('',#14948,#14948,#3022,.T.);
#18943=EDGE_CURVE('',#14948,#14949,#9692,.T.);
#18944=EDGE_CURVE('',#14949,#14949,#3023,.T.);
#18945=EDGE_CURVE('',#14950,#14950,#3024,.T.);
#18946=EDGE_CURVE('',#14950,#14951,#9693,.T.);
#18947=EDGE_CURVE('',#14951,#14951,#3025,.T.);
#18948=EDGE_CURVE('',#14952,#14952,#3026,.T.);
#18949=EDGE_CURVE('',#14952,#14953,#9694,.T.);
#18950=EDGE_CURVE('',#14953,#14953,#3027,.T.);
#18951=EDGE_CURVE('',#14954,#14955,#9695,.T.);
#18952=EDGE_CURVE('',#14955,#14956,#9696,.T.);
#18953=EDGE_CURVE('',#14957,#14956,#9697,.T.);
#18954=EDGE_CURVE('',#14954,#14957,#9698,.T.);
#18955=EDGE_CURVE('',#14958,#14954,#9699,.T.);
#18956=EDGE_CURVE('',#14959,#14957,#9700,.T.);
#18957=EDGE_CURVE('',#14958,#14959,#9701,.T.);
#18958=EDGE_CURVE('',#14960,#14958,#9702,.T.);
#18959=EDGE_CURVE('',#14961,#14959,#9703,.T.);
#18960=EDGE_CURVE('',#14960,#14961,#9704,.T.);
#18961=EDGE_CURVE('',#14955,#14960,#9705,.T.);
#18962=EDGE_CURVE('',#14956,#14961,#9706,.T.);
#18963=EDGE_CURVE('',#14962,#14963,#9707,.T.);
#18964=EDGE_CURVE('',#14964,#14962,#9708,.T.);
#18965=EDGE_CURVE('',#14965,#14964,#9709,.T.);
#18966=EDGE_CURVE('',#14963,#14965,#9710,.T.);
#18967=EDGE_CURVE('',#14965,#14966,#9711,.T.);
#18968=EDGE_CURVE('',#14967,#14966,#9712,.T.);
#18969=EDGE_CURVE('',#14967,#14963,#9713,.T.);
#18970=EDGE_CURVE('',#14964,#14968,#9714,.T.);
#18971=EDGE_CURVE('',#14969,#14968,#9715,.T.);
#18972=EDGE_CURVE('',#14970,#14969,#9716,.T.);
#18973=EDGE_CURVE('',#14970,#14971,#3028,.T.);
#18974=EDGE_CURVE('',#14972,#14971,#9717,.T.);
#18975=EDGE_CURVE('',#14966,#14972,#9718,.T.);
#18976=EDGE_CURVE('',#14971,#14973,#9719,.T.);
#18977=EDGE_CURVE('',#14974,#14970,#9720,.T.);
#18978=EDGE_CURVE('',#14973,#14974,#3029,.T.);
#18979=EDGE_CURVE('',#14975,#14967,#9721,.T.);
#18980=EDGE_CURVE('',#14973,#14975,#9722,.T.);
#18981=EDGE_CURVE('',#14976,#14974,#9723,.T.);
#18982=EDGE_CURVE('',#14977,#14976,#9724,.T.);
#18983=EDGE_CURVE('',#14977,#14962,#9725,.T.);
#18984=EDGE_CURVE('',#14976,#14969,#9726,.T.);
#18985=EDGE_CURVE('',#14972,#14975,#9727,.T.);
#18986=EDGE_CURVE('',#14968,#14977,#9728,.T.);
#18987=EDGE_CURVE('',#14978,#14978,#3030,.T.);
#18988=EDGE_CURVE('',#14978,#14979,#9729,.T.);
#18989=EDGE_CURVE('',#14979,#14979,#3031,.T.);
#18990=EDGE_CURVE('',#14980,#14980,#3032,.T.);
#18991=EDGE_CURVE('',#14980,#14981,#9730,.T.);
#18992=EDGE_CURVE('',#14981,#14981,#3033,.T.);
#18993=EDGE_CURVE('',#14982,#14982,#3034,.T.);
#18994=EDGE_CURVE('',#14982,#14983,#9731,.T.);
#18995=EDGE_CURVE('',#14983,#14983,#3035,.T.);
#18996=EDGE_CURVE('',#14984,#14984,#3036,.T.);
#18997=EDGE_CURVE('',#14984,#14985,#9732,.T.);
#18998=EDGE_CURVE('',#14985,#14985,#3037,.T.);
#18999=EDGE_CURVE('',#14986,#14987,#9733,.T.);
#19000=EDGE_CURVE('',#14986,#14988,#9734,.T.);
#19001=EDGE_CURVE('',#14989,#14988,#9735,.T.);
#19002=EDGE_CURVE('',#14987,#14989,#9736,.T.);
#19003=EDGE_CURVE('',#14990,#14986,#9737,.T.);
#19004=EDGE_CURVE('',#14990,#14991,#9738,.T.);
#19005=EDGE_CURVE('',#14988,#14991,#9739,.T.);
#19006=EDGE_CURVE('',#14992,#14990,#9740,.T.);
#19007=EDGE_CURVE('',#14992,#14993,#9741,.T.);
#19008=EDGE_CURVE('',#14991,#14993,#9742,.T.);
#19009=EDGE_CURVE('',#14987,#14992,#9743,.T.);
#19010=EDGE_CURVE('',#14993,#14989,#9744,.T.);
#19011=EDGE_CURVE('',#14994,#14995,#9745,.T.);
#19012=EDGE_CURVE('',#14995,#14996,#9746,.T.);
#19013=EDGE_CURVE('',#14997,#14996,#9747,.T.);
#19014=EDGE_CURVE('',#14994,#14997,#9748,.T.);
#19015=EDGE_CURVE('',#14998,#14994,#9749,.T.);
#19016=EDGE_CURVE('',#14999,#14997,#9750,.T.);
#19017=EDGE_CURVE('',#14998,#14999,#9751,.T.);
#19018=EDGE_CURVE('',#15000,#14998,#9752,.T.);
#19019=EDGE_CURVE('',#15001,#14999,#9753,.T.);
#19020=EDGE_CURVE('',#15000,#15001,#9754,.T.);
#19021=EDGE_CURVE('',#14995,#15000,#9755,.T.);
#19022=EDGE_CURVE('',#14996,#15001,#9756,.T.);
#19023=EDGE_CURVE('',#15002,#15003,#9757,.T.);
#19024=EDGE_CURVE('',#15004,#15002,#3038,.T.);
#19025=EDGE_CURVE('',#15004,#15005,#819,.T.);
#19026=EDGE_CURVE('',#15005,#15006,#9758,.T.);
#19027=EDGE_CURVE('',#15006,#15007,#820,.T.);
#19028=EDGE_CURVE('',#15007,#15003,#3039,.T.);
#19029=EDGE_CURVE('',#15008,#15009,#821,.T.);
#19030=EDGE_CURVE('',#15008,#15010,#9759,.T.);
#19031=EDGE_CURVE('',#15010,#15011,#3040,.T.);
#19032=EDGE_CURVE('',#15009,#15011,#9760,.T.);
#19033=EDGE_CURVE('',#15009,#15012,#9761,.T.);
#19034=EDGE_CURVE('',#15011,#15013,#9762,.T.);
#19035=EDGE_CURVE('',#15012,#15013,#9763,.T.);
#19036=EDGE_CURVE('',#15014,#15008,#9764,.T.);
#19037=EDGE_CURVE('',#15014,#15015,#9765,.T.);
#19038=EDGE_CURVE('',#15015,#15010,#9766,.T.);
#19039=EDGE_CURVE('',#15012,#15014,#822,.F.);
#19040=EDGE_CURVE('',#15013,#15015,#3041,.T.);
#19041=EDGE_CURVE('',#15016,#15017,#3042,.T.);
#19042=EDGE_CURVE('',#15017,#15016,#3043,.T.);
#19043=EDGE_CURVE('',#15016,#15018,#3044,.T.);
#19044=EDGE_CURVE('',#15018,#15018,#3045,.T.);
#19045=EDGE_CURVE('',#15019,#15019,#3046,.T.);
#19046=EDGE_CURVE('',#15020,#15020,#3047,.T.);
#19047=EDGE_CURVE('',#15020,#15017,#9767,.T.);
#19048=EDGE_CURVE('',#15021,#15021,#3048,.T.);
#19049=EDGE_CURVE('',#15021,#15022,#3049,.T.);
#19050=EDGE_CURVE('',#15022,#15023,#3050,.T.);
#19051=EDGE_CURVE('',#15023,#15022,#3051,.T.);
#19052=EDGE_CURVE('',#15024,#15024,#3052,.T.);
#19053=EDGE_CURVE('',#15023,#15025,#9768,.T.);
#19054=EDGE_CURVE('',#15026,#15025,#3053,.T.);
#19055=EDGE_CURVE('',#15025,#15026,#3054,.T.);
#19056=EDGE_CURVE('',#15027,#15028,#3055,.T.);
#19057=EDGE_CURVE('',#15028,#15027,#3056,.T.);
#19058=EDGE_CURVE('',#15027,#15024,#9769,.T.);
#19059=EDGE_CURVE('',#15029,#15030,#3057,.T.);
#19060=EDGE_CURVE('',#15029,#15028,#9770,.T.);
#19061=EDGE_CURVE('',#15030,#15029,#3058,.T.);
#19062=EDGE_CURVE('',#15031,#15032,#3059,.T.);
#19063=EDGE_CURVE('',#15032,#15031,#3060,.T.);
#19064=EDGE_CURVE('',#15031,#15019,#9771,.T.);
#19065=EDGE_CURVE('',#15032,#15033,#9772,.T.);
#19066=EDGE_CURVE('',#15033,#15034,#3061,.T.);
#19067=EDGE_CURVE('',#15034,#15033,#3062,.T.);
#19068=EDGE_CURVE('',#15026,#15035,#9773,.T.);
#19069=EDGE_CURVE('',#15035,#15035,#3063,.T.);
#19070=EDGE_CURVE('',#15006,#15036,#9774,.T.);
#19071=EDGE_CURVE('',#15036,#15037,#3064,.T.);
#19072=EDGE_CURVE('',#15038,#15037,#9775,.T.);
#19073=EDGE_CURVE('',#15007,#15038,#823,.T.);
#19074=EDGE_CURVE('',#15038,#15039,#9776,.T.);
#19075=EDGE_CURVE('',#15037,#15040,#9777,.T.);
#19076=EDGE_CURVE('',#15039,#15040,#9778,.T.);
#19077=EDGE_CURVE('',#15005,#15041,#9779,.T.);
#19078=EDGE_CURVE('',#15041,#15036,#9780,.T.);
#19079=EDGE_CURVE('',#15039,#15004,#824,.T.);
#19080=EDGE_CURVE('',#15040,#15041,#3065,.T.);
#19081=EDGE_CURVE('',#15003,#15007,#3066,.T.);
#19082=EDGE_CURVE('',#15002,#15004,#3067,.T.);
#19083=EDGE_CURVE('',#15020,#15042,#9781,.T.);
#19084=EDGE_CURVE('',#15042,#15042,#3068,.T.);
#19085=EDGE_CURVE('',#15043,#15043,#3069,.T.);
#19086=EDGE_CURVE('',#15043,#15030,#3070,.T.);
#19087=EDGE_CURVE('',#15044,#15044,#3071,.T.);
#19088=EDGE_CURVE('',#15003,#15044,#9782,.T.);
#19089=EDGE_CURVE('',#15002,#15045,#9783,.T.);
#19090=EDGE_CURVE('',#15045,#15045,#3072,.T.);
#19091=EDGE_CURVE('',#15046,#15046,#3073,.T.);
#19092=EDGE_CURVE('',#15034,#15046,#3074,.T.);
#19093=EDGE_CURVE('',#15047,#15048,#9784,.T.);
#19094=EDGE_CURVE('',#15049,#15047,#3075,.T.);
#19095=EDGE_CURVE('',#15049,#15050,#825,.T.);
#19096=EDGE_CURVE('',#15050,#15051,#9785,.T.);
#19097=EDGE_CURVE('',#15051,#15052,#826,.T.);
#19098=EDGE_CURVE('',#15052,#15048,#3076,.T.);
#19099=EDGE_CURVE('',#15053,#15054,#3077,.T.);
#19100=EDGE_CURVE('',#15054,#15053,#3078,.T.);
#19101=EDGE_CURVE('',#15053,#15055,#9786,.T.);
#19102=EDGE_CURVE('',#15055,#15055,#3079,.T.);
#19103=EDGE_CURVE('',#15054,#15056,#9787,.T.);
#19104=EDGE_CURVE('',#15056,#15056,#3080,.T.);
#19105=EDGE_CURVE('',#15057,#15058,#9788,.T.);
#19106=EDGE_CURVE('',#15058,#15059,#827,.T.);
#19107=EDGE_CURVE('',#15059,#15060,#9789,.T.);
#19108=EDGE_CURVE('',#15060,#15057,#828,.T.);
#19109=EDGE_CURVE('',#15061,#15062,#3081,.T.);
#19110=EDGE_CURVE('',#15062,#15061,#3082,.T.);
#19111=EDGE_CURVE('',#15061,#15063,#9790,.T.);
#19112=EDGE_CURVE('',#15063,#15063,#3083,.T.);
#19113=EDGE_CURVE('',#15062,#15064,#9791,.T.);
#19114=EDGE_CURVE('',#15065,#15064,#3084,.T.);
#19115=EDGE_CURVE('',#15064,#15065,#3085,.T.);
#19116=EDGE_CURVE('',#15059,#15066,#9792,.T.);
#19117=EDGE_CURVE('',#15066,#15067,#9793,.T.);
#19118=EDGE_CURVE('',#15060,#15067,#9794,.T.);
#19119=EDGE_CURVE('',#15067,#15068,#3086,.T.);
#19120=EDGE_CURVE('',#15057,#15068,#9795,.T.);
#19121=EDGE_CURVE('',#15068,#15069,#9796,.T.);
#19122=EDGE_CURVE('',#15058,#15069,#9797,.T.);
#19123=EDGE_CURVE('',#15069,#15066,#3087,.T.);
#19124=EDGE_CURVE('',#15070,#15071,#3088,.T.);
#19125=EDGE_CURVE('',#15071,#15070,#3089,.T.);
#19126=EDGE_CURVE('',#15070,#15072,#9798,.T.);
#19127=EDGE_CURVE('',#15072,#15072,#3090,.T.);
#19128=EDGE_CURVE('',#15073,#15073,#3091,.T.);
#19129=EDGE_CURVE('',#15074,#15075,#3092,.T.);
#19130=EDGE_CURVE('',#15074,#15071,#9799,.T.);
#19131=EDGE_CURVE('',#15075,#15074,#3093,.T.);
#19132=EDGE_CURVE('',#15073,#15076,#3094,.T.);
#19133=EDGE_CURVE('',#15076,#15077,#3095,.T.);
#19134=EDGE_CURVE('',#15077,#15076,#3096,.T.);
#19135=EDGE_CURVE('',#15077,#15078,#9800,.T.);
#19136=EDGE_CURVE('',#15079,#15078,#3097,.T.);
#19137=EDGE_CURVE('',#15078,#15079,#3098,.T.);
#19138=EDGE_CURVE('',#15065,#15080,#3099,.T.);
#19139=EDGE_CURVE('',#15080,#15080,#3100,.T.);
#19140=EDGE_CURVE('',#15081,#15081,#3101,.T.);
#19141=EDGE_CURVE('',#15082,#15083,#3102,.T.);
#19142=EDGE_CURVE('',#15083,#15082,#3103,.T.);
#19143=EDGE_CURVE('',#15082,#15081,#9801,.T.);
#19144=EDGE_CURVE('',#15083,#15084,#9802,.T.);
#19145=EDGE_CURVE('',#15084,#15085,#3104,.T.);
#19146=EDGE_CURVE('',#15085,#15084,#3105,.T.);
#19147=EDGE_CURVE('',#15079,#15086,#9803,.T.);
#19148=EDGE_CURVE('',#15086,#15086,#3106,.T.);
#19149=EDGE_CURVE('',#15051,#15087,#9804,.T.);
#19150=EDGE_CURVE('',#15087,#15088,#3107,.T.);
#19151=EDGE_CURVE('',#15089,#15088,#9805,.T.);
#19152=EDGE_CURVE('',#15052,#15089,#829,.T.);
#19153=EDGE_CURVE('',#15089,#15090,#9806,.T.);
#19154=EDGE_CURVE('',#15088,#15091,#9807,.T.);
#19155=EDGE_CURVE('',#15090,#15091,#9808,.T.);
#19156=EDGE_CURVE('',#15050,#15092,#9809,.T.);
#19157=EDGE_CURVE('',#15092,#15087,#9810,.T.);
#19158=EDGE_CURVE('',#15090,#15049,#830,.T.);
#19159=EDGE_CURVE('',#15091,#15092,#3108,.T.);
#19160=EDGE_CURVE('',#15048,#15052,#3109,.T.);
#19161=EDGE_CURVE('',#15047,#15049,#3110,.T.);
#19162=EDGE_CURVE('',#15093,#15093,#3111,.T.);
#19163=EDGE_CURVE('',#15093,#15075,#3112,.T.);
#19164=EDGE_CURVE('',#15094,#15094,#3113,.T.);
#19165=EDGE_CURVE('',#15048,#15094,#9811,.T.);
#19166=EDGE_CURVE('',#15047,#15095,#9812,.T.);
#19167=EDGE_CURVE('',#15095,#15095,#3114,.T.);
#19168=EDGE_CURVE('',#15096,#15096,#3115,.T.);
#19169=EDGE_CURVE('',#15085,#15096,#3116,.T.);
#19170=EDGE_CURVE('',#15097,#15098,#9813,.T.);
#19171=EDGE_CURVE('',#15099,#15097,#9814,.T.);
#19172=EDGE_CURVE('',#15099,#15100,#9815,.T.);
#19173=EDGE_CURVE('',#15098,#15100,#9816,.T.);
#19174=EDGE_CURVE('',#15101,#15099,#9817,.T.);
#19175=EDGE_CURVE('',#15101,#15102,#9818,.T.);
#19176=EDGE_CURVE('',#15100,#15102,#9819,.T.);
#19177=EDGE_CURVE('',#15103,#15104,#9820,.T.);
#19178=EDGE_CURVE('',#15102,#15103,#9821,.T.);
#19179=EDGE_CURVE('',#15104,#15101,#9822,.T.);
#19180=EDGE_CURVE('',#15105,#15105,#3117,.T.);
#19181=EDGE_CURVE('',#15103,#15098,#3118,.T.);
#19182=EDGE_CURVE('',#15097,#15104,#3119,.T.);
#19183=EDGE_CURVE('',#15106,#15106,#3120,.T.);
#19184=EDGE_CURVE('',#15106,#15105,#9823,.T.);
#19185=EDGE_CURVE('',#15107,#15107,#3121,.T.);
#19186=EDGE_CURVE('',#15107,#15108,#9824,.T.);
#19187=EDGE_CURVE('',#15108,#15108,#3122,.T.);
#19188=EDGE_CURVE('',#15109,#15109,#3123,.T.);
#19189=EDGE_CURVE('',#15109,#15110,#9825,.T.);
#19190=EDGE_CURVE('',#15110,#15110,#3124,.T.);
#19191=EDGE_CURVE('',#15111,#15111,#3125,.T.);
#19192=EDGE_CURVE('',#15111,#15112,#3126,.T.);
#19193=EDGE_CURVE('',#15112,#15113,#3127,.T.);
#19194=EDGE_CURVE('',#15113,#15112,#3128,.T.);
#19195=EDGE_CURVE('',#15113,#15114,#9826,.T.);
#19196=EDGE_CURVE('',#15114,#15114,#3129,.T.);
#19197=EDGE_CURVE('',#15115,#15116,#9827,.T.);
#19198=EDGE_CURVE('',#15116,#15117,#9828,.T.);
#19199=EDGE_CURVE('',#15117,#15118,#9829,.T.);
#19200=EDGE_CURVE('',#15118,#15115,#3130,.T.);
#19201=EDGE_CURVE('',#15119,#15119,#3131,.T.);
#19202=EDGE_CURVE('',#15119,#15114,#3132,.T.);
#19203=EDGE_CURVE('',#15120,#15121,#3133,.T.);
#19204=EDGE_CURVE('',#15121,#15122,#3134,.T.);
#19205=EDGE_CURVE('',#15122,#15123,#3135,.T.);
#19206=EDGE_CURVE('',#15124,#15123,#3136,.T.);
#19207=EDGE_CURVE('',#15124,#15125,#3137,.T.);
#19208=EDGE_CURVE('',#15125,#15126,#3138,.T.);
#19209=EDGE_CURVE('',#15126,#15127,#3139,.T.);
#19210=EDGE_CURVE('',#15128,#15127,#3140,.T.);
#19211=EDGE_CURVE('',#15128,#15129,#3141,.T.);
#19212=EDGE_CURVE('',#15129,#15130,#3142,.T.);
#19213=EDGE_CURVE('',#15130,#15131,#3143,.T.);
#19214=EDGE_CURVE('',#15132,#15131,#3144,.T.);
#19215=EDGE_CURVE('',#15132,#15133,#3145,.T.);
#19216=EDGE_CURVE('',#15133,#15134,#3146,.T.);
#19217=EDGE_CURVE('',#15134,#15135,#3147,.T.);
#19218=EDGE_CURVE('',#15136,#15135,#3148,.T.);
#19219=EDGE_CURVE('',#15136,#15137,#3149,.T.);
#19220=EDGE_CURVE('',#15137,#15138,#3150,.T.);
#19221=EDGE_CURVE('',#15138,#15139,#3151,.T.);
#19222=EDGE_CURVE('',#15140,#15139,#3152,.T.);
#19223=EDGE_CURVE('',#15140,#15141,#3153,.T.);
#19224=EDGE_CURVE('',#15141,#15142,#3154,.T.);
#19225=EDGE_CURVE('',#15142,#15143,#3155,.T.);
#19226=EDGE_CURVE('',#15144,#15143,#3156,.T.);
#19227=EDGE_CURVE('',#15144,#15145,#3157,.T.);
#19228=EDGE_CURVE('',#15145,#15146,#3158,.T.);
#19229=EDGE_CURVE('',#15146,#15147,#3159,.T.);
#19230=EDGE_CURVE('',#15148,#15147,#3160,.T.);
#19231=EDGE_CURVE('',#15148,#15149,#3161,.T.);
#19232=EDGE_CURVE('',#15149,#15150,#3162,.T.);
#19233=EDGE_CURVE('',#15150,#15151,#3163,.T.);
#19234=EDGE_CURVE('',#15152,#15151,#3164,.T.);
#19235=EDGE_CURVE('',#15152,#15153,#3165,.T.);
#19236=EDGE_CURVE('',#15153,#15154,#3166,.T.);
#19237=EDGE_CURVE('',#15154,#15155,#3167,.T.);
#19238=EDGE_CURVE('',#15156,#15155,#3168,.T.);
#19239=EDGE_CURVE('',#15156,#15157,#3169,.T.);
#19240=EDGE_CURVE('',#15157,#15158,#3170,.T.);
#19241=EDGE_CURVE('',#15158,#15159,#3171,.T.);
#19242=EDGE_CURVE('',#15160,#15159,#3172,.T.);
#19243=EDGE_CURVE('',#15160,#15161,#3173,.T.);
#19244=EDGE_CURVE('',#15161,#15162,#3174,.T.);
#19245=EDGE_CURVE('',#15162,#15163,#3175,.T.);
#19246=EDGE_CURVE('',#15164,#15163,#3176,.T.);
#19247=EDGE_CURVE('',#15164,#15165,#3177,.T.);
#19248=EDGE_CURVE('',#15165,#15166,#3178,.T.);
#19249=EDGE_CURVE('',#15166,#15167,#3179,.T.);
#19250=EDGE_CURVE('',#15168,#15167,#3180,.T.);
#19251=EDGE_CURVE('',#15168,#15169,#3181,.T.);
#19252=EDGE_CURVE('',#15169,#15170,#3182,.T.);
#19253=EDGE_CURVE('',#15170,#15171,#3183,.T.);
#19254=EDGE_CURVE('',#15172,#15171,#3184,.T.);
#19255=EDGE_CURVE('',#15172,#15173,#3185,.T.);
#19256=EDGE_CURVE('',#15173,#15174,#3186,.T.);
#19257=EDGE_CURVE('',#15174,#15175,#3187,.T.);
#19258=EDGE_CURVE('',#15176,#15175,#3188,.T.);
#19259=EDGE_CURVE('',#15176,#15177,#3189,.T.);
#19260=EDGE_CURVE('',#15177,#15178,#3190,.T.);
#19261=EDGE_CURVE('',#15178,#15179,#3191,.T.);
#19262=EDGE_CURVE('',#15180,#15179,#3192,.T.);
#19263=EDGE_CURVE('',#15180,#15181,#3193,.T.);
#19264=EDGE_CURVE('',#15181,#15182,#3194,.T.);
#19265=EDGE_CURVE('',#15182,#15183,#3195,.T.);
#19266=EDGE_CURVE('',#15184,#15183,#3196,.T.);
#19267=EDGE_CURVE('',#15184,#15185,#3197,.T.);
#19268=EDGE_CURVE('',#15185,#15186,#3198,.T.);
#19269=EDGE_CURVE('',#15186,#15187,#3199,.T.);
#19270=EDGE_CURVE('',#15188,#15187,#3200,.T.);
#19271=EDGE_CURVE('',#15188,#15189,#3201,.T.);
#19272=EDGE_CURVE('',#15189,#15190,#3202,.T.);
#19273=EDGE_CURVE('',#15190,#15191,#3203,.T.);
#19274=EDGE_CURVE('',#15192,#15191,#3204,.T.);
#19275=EDGE_CURVE('',#15192,#15193,#3205,.T.);
#19276=EDGE_CURVE('',#15193,#15194,#3206,.T.);
#19277=EDGE_CURVE('',#15194,#15195,#3207,.T.);
#19278=EDGE_CURVE('',#15196,#15195,#3208,.T.);
#19279=EDGE_CURVE('',#15196,#15197,#3209,.T.);
#19280=EDGE_CURVE('',#15197,#15198,#3210,.T.);
#19281=EDGE_CURVE('',#15198,#15199,#3211,.T.);
#19282=EDGE_CURVE('',#15200,#15199,#3212,.T.);
#19283=EDGE_CURVE('',#15200,#15201,#3213,.T.);
#19284=EDGE_CURVE('',#15201,#15202,#3214,.T.);
#19285=EDGE_CURVE('',#15202,#15203,#3215,.T.);
#19286=EDGE_CURVE('',#15204,#15203,#3216,.T.);
#19287=EDGE_CURVE('',#15204,#15205,#3217,.T.);
#19288=EDGE_CURVE('',#15205,#15206,#3218,.T.);
#19289=EDGE_CURVE('',#15206,#15207,#3219,.T.);
#19290=EDGE_CURVE('',#15208,#15207,#3220,.T.);
#19291=EDGE_CURVE('',#15208,#15209,#3221,.T.);
#19292=EDGE_CURVE('',#15209,#15210,#3222,.T.);
#19293=EDGE_CURVE('',#15210,#15211,#3223,.T.);
#19294=EDGE_CURVE('',#15212,#15211,#3224,.T.);
#19295=EDGE_CURVE('',#15212,#15213,#3225,.T.);
#19296=EDGE_CURVE('',#15213,#15214,#3226,.T.);
#19297=EDGE_CURVE('',#15214,#15215,#3227,.T.);
#19298=EDGE_CURVE('',#15216,#15215,#3228,.T.);
#19299=EDGE_CURVE('',#15216,#15217,#3229,.T.);
#19300=EDGE_CURVE('',#15217,#15218,#3230,.T.);
#19301=EDGE_CURVE('',#15218,#15219,#3231,.T.);
#19302=EDGE_CURVE('',#15220,#15219,#3232,.T.);
#19303=EDGE_CURVE('',#15220,#15221,#3233,.T.);
#19304=EDGE_CURVE('',#15221,#15222,#3234,.T.);
#19305=EDGE_CURVE('',#15222,#15223,#3235,.T.);
#19306=EDGE_CURVE('',#15224,#15223,#3236,.T.);
#19307=EDGE_CURVE('',#15224,#15225,#3237,.T.);
#19308=EDGE_CURVE('',#15225,#15226,#3238,.T.);
#19309=EDGE_CURVE('',#15226,#15227,#3239,.T.);
#19310=EDGE_CURVE('',#15228,#15227,#3240,.T.);
#19311=EDGE_CURVE('',#15228,#15229,#3241,.T.);
#19312=EDGE_CURVE('',#15229,#15230,#3242,.T.);
#19313=EDGE_CURVE('',#15230,#15231,#3243,.T.);
#19314=EDGE_CURVE('',#15232,#15231,#3244,.T.);
#19315=EDGE_CURVE('',#15232,#15233,#3245,.T.);
#19316=EDGE_CURVE('',#15233,#15234,#3246,.T.);
#19317=EDGE_CURVE('',#15234,#15235,#3247,.T.);
#19318=EDGE_CURVE('',#15236,#15235,#3248,.T.);
#19319=EDGE_CURVE('',#15236,#15237,#3249,.T.);
#19320=EDGE_CURVE('',#15237,#15238,#3250,.T.);
#19321=EDGE_CURVE('',#15238,#15239,#3251,.T.);
#19322=EDGE_CURVE('',#15240,#15239,#3252,.T.);
#19323=EDGE_CURVE('',#15240,#15241,#3253,.T.);
#19324=EDGE_CURVE('',#15241,#15242,#3254,.T.);
#19325=EDGE_CURVE('',#15242,#15243,#3255,.T.);
#19326=EDGE_CURVE('',#15244,#15243,#3256,.T.);
#19327=EDGE_CURVE('',#15244,#15245,#3257,.T.);
#19328=EDGE_CURVE('',#15245,#15246,#3258,.T.);
#19329=EDGE_CURVE('',#15246,#15247,#3259,.T.);
#19330=EDGE_CURVE('',#15248,#15247,#3260,.T.);
#19331=EDGE_CURVE('',#15248,#15249,#3261,.T.);
#19332=EDGE_CURVE('',#15249,#15250,#3262,.T.);
#19333=EDGE_CURVE('',#15250,#15251,#3263,.T.);
#19334=EDGE_CURVE('',#15252,#15251,#3264,.T.);
#19335=EDGE_CURVE('',#15252,#15253,#3265,.T.);
#19336=EDGE_CURVE('',#15253,#15254,#3266,.T.);
#19337=EDGE_CURVE('',#15254,#15255,#3267,.T.);
#19338=EDGE_CURVE('',#15256,#15255,#3268,.T.);
#19339=EDGE_CURVE('',#15256,#15257,#3269,.T.);
#19340=EDGE_CURVE('',#15257,#15258,#3270,.T.);
#19341=EDGE_CURVE('',#15258,#15259,#3271,.T.);
#19342=EDGE_CURVE('',#15260,#15259,#3272,.T.);
#19343=EDGE_CURVE('',#15260,#15261,#3273,.T.);
#19344=EDGE_CURVE('',#15261,#15262,#3274,.T.);
#19345=EDGE_CURVE('',#15262,#15263,#3275,.T.);
#19346=EDGE_CURVE('',#15264,#15263,#3276,.T.);
#19347=EDGE_CURVE('',#15264,#15265,#3277,.T.);
#19348=EDGE_CURVE('',#15265,#15266,#3278,.T.);
#19349=EDGE_CURVE('',#15266,#15267,#3279,.T.);
#19350=EDGE_CURVE('',#15268,#15267,#3280,.T.);
#19351=EDGE_CURVE('',#15268,#15269,#3281,.T.);
#19352=EDGE_CURVE('',#15269,#15270,#3282,.T.);
#19353=EDGE_CURVE('',#15270,#15271,#3283,.T.);
#19354=EDGE_CURVE('',#15272,#15271,#3284,.T.);
#19355=EDGE_CURVE('',#15272,#15273,#3285,.T.);
#19356=EDGE_CURVE('',#15273,#15274,#3286,.T.);
#19357=EDGE_CURVE('',#15274,#15275,#3287,.T.);
#19358=EDGE_CURVE('',#15276,#15275,#3288,.T.);
#19359=EDGE_CURVE('',#15276,#15277,#3289,.T.);
#19360=EDGE_CURVE('',#15277,#15278,#3290,.T.);
#19361=EDGE_CURVE('',#15278,#15279,#3291,.T.);
#19362=EDGE_CURVE('',#15280,#15279,#3292,.T.);
#19363=EDGE_CURVE('',#15280,#15281,#3293,.T.);
#19364=EDGE_CURVE('',#15281,#15282,#3294,.T.);
#19365=EDGE_CURVE('',#15282,#15283,#3295,.T.);
#19366=EDGE_CURVE('',#15284,#15283,#3296,.T.);
#19367=EDGE_CURVE('',#15284,#15285,#3297,.T.);
#19368=EDGE_CURVE('',#15285,#15286,#3298,.T.);
#19369=EDGE_CURVE('',#15286,#15287,#3299,.T.);
#19370=EDGE_CURVE('',#15288,#15287,#3300,.T.);
#19371=EDGE_CURVE('',#15288,#15289,#3301,.T.);
#19372=EDGE_CURVE('',#15289,#15290,#3302,.T.);
#19373=EDGE_CURVE('',#15290,#15291,#3303,.T.);
#19374=EDGE_CURVE('',#15292,#15291,#3304,.T.);
#19375=EDGE_CURVE('',#15292,#15293,#3305,.T.);
#19376=EDGE_CURVE('',#15293,#15294,#3306,.T.);
#19377=EDGE_CURVE('',#15294,#15295,#3307,.T.);
#19378=EDGE_CURVE('',#15296,#15295,#3308,.T.);
#19379=EDGE_CURVE('',#15296,#15297,#3309,.T.);
#19380=EDGE_CURVE('',#15297,#15298,#3310,.T.);
#19381=EDGE_CURVE('',#15298,#15299,#3311,.T.);
#19382=EDGE_CURVE('',#15300,#15299,#3312,.T.);
#19383=EDGE_CURVE('',#15300,#15301,#3313,.T.);
#19384=EDGE_CURVE('',#15301,#15302,#3314,.T.);
#19385=EDGE_CURVE('',#15302,#15303,#3315,.T.);
#19386=EDGE_CURVE('',#15304,#15303,#3316,.T.);
#19387=EDGE_CURVE('',#15304,#15305,#3317,.T.);
#19388=EDGE_CURVE('',#15305,#15306,#3318,.T.);
#19389=EDGE_CURVE('',#15306,#15307,#3319,.T.);
#19390=EDGE_CURVE('',#15308,#15307,#3320,.T.);
#19391=EDGE_CURVE('',#15308,#15309,#3321,.T.);
#19392=EDGE_CURVE('',#15309,#15310,#3322,.T.);
#19393=EDGE_CURVE('',#15310,#15311,#3323,.T.);
#19394=EDGE_CURVE('',#15120,#15311,#3324,.T.);
#19395=EDGE_CURVE('',#15312,#15313,#9830,.T.);
#19396=EDGE_CURVE('',#15117,#15312,#9831,.T.);
#19397=EDGE_CURVE('',#15116,#15313,#9832,.T.);
#19398=EDGE_CURVE('',#15313,#15314,#9833,.T.);
#19399=EDGE_CURVE('',#15314,#15115,#9834,.T.);
#19400=EDGE_CURVE('',#15314,#15315,#3325,.T.);
#19401=EDGE_CURVE('',#15118,#15315,#9835,.T.);
#19402=EDGE_CURVE('',#15315,#15312,#9836,.T.);
#19403=EDGE_CURVE('',#15316,#15121,#9837,.T.);
#19404=EDGE_CURVE('',#15317,#15316,#3326,.T.);
#19405=EDGE_CURVE('',#15317,#15122,#9838,.T.);
#19406=EDGE_CURVE('',#15318,#15317,#3327,.T.);
#19407=EDGE_CURVE('',#15123,#15318,#9839,.T.);
#19408=EDGE_CURVE('',#15319,#15120,#9840,.T.);
#19409=EDGE_CURVE('',#15316,#15319,#3328,.T.);
#19410=EDGE_CURVE('',#15320,#15125,#9841,.T.);
#19411=EDGE_CURVE('',#15321,#15320,#3329,.T.);
#19412=EDGE_CURVE('',#15321,#15126,#9842,.T.);
#19413=EDGE_CURVE('',#15322,#15321,#3330,.T.);
#19414=EDGE_CURVE('',#15127,#15322,#9843,.T.);
#19415=EDGE_CURVE('',#15323,#15124,#9844,.T.);
#19416=EDGE_CURVE('',#15320,#15323,#3331,.T.);
#19417=EDGE_CURVE('',#15324,#15129,#9845,.T.);
#19418=EDGE_CURVE('',#15325,#15324,#3332,.T.);
#19419=EDGE_CURVE('',#15325,#15130,#9846,.T.);
#19420=EDGE_CURVE('',#15326,#15325,#3333,.T.);
#19421=EDGE_CURVE('',#15131,#15326,#9847,.T.);
#19422=EDGE_CURVE('',#15327,#15128,#9848,.T.);
#19423=EDGE_CURVE('',#15324,#15327,#3334,.T.);
#19424=EDGE_CURVE('',#15328,#15133,#9849,.T.);
#19425=EDGE_CURVE('',#15329,#15328,#3335,.T.);
#19426=EDGE_CURVE('',#15329,#15134,#9850,.T.);
#19427=EDGE_CURVE('',#15330,#15329,#3336,.T.);
#19428=EDGE_CURVE('',#15135,#15330,#9851,.T.);
#19429=EDGE_CURVE('',#15331,#15132,#9852,.T.);
#19430=EDGE_CURVE('',#15328,#15331,#3337,.T.);
#19431=EDGE_CURVE('',#15332,#15137,#9853,.T.);
#19432=EDGE_CURVE('',#15333,#15332,#3338,.T.);
#19433=EDGE_CURVE('',#15333,#15138,#9854,.T.);
#19434=EDGE_CURVE('',#15334,#15333,#3339,.T.);
#19435=EDGE_CURVE('',#15139,#15334,#9855,.T.);
#19436=EDGE_CURVE('',#15335,#15136,#9856,.T.);
#19437=EDGE_CURVE('',#15332,#15335,#3340,.T.);
#19438=EDGE_CURVE('',#15336,#15141,#9857,.T.);
#19439=EDGE_CURVE('',#15337,#15336,#3341,.T.);
#19440=EDGE_CURVE('',#15337,#15142,#9858,.T.);
#19441=EDGE_CURVE('',#15338,#15337,#3342,.T.);
#19442=EDGE_CURVE('',#15143,#15338,#9859,.T.);
#19443=EDGE_CURVE('',#15339,#15140,#9860,.T.);
#19444=EDGE_CURVE('',#15336,#15339,#3343,.T.);
#19445=EDGE_CURVE('',#15340,#15145,#9861,.T.);
#19446=EDGE_CURVE('',#15341,#15340,#3344,.T.);
#19447=EDGE_CURVE('',#15341,#15146,#9862,.T.);
#19448=EDGE_CURVE('',#15342,#15341,#3345,.T.);
#19449=EDGE_CURVE('',#15147,#15342,#9863,.T.);
#19450=EDGE_CURVE('',#15343,#15144,#9864,.T.);
#19451=EDGE_CURVE('',#15340,#15343,#3346,.T.);
#19452=EDGE_CURVE('',#15344,#15149,#9865,.T.);
#19453=EDGE_CURVE('',#15345,#15344,#3347,.T.);
#19454=EDGE_CURVE('',#15345,#15150,#9866,.T.);
#19455=EDGE_CURVE('',#15346,#15345,#3348,.T.);
#19456=EDGE_CURVE('',#15151,#15346,#9867,.T.);
#19457=EDGE_CURVE('',#15347,#15148,#9868,.T.);
#19458=EDGE_CURVE('',#15344,#15347,#3349,.T.);
#19459=EDGE_CURVE('',#15348,#15153,#9869,.T.);
#19460=EDGE_CURVE('',#15349,#15348,#3350,.T.);
#19461=EDGE_CURVE('',#15349,#15154,#9870,.T.);
#19462=EDGE_CURVE('',#15350,#15349,#3351,.T.);
#19463=EDGE_CURVE('',#15155,#15350,#9871,.T.);
#19464=EDGE_CURVE('',#15351,#15152,#9872,.T.);
#19465=EDGE_CURVE('',#15348,#15351,#3352,.T.);
#19466=EDGE_CURVE('',#15352,#15157,#9873,.T.);
#19467=EDGE_CURVE('',#15353,#15352,#3353,.T.);
#19468=EDGE_CURVE('',#15353,#15158,#9874,.T.);
#19469=EDGE_CURVE('',#15354,#15353,#3354,.T.);
#19470=EDGE_CURVE('',#15159,#15354,#9875,.T.);
#19471=EDGE_CURVE('',#15355,#15156,#9876,.T.);
#19472=EDGE_CURVE('',#15352,#15355,#3355,.T.);
#19473=EDGE_CURVE('',#15356,#15161,#9877,.T.);
#19474=EDGE_CURVE('',#15357,#15356,#3356,.T.);
#19475=EDGE_CURVE('',#15357,#15162,#9878,.T.);
#19476=EDGE_CURVE('',#15358,#15357,#3357,.T.);
#19477=EDGE_CURVE('',#15163,#15358,#9879,.T.);
#19478=EDGE_CURVE('',#15359,#15160,#9880,.T.);
#19479=EDGE_CURVE('',#15356,#15359,#3358,.T.);
#19480=EDGE_CURVE('',#15360,#15165,#9881,.T.);
#19481=EDGE_CURVE('',#15361,#15360,#3359,.T.);
#19482=EDGE_CURVE('',#15361,#15166,#9882,.T.);
#19483=EDGE_CURVE('',#15362,#15361,#3360,.T.);
#19484=EDGE_CURVE('',#15167,#15362,#9883,.T.);
#19485=EDGE_CURVE('',#15363,#15164,#9884,.T.);
#19486=EDGE_CURVE('',#15360,#15363,#3361,.T.);
#19487=EDGE_CURVE('',#15364,#15169,#9885,.T.);
#19488=EDGE_CURVE('',#15365,#15364,#3362,.T.);
#19489=EDGE_CURVE('',#15365,#15170,#9886,.T.);
#19490=EDGE_CURVE('',#15366,#15365,#3363,.T.);
#19491=EDGE_CURVE('',#15171,#15366,#9887,.T.);
#19492=EDGE_CURVE('',#15367,#15168,#9888,.T.);
#19493=EDGE_CURVE('',#15364,#15367,#3364,.T.);
#19494=EDGE_CURVE('',#15368,#15173,#9889,.T.);
#19495=EDGE_CURVE('',#15369,#15368,#3365,.T.);
#19496=EDGE_CURVE('',#15369,#15174,#9890,.T.);
#19497=EDGE_CURVE('',#15370,#15369,#3366,.T.);
#19498=EDGE_CURVE('',#15175,#15370,#9891,.T.);
#19499=EDGE_CURVE('',#15371,#15172,#9892,.T.);
#19500=EDGE_CURVE('',#15368,#15371,#3367,.T.);
#19501=EDGE_CURVE('',#15372,#15177,#9893,.T.);
#19502=EDGE_CURVE('',#15373,#15372,#3368,.T.);
#19503=EDGE_CURVE('',#15373,#15178,#9894,.T.);
#19504=EDGE_CURVE('',#15374,#15373,#3369,.T.);
#19505=EDGE_CURVE('',#15179,#15374,#9895,.T.);
#19506=EDGE_CURVE('',#15375,#15176,#9896,.T.);
#19507=EDGE_CURVE('',#15372,#15375,#3370,.T.);
#19508=EDGE_CURVE('',#15376,#15181,#9897,.T.);
#19509=EDGE_CURVE('',#15377,#15376,#3371,.T.);
#19510=EDGE_CURVE('',#15377,#15182,#9898,.T.);
#19511=EDGE_CURVE('',#15378,#15377,#3372,.T.);
#19512=EDGE_CURVE('',#15183,#15378,#9899,.T.);
#19513=EDGE_CURVE('',#15379,#15180,#9900,.T.);
#19514=EDGE_CURVE('',#15376,#15379,#3373,.T.);
#19515=EDGE_CURVE('',#15380,#15185,#9901,.T.);
#19516=EDGE_CURVE('',#15381,#15380,#3374,.T.);
#19517=EDGE_CURVE('',#15381,#15186,#9902,.T.);
#19518=EDGE_CURVE('',#15382,#15381,#3375,.T.);
#19519=EDGE_CURVE('',#15187,#15382,#9903,.T.);
#19520=EDGE_CURVE('',#15383,#15184,#9904,.T.);
#19521=EDGE_CURVE('',#15380,#15383,#3376,.T.);
#19522=EDGE_CURVE('',#15384,#15189,#9905,.T.);
#19523=EDGE_CURVE('',#15385,#15384,#3377,.T.);
#19524=EDGE_CURVE('',#15385,#15190,#9906,.T.);
#19525=EDGE_CURVE('',#15386,#15385,#3378,.T.);
#19526=EDGE_CURVE('',#15191,#15386,#9907,.T.);
#19527=EDGE_CURVE('',#15387,#15188,#9908,.T.);
#19528=EDGE_CURVE('',#15384,#15387,#3379,.T.);
#19529=EDGE_CURVE('',#15388,#15193,#9909,.T.);
#19530=EDGE_CURVE('',#15389,#15388,#3380,.T.);
#19531=EDGE_CURVE('',#15389,#15194,#9910,.T.);
#19532=EDGE_CURVE('',#15390,#15389,#3381,.T.);
#19533=EDGE_CURVE('',#15195,#15390,#9911,.T.);
#19534=EDGE_CURVE('',#15391,#15192,#9912,.T.);
#19535=EDGE_CURVE('',#15388,#15391,#3382,.T.);
#19536=EDGE_CURVE('',#15392,#15197,#9913,.T.);
#19537=EDGE_CURVE('',#15393,#15392,#3383,.T.);
#19538=EDGE_CURVE('',#15393,#15198,#9914,.T.);
#19539=EDGE_CURVE('',#15394,#15393,#3384,.T.);
#19540=EDGE_CURVE('',#15199,#15394,#9915,.T.);
#19541=EDGE_CURVE('',#15395,#15196,#9916,.T.);
#19542=EDGE_CURVE('',#15392,#15395,#3385,.T.);
#19543=EDGE_CURVE('',#15396,#15201,#9917,.T.);
#19544=EDGE_CURVE('',#15397,#15396,#3386,.T.);
#19545=EDGE_CURVE('',#15397,#15202,#9918,.T.);
#19546=EDGE_CURVE('',#15398,#15397,#3387,.T.);
#19547=EDGE_CURVE('',#15203,#15398,#9919,.T.);
#19548=EDGE_CURVE('',#15399,#15200,#9920,.T.);
#19549=EDGE_CURVE('',#15396,#15399,#3388,.T.);
#19550=EDGE_CURVE('',#15400,#15205,#9921,.T.);
#19551=EDGE_CURVE('',#15401,#15400,#3389,.T.);
#19552=EDGE_CURVE('',#15401,#15206,#9922,.T.);
#19553=EDGE_CURVE('',#15402,#15401,#3390,.T.);
#19554=EDGE_CURVE('',#15207,#15402,#9923,.T.);
#19555=EDGE_CURVE('',#15403,#15204,#9924,.T.);
#19556=EDGE_CURVE('',#15400,#15403,#3391,.T.);
#19557=EDGE_CURVE('',#15404,#15209,#9925,.T.);
#19558=EDGE_CURVE('',#15405,#15404,#3392,.T.);
#19559=EDGE_CURVE('',#15405,#15210,#9926,.T.);
#19560=EDGE_CURVE('',#15406,#15405,#3393,.T.);
#19561=EDGE_CURVE('',#15211,#15406,#9927,.T.);
#19562=EDGE_CURVE('',#15407,#15208,#9928,.T.);
#19563=EDGE_CURVE('',#15404,#15407,#3394,.T.);
#19564=EDGE_CURVE('',#15408,#15213,#9929,.T.);
#19565=EDGE_CURVE('',#15409,#15408,#3395,.T.);
#19566=EDGE_CURVE('',#15409,#15214,#9930,.T.);
#19567=EDGE_CURVE('',#15410,#15409,#3396,.T.);
#19568=EDGE_CURVE('',#15215,#15410,#9931,.T.);
#19569=EDGE_CURVE('',#15411,#15212,#9932,.T.);
#19570=EDGE_CURVE('',#15408,#15411,#3397,.T.);
#19571=EDGE_CURVE('',#15412,#15217,#9933,.T.);
#19572=EDGE_CURVE('',#15413,#15412,#3398,.T.);
#19573=EDGE_CURVE('',#15413,#15218,#9934,.T.);
#19574=EDGE_CURVE('',#15414,#15413,#3399,.T.);
#19575=EDGE_CURVE('',#15219,#15414,#9935,.T.);
#19576=EDGE_CURVE('',#15415,#15216,#9936,.T.);
#19577=EDGE_CURVE('',#15412,#15415,#3400,.T.);
#19578=EDGE_CURVE('',#15416,#15221,#9937,.T.);
#19579=EDGE_CURVE('',#15417,#15416,#3401,.T.);
#19580=EDGE_CURVE('',#15417,#15222,#9938,.T.);
#19581=EDGE_CURVE('',#15418,#15417,#3402,.T.);
#19582=EDGE_CURVE('',#15223,#15418,#9939,.T.);
#19583=EDGE_CURVE('',#15419,#15220,#9940,.T.);
#19584=EDGE_CURVE('',#15416,#15419,#3403,.T.);
#19585=EDGE_CURVE('',#15420,#15225,#9941,.T.);
#19586=EDGE_CURVE('',#15421,#15420,#3404,.T.);
#19587=EDGE_CURVE('',#15421,#15226,#9942,.T.);
#19588=EDGE_CURVE('',#15422,#15421,#3405,.T.);
#19589=EDGE_CURVE('',#15227,#15422,#9943,.T.);
#19590=EDGE_CURVE('',#15423,#15224,#9944,.T.);
#19591=EDGE_CURVE('',#15420,#15423,#3406,.T.);
#19592=EDGE_CURVE('',#15424,#15229,#9945,.T.);
#19593=EDGE_CURVE('',#15425,#15424,#3407,.T.);
#19594=EDGE_CURVE('',#15425,#15230,#9946,.T.);
#19595=EDGE_CURVE('',#15426,#15425,#3408,.T.);
#19596=EDGE_CURVE('',#15231,#15426,#9947,.T.);
#19597=EDGE_CURVE('',#15427,#15228,#9948,.T.);
#19598=EDGE_CURVE('',#15424,#15427,#3409,.T.);
#19599=EDGE_CURVE('',#15428,#15233,#9949,.T.);
#19600=EDGE_CURVE('',#15429,#15428,#3410,.T.);
#19601=EDGE_CURVE('',#15429,#15234,#9950,.T.);
#19602=EDGE_CURVE('',#15430,#15429,#3411,.T.);
#19603=EDGE_CURVE('',#15235,#15430,#9951,.T.);
#19604=EDGE_CURVE('',#15431,#15232,#9952,.T.);
#19605=EDGE_CURVE('',#15428,#15431,#3412,.T.);
#19606=EDGE_CURVE('',#15432,#15237,#9953,.T.);
#19607=EDGE_CURVE('',#15433,#15432,#3413,.T.);
#19608=EDGE_CURVE('',#15433,#15238,#9954,.T.);
#19609=EDGE_CURVE('',#15434,#15433,#3414,.T.);
#19610=EDGE_CURVE('',#15239,#15434,#9955,.T.);
#19611=EDGE_CURVE('',#15435,#15236,#9956,.T.);
#19612=EDGE_CURVE('',#15432,#15435,#3415,.T.);
#19613=EDGE_CURVE('',#15436,#15241,#9957,.T.);
#19614=EDGE_CURVE('',#15437,#15436,#3416,.T.);
#19615=EDGE_CURVE('',#15437,#15242,#9958,.T.);
#19616=EDGE_CURVE('',#15438,#15437,#3417,.T.);
#19617=EDGE_CURVE('',#15243,#15438,#9959,.T.);
#19618=EDGE_CURVE('',#15439,#15240,#9960,.T.);
#19619=EDGE_CURVE('',#15436,#15439,#3418,.T.);
#19620=EDGE_CURVE('',#15440,#15245,#9961,.T.);
#19621=EDGE_CURVE('',#15441,#15440,#3419,.T.);
#19622=EDGE_CURVE('',#15441,#15246,#9962,.T.);
#19623=EDGE_CURVE('',#15442,#15441,#3420,.T.);
#19624=EDGE_CURVE('',#15247,#15442,#9963,.T.);
#19625=EDGE_CURVE('',#15443,#15244,#9964,.T.);
#19626=EDGE_CURVE('',#15440,#15443,#3421,.T.);
#19627=EDGE_CURVE('',#15444,#15249,#9965,.T.);
#19628=EDGE_CURVE('',#15445,#15444,#3422,.T.);
#19629=EDGE_CURVE('',#15445,#15250,#9966,.T.);
#19630=EDGE_CURVE('',#15446,#15445,#3423,.T.);
#19631=EDGE_CURVE('',#15251,#15446,#9967,.T.);
#19632=EDGE_CURVE('',#15447,#15248,#9968,.T.);
#19633=EDGE_CURVE('',#15444,#15447,#3424,.T.);
#19634=EDGE_CURVE('',#15448,#15253,#9969,.T.);
#19635=EDGE_CURVE('',#15449,#15448,#3425,.T.);
#19636=EDGE_CURVE('',#15449,#15254,#9970,.T.);
#19637=EDGE_CURVE('',#15450,#15449,#3426,.T.);
#19638=EDGE_CURVE('',#15255,#15450,#9971,.T.);
#19639=EDGE_CURVE('',#15451,#15252,#9972,.T.);
#19640=EDGE_CURVE('',#15448,#15451,#3427,.T.);
#19641=EDGE_CURVE('',#15452,#15257,#9973,.T.);
#19642=EDGE_CURVE('',#15453,#15452,#3428,.T.);
#19643=EDGE_CURVE('',#15453,#15258,#9974,.T.);
#19644=EDGE_CURVE('',#15454,#15453,#3429,.T.);
#19645=EDGE_CURVE('',#15259,#15454,#9975,.T.);
#19646=EDGE_CURVE('',#15455,#15256,#9976,.T.);
#19647=EDGE_CURVE('',#15452,#15455,#3430,.T.);
#19648=EDGE_CURVE('',#15456,#15261,#9977,.T.);
#19649=EDGE_CURVE('',#15457,#15456,#3431,.T.);
#19650=EDGE_CURVE('',#15457,#15262,#9978,.T.);
#19651=EDGE_CURVE('',#15458,#15457,#3432,.T.);
#19652=EDGE_CURVE('',#15263,#15458,#9979,.T.);
#19653=EDGE_CURVE('',#15459,#15260,#9980,.T.);
#19654=EDGE_CURVE('',#15456,#15459,#3433,.T.);
#19655=EDGE_CURVE('',#15460,#15265,#9981,.T.);
#19656=EDGE_CURVE('',#15461,#15460,#3434,.T.);
#19657=EDGE_CURVE('',#15461,#15266,#9982,.T.);
#19658=EDGE_CURVE('',#15462,#15461,#3435,.T.);
#19659=EDGE_CURVE('',#15267,#15462,#9983,.T.);
#19660=EDGE_CURVE('',#15463,#15264,#9984,.T.);
#19661=EDGE_CURVE('',#15460,#15463,#3436,.T.);
#19662=EDGE_CURVE('',#15464,#15269,#9985,.T.);
#19663=EDGE_CURVE('',#15465,#15464,#3437,.T.);
#19664=EDGE_CURVE('',#15465,#15270,#9986,.T.);
#19665=EDGE_CURVE('',#15466,#15465,#3438,.T.);
#19666=EDGE_CURVE('',#15271,#15466,#9987,.T.);
#19667=EDGE_CURVE('',#15467,#15268,#9988,.T.);
#19668=EDGE_CURVE('',#15464,#15467,#3439,.T.);
#19669=EDGE_CURVE('',#15468,#15273,#9989,.T.);
#19670=EDGE_CURVE('',#15469,#15468,#3440,.T.);
#19671=EDGE_CURVE('',#15469,#15274,#9990,.T.);
#19672=EDGE_CURVE('',#15470,#15469,#3441,.T.);
#19673=EDGE_CURVE('',#15275,#15470,#9991,.T.);
#19674=EDGE_CURVE('',#15471,#15272,#9992,.T.);
#19675=EDGE_CURVE('',#15468,#15471,#3442,.T.);
#19676=EDGE_CURVE('',#15472,#15277,#9993,.T.);
#19677=EDGE_CURVE('',#15473,#15472,#3443,.T.);
#19678=EDGE_CURVE('',#15473,#15278,#9994,.T.);
#19679=EDGE_CURVE('',#15474,#15473,#3444,.T.);
#19680=EDGE_CURVE('',#15279,#15474,#9995,.T.);
#19681=EDGE_CURVE('',#15475,#15276,#9996,.T.);
#19682=EDGE_CURVE('',#15472,#15475,#3445,.T.);
#19683=EDGE_CURVE('',#15476,#15281,#9997,.T.);
#19684=EDGE_CURVE('',#15477,#15476,#3446,.T.);
#19685=EDGE_CURVE('',#15477,#15282,#9998,.T.);
#19686=EDGE_CURVE('',#15478,#15477,#3447,.T.);
#19687=EDGE_CURVE('',#15283,#15478,#9999,.T.);
#19688=EDGE_CURVE('',#15479,#15280,#10000,.T.);
#19689=EDGE_CURVE('',#15476,#15479,#3448,.T.);
#19690=EDGE_CURVE('',#15480,#15285,#10001,.T.);
#19691=EDGE_CURVE('',#15481,#15480,#3449,.T.);
#19692=EDGE_CURVE('',#15481,#15286,#10002,.T.);
#19693=EDGE_CURVE('',#15482,#15481,#3450,.T.);
#19694=EDGE_CURVE('',#15287,#15482,#10003,.T.);
#19695=EDGE_CURVE('',#15483,#15284,#10004,.T.);
#19696=EDGE_CURVE('',#15480,#15483,#3451,.T.);
#19697=EDGE_CURVE('',#15484,#15289,#10005,.T.);
#19698=EDGE_CURVE('',#15485,#15484,#3452,.T.);
#19699=EDGE_CURVE('',#15485,#15290,#10006,.T.);
#19700=EDGE_CURVE('',#15486,#15485,#3453,.T.);
#19701=EDGE_CURVE('',#15291,#15486,#10007,.T.);
#19702=EDGE_CURVE('',#15487,#15288,#10008,.T.);
#19703=EDGE_CURVE('',#15484,#15487,#3454,.T.);
#19704=EDGE_CURVE('',#15488,#15293,#10009,.T.);
#19705=EDGE_CURVE('',#15489,#15488,#3455,.T.);
#19706=EDGE_CURVE('',#15489,#15294,#10010,.T.);
#19707=EDGE_CURVE('',#15490,#15489,#3456,.T.);
#19708=EDGE_CURVE('',#15295,#15490,#10011,.T.);
#19709=EDGE_CURVE('',#15491,#15292,#10012,.T.);
#19710=EDGE_CURVE('',#15488,#15491,#3457,.T.);
#19711=EDGE_CURVE('',#15492,#15297,#10013,.T.);
#19712=EDGE_CURVE('',#15493,#15492,#3458,.T.);
#19713=EDGE_CURVE('',#15493,#15298,#10014,.T.);
#19714=EDGE_CURVE('',#15494,#15493,#3459,.T.);
#19715=EDGE_CURVE('',#15299,#15494,#10015,.T.);
#19716=EDGE_CURVE('',#15495,#15296,#10016,.T.);
#19717=EDGE_CURVE('',#15492,#15495,#3460,.T.);
#19718=EDGE_CURVE('',#15496,#15301,#10017,.T.);
#19719=EDGE_CURVE('',#15497,#15496,#3461,.T.);
#19720=EDGE_CURVE('',#15497,#15302,#10018,.T.);
#19721=EDGE_CURVE('',#15498,#15497,#3462,.T.);
#19722=EDGE_CURVE('',#15303,#15498,#10019,.T.);
#19723=EDGE_CURVE('',#15499,#15300,#10020,.T.);
#19724=EDGE_CURVE('',#15496,#15499,#3463,.T.);
#19725=EDGE_CURVE('',#15500,#15305,#10021,.T.);
#19726=EDGE_CURVE('',#15501,#15500,#3464,.T.);
#19727=EDGE_CURVE('',#15501,#15306,#10022,.T.);
#19728=EDGE_CURVE('',#15502,#15501,#3465,.T.);
#19729=EDGE_CURVE('',#15307,#15502,#10023,.T.);
#19730=EDGE_CURVE('',#15503,#15304,#10024,.T.);
#19731=EDGE_CURVE('',#15500,#15503,#3466,.T.);
#19732=EDGE_CURVE('',#15504,#15502,#3467,.T.);
#19733=EDGE_CURVE('',#15504,#15308,#10025,.T.);
#19734=EDGE_CURVE('',#15503,#15498,#3468,.T.);
#19735=EDGE_CURVE('',#15499,#15494,#3469,.T.);
#19736=EDGE_CURVE('',#15495,#15490,#3470,.T.);
#19737=EDGE_CURVE('',#15491,#15486,#3471,.T.);
#19738=EDGE_CURVE('',#15487,#15482,#3472,.T.);
#19739=EDGE_CURVE('',#15483,#15478,#3473,.T.);
#19740=EDGE_CURVE('',#15479,#15474,#3474,.T.);
#19741=EDGE_CURVE('',#15475,#15470,#3475,.T.);
#19742=EDGE_CURVE('',#15471,#15466,#3476,.T.);
#19743=EDGE_CURVE('',#15467,#15462,#3477,.T.);
#19744=EDGE_CURVE('',#15463,#15458,#3478,.T.);
#19745=EDGE_CURVE('',#15459,#15454,#3479,.T.);
#19746=EDGE_CURVE('',#15455,#15450,#3480,.T.);
#19747=EDGE_CURVE('',#15451,#15446,#3481,.T.);
#19748=EDGE_CURVE('',#15447,#15442,#3482,.T.);
#19749=EDGE_CURVE('',#15443,#15438,#3483,.T.);
#19750=EDGE_CURVE('',#15439,#15434,#3484,.T.);
#19751=EDGE_CURVE('',#15435,#15430,#3485,.T.);
#19752=EDGE_CURVE('',#15431,#15426,#3486,.T.);
#19753=EDGE_CURVE('',#15427,#15422,#3487,.T.);
#19754=EDGE_CURVE('',#15423,#15418,#3488,.T.);
#19755=EDGE_CURVE('',#15419,#15414,#3489,.T.);
#19756=EDGE_CURVE('',#15415,#15410,#3490,.T.);
#19757=EDGE_CURVE('',#15411,#15406,#3491,.T.);
#19758=EDGE_CURVE('',#15407,#15402,#3492,.T.);
#19759=EDGE_CURVE('',#15403,#15398,#3493,.T.);
#19760=EDGE_CURVE('',#15399,#15394,#3494,.T.);
#19761=EDGE_CURVE('',#15395,#15390,#3495,.T.);
#19762=EDGE_CURVE('',#15391,#15386,#3496,.T.);
#19763=EDGE_CURVE('',#15387,#15382,#3497,.T.);
#19764=EDGE_CURVE('',#15383,#15378,#3498,.T.);
#19765=EDGE_CURVE('',#15379,#15374,#3499,.T.);
#19766=EDGE_CURVE('',#15375,#15370,#3500,.T.);
#19767=EDGE_CURVE('',#15371,#15366,#3501,.T.);
#19768=EDGE_CURVE('',#15367,#15362,#3502,.T.);
#19769=EDGE_CURVE('',#15363,#15358,#3503,.T.);
#19770=EDGE_CURVE('',#15359,#15354,#3504,.T.);
#19771=EDGE_CURVE('',#15355,#15350,#3505,.T.);
#19772=EDGE_CURVE('',#15351,#15346,#3506,.T.);
#19773=EDGE_CURVE('',#15347,#15342,#3507,.T.);
#19774=EDGE_CURVE('',#15343,#15338,#3508,.T.);
#19775=EDGE_CURVE('',#15339,#15334,#3509,.T.);
#19776=EDGE_CURVE('',#15335,#15330,#3510,.T.);
#19777=EDGE_CURVE('',#15331,#15326,#3511,.T.);
#19778=EDGE_CURVE('',#15327,#15322,#3512,.T.);
#19779=EDGE_CURVE('',#15323,#15318,#3513,.T.);
#19780=EDGE_CURVE('',#15505,#15309,#10026,.T.);
#19781=EDGE_CURVE('',#15506,#15505,#3514,.T.);
#19782=EDGE_CURVE('',#15506,#15310,#10027,.T.);
#19783=EDGE_CURVE('',#15507,#15506,#3515,.T.);
#19784=EDGE_CURVE('',#15311,#15507,#10028,.T.);
#19785=EDGE_CURVE('',#15505,#15504,#3516,.T.);
#19786=EDGE_CURVE('',#15319,#15507,#3517,.T.);
#19787=EDGE_CURVE('',#15508,#15508,#3518,.T.);
#19788=EDGE_CURVE('',#15508,#15509,#3519,.T.);
#19789=EDGE_CURVE('',#15509,#15510,#3520,.T.);
#19790=EDGE_CURVE('',#15510,#15509,#3521,.T.);
#19791=EDGE_CURVE('',#15510,#15511,#10029,.T.);
#19792=EDGE_CURVE('',#15511,#15511,#3522,.T.);
#19793=EDGE_CURVE('',#15512,#15513,#10030,.T.);
#19794=EDGE_CURVE('',#15513,#15514,#10031,.T.);
#19795=EDGE_CURVE('',#15514,#15515,#10032,.T.);
#19796=EDGE_CURVE('',#15515,#15512,#3523,.T.);
#19797=EDGE_CURVE('',#15516,#15516,#3524,.T.);
#19798=EDGE_CURVE('',#15516,#15511,#3525,.T.);
#19799=EDGE_CURVE('',#15517,#15518,#3526,.T.);
#19800=EDGE_CURVE('',#15518,#15519,#3527,.T.);
#19801=EDGE_CURVE('',#15519,#15520,#3528,.T.);
#19802=EDGE_CURVE('',#15521,#15520,#3529,.T.);
#19803=EDGE_CURVE('',#15521,#15522,#3530,.T.);
#19804=EDGE_CURVE('',#15522,#15523,#3531,.T.);
#19805=EDGE_CURVE('',#15523,#15524,#3532,.T.);
#19806=EDGE_CURVE('',#15525,#15524,#3533,.T.);
#19807=EDGE_CURVE('',#15525,#15526,#3534,.T.);
#19808=EDGE_CURVE('',#15526,#15527,#3535,.T.);
#19809=EDGE_CURVE('',#15527,#15528,#3536,.T.);
#19810=EDGE_CURVE('',#15529,#15528,#3537,.T.);
#19811=EDGE_CURVE('',#15529,#15530,#3538,.T.);
#19812=EDGE_CURVE('',#15530,#15531,#3539,.T.);
#19813=EDGE_CURVE('',#15531,#15532,#3540,.T.);
#19814=EDGE_CURVE('',#15533,#15532,#3541,.T.);
#19815=EDGE_CURVE('',#15533,#15534,#3542,.T.);
#19816=EDGE_CURVE('',#15534,#15535,#3543,.T.);
#19817=EDGE_CURVE('',#15535,#15536,#3544,.T.);
#19818=EDGE_CURVE('',#15537,#15536,#3545,.T.);
#19819=EDGE_CURVE('',#15537,#15538,#3546,.T.);
#19820=EDGE_CURVE('',#15538,#15539,#3547,.T.);
#19821=EDGE_CURVE('',#15539,#15540,#3548,.T.);
#19822=EDGE_CURVE('',#15541,#15540,#3549,.T.);
#19823=EDGE_CURVE('',#15541,#15542,#3550,.T.);
#19824=EDGE_CURVE('',#15542,#15543,#3551,.T.);
#19825=EDGE_CURVE('',#15543,#15544,#3552,.T.);
#19826=EDGE_CURVE('',#15545,#15544,#3553,.T.);
#19827=EDGE_CURVE('',#15545,#15546,#3554,.T.);
#19828=EDGE_CURVE('',#15546,#15547,#3555,.T.);
#19829=EDGE_CURVE('',#15547,#15548,#3556,.T.);
#19830=EDGE_CURVE('',#15549,#15548,#3557,.T.);
#19831=EDGE_CURVE('',#15549,#15550,#3558,.T.);
#19832=EDGE_CURVE('',#15550,#15551,#3559,.T.);
#19833=EDGE_CURVE('',#15551,#15552,#3560,.T.);
#19834=EDGE_CURVE('',#15553,#15552,#3561,.T.);
#19835=EDGE_CURVE('',#15553,#15554,#3562,.T.);
#19836=EDGE_CURVE('',#15554,#15555,#3563,.T.);
#19837=EDGE_CURVE('',#15555,#15556,#3564,.T.);
#19838=EDGE_CURVE('',#15557,#15556,#3565,.T.);
#19839=EDGE_CURVE('',#15557,#15558,#3566,.T.);
#19840=EDGE_CURVE('',#15558,#15559,#3567,.T.);
#19841=EDGE_CURVE('',#15559,#15560,#3568,.T.);
#19842=EDGE_CURVE('',#15561,#15560,#3569,.T.);
#19843=EDGE_CURVE('',#15561,#15562,#3570,.T.);
#19844=EDGE_CURVE('',#15562,#15563,#3571,.T.);
#19845=EDGE_CURVE('',#15563,#15564,#3572,.T.);
#19846=EDGE_CURVE('',#15565,#15564,#3573,.T.);
#19847=EDGE_CURVE('',#15565,#15566,#3574,.T.);
#19848=EDGE_CURVE('',#15566,#15567,#3575,.T.);
#19849=EDGE_CURVE('',#15567,#15568,#3576,.T.);
#19850=EDGE_CURVE('',#15569,#15568,#3577,.T.);
#19851=EDGE_CURVE('',#15569,#15570,#3578,.T.);
#19852=EDGE_CURVE('',#15570,#15571,#3579,.T.);
#19853=EDGE_CURVE('',#15571,#15572,#3580,.T.);
#19854=EDGE_CURVE('',#15573,#15572,#3581,.T.);
#19855=EDGE_CURVE('',#15573,#15574,#3582,.T.);
#19856=EDGE_CURVE('',#15574,#15575,#3583,.T.);
#19857=EDGE_CURVE('',#15575,#15576,#3584,.T.);
#19858=EDGE_CURVE('',#15577,#15576,#3585,.T.);
#19859=EDGE_CURVE('',#15577,#15578,#3586,.T.);
#19860=EDGE_CURVE('',#15578,#15579,#3587,.T.);
#19861=EDGE_CURVE('',#15579,#15580,#3588,.T.);
#19862=EDGE_CURVE('',#15581,#15580,#3589,.T.);
#19863=EDGE_CURVE('',#15581,#15582,#3590,.T.);
#19864=EDGE_CURVE('',#15582,#15583,#3591,.T.);
#19865=EDGE_CURVE('',#15583,#15584,#3592,.T.);
#19866=EDGE_CURVE('',#15585,#15584,#3593,.T.);
#19867=EDGE_CURVE('',#15585,#15586,#3594,.T.);
#19868=EDGE_CURVE('',#15586,#15587,#3595,.T.);
#19869=EDGE_CURVE('',#15587,#15588,#3596,.T.);
#19870=EDGE_CURVE('',#15589,#15588,#3597,.T.);
#19871=EDGE_CURVE('',#15589,#15590,#3598,.T.);
#19872=EDGE_CURVE('',#15590,#15591,#3599,.T.);
#19873=EDGE_CURVE('',#15591,#15592,#3600,.T.);
#19874=EDGE_CURVE('',#15593,#15592,#3601,.T.);
#19875=EDGE_CURVE('',#15593,#15594,#3602,.T.);
#19876=EDGE_CURVE('',#15594,#15595,#3603,.T.);
#19877=EDGE_CURVE('',#15595,#15596,#3604,.T.);
#19878=EDGE_CURVE('',#15597,#15596,#3605,.T.);
#19879=EDGE_CURVE('',#15597,#15598,#3606,.T.);
#19880=EDGE_CURVE('',#15598,#15599,#3607,.T.);
#19881=EDGE_CURVE('',#15599,#15600,#3608,.T.);
#19882=EDGE_CURVE('',#15601,#15600,#3609,.T.);
#19883=EDGE_CURVE('',#15601,#15602,#3610,.T.);
#19884=EDGE_CURVE('',#15602,#15603,#3611,.T.);
#19885=EDGE_CURVE('',#15603,#15604,#3612,.T.);
#19886=EDGE_CURVE('',#15605,#15604,#3613,.T.);
#19887=EDGE_CURVE('',#15605,#15606,#3614,.T.);
#19888=EDGE_CURVE('',#15606,#15607,#3615,.T.);
#19889=EDGE_CURVE('',#15607,#15608,#3616,.T.);
#19890=EDGE_CURVE('',#15609,#15608,#3617,.T.);
#19891=EDGE_CURVE('',#15609,#15610,#3618,.T.);
#19892=EDGE_CURVE('',#15610,#15611,#3619,.T.);
#19893=EDGE_CURVE('',#15611,#15612,#3620,.T.);
#19894=EDGE_CURVE('',#15613,#15612,#3621,.T.);
#19895=EDGE_CURVE('',#15613,#15614,#3622,.T.);
#19896=EDGE_CURVE('',#15614,#15615,#3623,.T.);
#19897=EDGE_CURVE('',#15615,#15616,#3624,.T.);
#19898=EDGE_CURVE('',#15617,#15616,#3625,.T.);
#19899=EDGE_CURVE('',#15617,#15618,#3626,.T.);
#19900=EDGE_CURVE('',#15618,#15619,#3627,.T.);
#19901=EDGE_CURVE('',#15619,#15620,#3628,.T.);
#19902=EDGE_CURVE('',#15621,#15620,#3629,.T.);
#19903=EDGE_CURVE('',#15621,#15622,#3630,.T.);
#19904=EDGE_CURVE('',#15622,#15623,#3631,.T.);
#19905=EDGE_CURVE('',#15623,#15624,#3632,.T.);
#19906=EDGE_CURVE('',#15625,#15624,#3633,.T.);
#19907=EDGE_CURVE('',#15625,#15626,#3634,.T.);
#19908=EDGE_CURVE('',#15626,#15627,#3635,.T.);
#19909=EDGE_CURVE('',#15627,#15628,#3636,.T.);
#19910=EDGE_CURVE('',#15629,#15628,#3637,.T.);
#19911=EDGE_CURVE('',#15629,#15630,#3638,.T.);
#19912=EDGE_CURVE('',#15630,#15631,#3639,.T.);
#19913=EDGE_CURVE('',#15631,#15632,#3640,.T.);
#19914=EDGE_CURVE('',#15633,#15632,#3641,.T.);
#19915=EDGE_CURVE('',#15633,#15634,#3642,.T.);
#19916=EDGE_CURVE('',#15634,#15635,#3643,.T.);
#19917=EDGE_CURVE('',#15635,#15636,#3644,.T.);
#19918=EDGE_CURVE('',#15637,#15636,#3645,.T.);
#19919=EDGE_CURVE('',#15637,#15638,#3646,.T.);
#19920=EDGE_CURVE('',#15638,#15639,#3647,.T.);
#19921=EDGE_CURVE('',#15639,#15640,#3648,.T.);
#19922=EDGE_CURVE('',#15641,#15640,#3649,.T.);
#19923=EDGE_CURVE('',#15641,#15642,#3650,.T.);
#19924=EDGE_CURVE('',#15642,#15643,#3651,.T.);
#19925=EDGE_CURVE('',#15643,#15644,#3652,.T.);
#19926=EDGE_CURVE('',#15645,#15644,#3653,.T.);
#19927=EDGE_CURVE('',#15645,#15646,#3654,.T.);
#19928=EDGE_CURVE('',#15646,#15647,#3655,.T.);
#19929=EDGE_CURVE('',#15647,#15648,#3656,.T.);
#19930=EDGE_CURVE('',#15649,#15648,#3657,.T.);
#19931=EDGE_CURVE('',#15649,#15650,#3658,.T.);
#19932=EDGE_CURVE('',#15650,#15651,#3659,.T.);
#19933=EDGE_CURVE('',#15651,#15652,#3660,.T.);
#19934=EDGE_CURVE('',#15653,#15652,#3661,.T.);
#19935=EDGE_CURVE('',#15653,#15654,#3662,.T.);
#19936=EDGE_CURVE('',#15654,#15655,#3663,.T.);
#19937=EDGE_CURVE('',#15655,#15656,#3664,.T.);
#19938=EDGE_CURVE('',#15657,#15656,#3665,.T.);
#19939=EDGE_CURVE('',#15657,#15658,#3666,.T.);
#19940=EDGE_CURVE('',#15658,#15659,#3667,.T.);
#19941=EDGE_CURVE('',#15659,#15660,#3668,.T.);
#19942=EDGE_CURVE('',#15661,#15660,#3669,.T.);
#19943=EDGE_CURVE('',#15661,#15662,#3670,.T.);
#19944=EDGE_CURVE('',#15662,#15663,#3671,.T.);
#19945=EDGE_CURVE('',#15663,#15664,#3672,.T.);
#19946=EDGE_CURVE('',#15665,#15664,#3673,.T.);
#19947=EDGE_CURVE('',#15665,#15666,#3674,.T.);
#19948=EDGE_CURVE('',#15666,#15667,#3675,.T.);
#19949=EDGE_CURVE('',#15667,#15668,#3676,.T.);
#19950=EDGE_CURVE('',#15669,#15668,#3677,.T.);
#19951=EDGE_CURVE('',#15669,#15670,#3678,.T.);
#19952=EDGE_CURVE('',#15670,#15671,#3679,.T.);
#19953=EDGE_CURVE('',#15671,#15672,#3680,.T.);
#19954=EDGE_CURVE('',#15673,#15672,#3681,.T.);
#19955=EDGE_CURVE('',#15673,#15674,#3682,.T.);
#19956=EDGE_CURVE('',#15674,#15675,#3683,.T.);
#19957=EDGE_CURVE('',#15675,#15676,#3684,.T.);
#19958=EDGE_CURVE('',#15517,#15676,#3685,.T.);
#19959=EDGE_CURVE('',#15677,#15678,#10033,.T.);
#19960=EDGE_CURVE('',#15514,#15677,#10034,.T.);
#19961=EDGE_CURVE('',#15513,#15678,#10035,.T.);
#19962=EDGE_CURVE('',#15678,#15679,#10036,.T.);
#19963=EDGE_CURVE('',#15679,#15512,#10037,.T.);
#19964=EDGE_CURVE('',#15679,#15680,#3686,.T.);
#19965=EDGE_CURVE('',#15515,#15680,#10038,.T.);
#19966=EDGE_CURVE('',#15680,#15677,#10039,.T.);
#19967=EDGE_CURVE('',#15681,#15518,#10040,.T.);
#19968=EDGE_CURVE('',#15682,#15681,#3687,.T.);
#19969=EDGE_CURVE('',#15682,#15519,#10041,.T.);
#19970=EDGE_CURVE('',#15683,#15682,#3688,.T.);
#19971=EDGE_CURVE('',#15520,#15683,#10042,.T.);
#19972=EDGE_CURVE('',#15684,#15517,#10043,.T.);
#19973=EDGE_CURVE('',#15681,#15684,#3689,.T.);
#19974=EDGE_CURVE('',#15685,#15522,#10044,.T.);
#19975=EDGE_CURVE('',#15686,#15685,#3690,.T.);
#19976=EDGE_CURVE('',#15686,#15523,#10045,.T.);
#19977=EDGE_CURVE('',#15687,#15686,#3691,.T.);
#19978=EDGE_CURVE('',#15524,#15687,#10046,.T.);
#19979=EDGE_CURVE('',#15688,#15521,#10047,.T.);
#19980=EDGE_CURVE('',#15685,#15688,#3692,.T.);
#19981=EDGE_CURVE('',#15689,#15526,#10048,.T.);
#19982=EDGE_CURVE('',#15690,#15689,#3693,.T.);
#19983=EDGE_CURVE('',#15690,#15527,#10049,.T.);
#19984=EDGE_CURVE('',#15691,#15690,#3694,.T.);
#19985=EDGE_CURVE('',#15528,#15691,#10050,.T.);
#19986=EDGE_CURVE('',#15692,#15525,#10051,.T.);
#19987=EDGE_CURVE('',#15689,#15692,#3695,.T.);
#19988=EDGE_CURVE('',#15693,#15530,#10052,.T.);
#19989=EDGE_CURVE('',#15694,#15693,#3696,.T.);
#19990=EDGE_CURVE('',#15694,#15531,#10053,.T.);
#19991=EDGE_CURVE('',#15695,#15694,#3697,.T.);
#19992=EDGE_CURVE('',#15532,#15695,#10054,.T.);
#19993=EDGE_CURVE('',#15696,#15529,#10055,.T.);
#19994=EDGE_CURVE('',#15693,#15696,#3698,.T.);
#19995=EDGE_CURVE('',#15697,#15534,#10056,.T.);
#19996=EDGE_CURVE('',#15698,#15697,#3699,.T.);
#19997=EDGE_CURVE('',#15698,#15535,#10057,.T.);
#19998=EDGE_CURVE('',#15699,#15698,#3700,.T.);
#19999=EDGE_CURVE('',#15536,#15699,#10058,.T.);
#20000=EDGE_CURVE('',#15700,#15533,#10059,.T.);
#20001=EDGE_CURVE('',#15697,#15700,#3701,.T.);
#20002=EDGE_CURVE('',#15701,#15538,#10060,.T.);
#20003=EDGE_CURVE('',#15702,#15701,#3702,.T.);
#20004=EDGE_CURVE('',#15702,#15539,#10061,.T.);
#20005=EDGE_CURVE('',#15703,#15702,#3703,.T.);
#20006=EDGE_CURVE('',#15540,#15703,#10062,.T.);
#20007=EDGE_CURVE('',#15704,#15537,#10063,.T.);
#20008=EDGE_CURVE('',#15701,#15704,#3704,.T.);
#20009=EDGE_CURVE('',#15705,#15542,#10064,.T.);
#20010=EDGE_CURVE('',#15706,#15705,#3705,.T.);
#20011=EDGE_CURVE('',#15706,#15543,#10065,.T.);
#20012=EDGE_CURVE('',#15707,#15706,#3706,.T.);
#20013=EDGE_CURVE('',#15544,#15707,#10066,.T.);
#20014=EDGE_CURVE('',#15708,#15541,#10067,.T.);
#20015=EDGE_CURVE('',#15705,#15708,#3707,.T.);
#20016=EDGE_CURVE('',#15709,#15546,#10068,.T.);
#20017=EDGE_CURVE('',#15710,#15709,#3708,.T.);
#20018=EDGE_CURVE('',#15710,#15547,#10069,.T.);
#20019=EDGE_CURVE('',#15711,#15710,#3709,.T.);
#20020=EDGE_CURVE('',#15548,#15711,#10070,.T.);
#20021=EDGE_CURVE('',#15712,#15545,#10071,.T.);
#20022=EDGE_CURVE('',#15709,#15712,#3710,.T.);
#20023=EDGE_CURVE('',#15713,#15550,#10072,.T.);
#20024=EDGE_CURVE('',#15714,#15713,#3711,.T.);
#20025=EDGE_CURVE('',#15714,#15551,#10073,.T.);
#20026=EDGE_CURVE('',#15715,#15714,#3712,.T.);
#20027=EDGE_CURVE('',#15552,#15715,#10074,.T.);
#20028=EDGE_CURVE('',#15716,#15549,#10075,.T.);
#20029=EDGE_CURVE('',#15713,#15716,#3713,.T.);
#20030=EDGE_CURVE('',#15717,#15554,#10076,.T.);
#20031=EDGE_CURVE('',#15718,#15717,#3714,.T.);
#20032=EDGE_CURVE('',#15718,#15555,#10077,.T.);
#20033=EDGE_CURVE('',#15719,#15718,#3715,.T.);
#20034=EDGE_CURVE('',#15556,#15719,#10078,.T.);
#20035=EDGE_CURVE('',#15720,#15553,#10079,.T.);
#20036=EDGE_CURVE('',#15717,#15720,#3716,.T.);
#20037=EDGE_CURVE('',#15721,#15558,#10080,.T.);
#20038=EDGE_CURVE('',#15722,#15721,#3717,.T.);
#20039=EDGE_CURVE('',#15722,#15559,#10081,.T.);
#20040=EDGE_CURVE('',#15723,#15722,#3718,.T.);
#20041=EDGE_CURVE('',#15560,#15723,#10082,.T.);
#20042=EDGE_CURVE('',#15724,#15557,#10083,.T.);
#20043=EDGE_CURVE('',#15721,#15724,#3719,.T.);
#20044=EDGE_CURVE('',#15725,#15562,#10084,.T.);
#20045=EDGE_CURVE('',#15726,#15725,#3720,.T.);
#20046=EDGE_CURVE('',#15726,#15563,#10085,.T.);
#20047=EDGE_CURVE('',#15727,#15726,#3721,.T.);
#20048=EDGE_CURVE('',#15564,#15727,#10086,.T.);
#20049=EDGE_CURVE('',#15728,#15561,#10087,.T.);
#20050=EDGE_CURVE('',#15725,#15728,#3722,.T.);
#20051=EDGE_CURVE('',#15729,#15566,#10088,.T.);
#20052=EDGE_CURVE('',#15730,#15729,#3723,.T.);
#20053=EDGE_CURVE('',#15730,#15567,#10089,.T.);
#20054=EDGE_CURVE('',#15731,#15730,#3724,.T.);
#20055=EDGE_CURVE('',#15568,#15731,#10090,.T.);
#20056=EDGE_CURVE('',#15732,#15565,#10091,.T.);
#20057=EDGE_CURVE('',#15729,#15732,#3725,.T.);
#20058=EDGE_CURVE('',#15733,#15570,#10092,.T.);
#20059=EDGE_CURVE('',#15734,#15733,#3726,.T.);
#20060=EDGE_CURVE('',#15734,#15571,#10093,.T.);
#20061=EDGE_CURVE('',#15735,#15734,#3727,.T.);
#20062=EDGE_CURVE('',#15572,#15735,#10094,.T.);
#20063=EDGE_CURVE('',#15736,#15569,#10095,.T.);
#20064=EDGE_CURVE('',#15733,#15736,#3728,.T.);
#20065=EDGE_CURVE('',#15737,#15574,#10096,.T.);
#20066=EDGE_CURVE('',#15738,#15737,#3729,.T.);
#20067=EDGE_CURVE('',#15738,#15575,#10097,.T.);
#20068=EDGE_CURVE('',#15739,#15738,#3730,.T.);
#20069=EDGE_CURVE('',#15576,#15739,#10098,.T.);
#20070=EDGE_CURVE('',#15740,#15573,#10099,.T.);
#20071=EDGE_CURVE('',#15737,#15740,#3731,.T.);
#20072=EDGE_CURVE('',#15741,#15578,#10100,.T.);
#20073=EDGE_CURVE('',#15742,#15741,#3732,.T.);
#20074=EDGE_CURVE('',#15742,#15579,#10101,.T.);
#20075=EDGE_CURVE('',#15743,#15742,#3733,.T.);
#20076=EDGE_CURVE('',#15580,#15743,#10102,.T.);
#20077=EDGE_CURVE('',#15744,#15577,#10103,.T.);
#20078=EDGE_CURVE('',#15741,#15744,#3734,.T.);
#20079=EDGE_CURVE('',#15745,#15582,#10104,.T.);
#20080=EDGE_CURVE('',#15746,#15745,#3735,.T.);
#20081=EDGE_CURVE('',#15746,#15583,#10105,.T.);
#20082=EDGE_CURVE('',#15747,#15746,#3736,.T.);
#20083=EDGE_CURVE('',#15584,#15747,#10106,.T.);
#20084=EDGE_CURVE('',#15748,#15581,#10107,.T.);
#20085=EDGE_CURVE('',#15745,#15748,#3737,.T.);
#20086=EDGE_CURVE('',#15749,#15586,#10108,.T.);
#20087=EDGE_CURVE('',#15750,#15749,#3738,.T.);
#20088=EDGE_CURVE('',#15750,#15587,#10109,.T.);
#20089=EDGE_CURVE('',#15751,#15750,#3739,.T.);
#20090=EDGE_CURVE('',#15588,#15751,#10110,.T.);
#20091=EDGE_CURVE('',#15752,#15585,#10111,.T.);
#20092=EDGE_CURVE('',#15749,#15752,#3740,.T.);
#20093=EDGE_CURVE('',#15753,#15590,#10112,.T.);
#20094=EDGE_CURVE('',#15754,#15753,#3741,.T.);
#20095=EDGE_CURVE('',#15754,#15591,#10113,.T.);
#20096=EDGE_CURVE('',#15755,#15754,#3742,.T.);
#20097=EDGE_CURVE('',#15592,#15755,#10114,.T.);
#20098=EDGE_CURVE('',#15756,#15589,#10115,.T.);
#20099=EDGE_CURVE('',#15753,#15756,#3743,.T.);
#20100=EDGE_CURVE('',#15757,#15594,#10116,.T.);
#20101=EDGE_CURVE('',#15758,#15757,#3744,.T.);
#20102=EDGE_CURVE('',#15758,#15595,#10117,.T.);
#20103=EDGE_CURVE('',#15759,#15758,#3745,.T.);
#20104=EDGE_CURVE('',#15596,#15759,#10118,.T.);
#20105=EDGE_CURVE('',#15760,#15593,#10119,.T.);
#20106=EDGE_CURVE('',#15757,#15760,#3746,.T.);
#20107=EDGE_CURVE('',#15761,#15598,#10120,.T.);
#20108=EDGE_CURVE('',#15762,#15761,#3747,.T.);
#20109=EDGE_CURVE('',#15762,#15599,#10121,.T.);
#20110=EDGE_CURVE('',#15763,#15762,#3748,.T.);
#20111=EDGE_CURVE('',#15600,#15763,#10122,.T.);
#20112=EDGE_CURVE('',#15764,#15597,#10123,.T.);
#20113=EDGE_CURVE('',#15761,#15764,#3749,.T.);
#20114=EDGE_CURVE('',#15765,#15602,#10124,.T.);
#20115=EDGE_CURVE('',#15766,#15765,#3750,.T.);
#20116=EDGE_CURVE('',#15766,#15603,#10125,.T.);
#20117=EDGE_CURVE('',#15767,#15766,#3751,.T.);
#20118=EDGE_CURVE('',#15604,#15767,#10126,.T.);
#20119=EDGE_CURVE('',#15768,#15601,#10127,.T.);
#20120=EDGE_CURVE('',#15765,#15768,#3752,.T.);
#20121=EDGE_CURVE('',#15769,#15606,#10128,.T.);
#20122=EDGE_CURVE('',#15770,#15769,#3753,.T.);
#20123=EDGE_CURVE('',#15770,#15607,#10129,.T.);
#20124=EDGE_CURVE('',#15771,#15770,#3754,.T.);
#20125=EDGE_CURVE('',#15608,#15771,#10130,.T.);
#20126=EDGE_CURVE('',#15772,#15605,#10131,.T.);
#20127=EDGE_CURVE('',#15769,#15772,#3755,.T.);
#20128=EDGE_CURVE('',#15773,#15610,#10132,.T.);
#20129=EDGE_CURVE('',#15774,#15773,#3756,.T.);
#20130=EDGE_CURVE('',#15774,#15611,#10133,.T.);
#20131=EDGE_CURVE('',#15775,#15774,#3757,.T.);
#20132=EDGE_CURVE('',#15612,#15775,#10134,.T.);
#20133=EDGE_CURVE('',#15776,#15609,#10135,.T.);
#20134=EDGE_CURVE('',#15773,#15776,#3758,.T.);
#20135=EDGE_CURVE('',#15777,#15614,#10136,.T.);
#20136=EDGE_CURVE('',#15778,#15777,#3759,.T.);
#20137=EDGE_CURVE('',#15778,#15615,#10137,.T.);
#20138=EDGE_CURVE('',#15779,#15778,#3760,.T.);
#20139=EDGE_CURVE('',#15616,#15779,#10138,.T.);
#20140=EDGE_CURVE('',#15780,#15613,#10139,.T.);
#20141=EDGE_CURVE('',#15777,#15780,#3761,.T.);
#20142=EDGE_CURVE('',#15781,#15618,#10140,.T.);
#20143=EDGE_CURVE('',#15782,#15781,#3762,.T.);
#20144=EDGE_CURVE('',#15782,#15619,#10141,.T.);
#20145=EDGE_CURVE('',#15783,#15782,#3763,.T.);
#20146=EDGE_CURVE('',#15620,#15783,#10142,.T.);
#20147=EDGE_CURVE('',#15784,#15617,#10143,.T.);
#20148=EDGE_CURVE('',#15781,#15784,#3764,.T.);
#20149=EDGE_CURVE('',#15785,#15622,#10144,.T.);
#20150=EDGE_CURVE('',#15786,#15785,#3765,.T.);
#20151=EDGE_CURVE('',#15786,#15623,#10145,.T.);
#20152=EDGE_CURVE('',#15787,#15786,#3766,.T.);
#20153=EDGE_CURVE('',#15624,#15787,#10146,.T.);
#20154=EDGE_CURVE('',#15788,#15621,#10147,.T.);
#20155=EDGE_CURVE('',#15785,#15788,#3767,.T.);
#20156=EDGE_CURVE('',#15789,#15626,#10148,.T.);
#20157=EDGE_CURVE('',#15790,#15789,#3768,.T.);
#20158=EDGE_CURVE('',#15790,#15627,#10149,.T.);
#20159=EDGE_CURVE('',#15791,#15790,#3769,.T.);
#20160=EDGE_CURVE('',#15628,#15791,#10150,.T.);
#20161=EDGE_CURVE('',#15792,#15625,#10151,.T.);
#20162=EDGE_CURVE('',#15789,#15792,#3770,.T.);
#20163=EDGE_CURVE('',#15793,#15630,#10152,.T.);
#20164=EDGE_CURVE('',#15794,#15793,#3771,.T.);
#20165=EDGE_CURVE('',#15794,#15631,#10153,.T.);
#20166=EDGE_CURVE('',#15795,#15794,#3772,.T.);
#20167=EDGE_CURVE('',#15632,#15795,#10154,.T.);
#20168=EDGE_CURVE('',#15796,#15629,#10155,.T.);
#20169=EDGE_CURVE('',#15793,#15796,#3773,.T.);
#20170=EDGE_CURVE('',#15797,#15634,#10156,.T.);
#20171=EDGE_CURVE('',#15798,#15797,#3774,.T.);
#20172=EDGE_CURVE('',#15798,#15635,#10157,.T.);
#20173=EDGE_CURVE('',#15799,#15798,#3775,.T.);
#20174=EDGE_CURVE('',#15636,#15799,#10158,.T.);
#20175=EDGE_CURVE('',#15800,#15633,#10159,.T.);
#20176=EDGE_CURVE('',#15797,#15800,#3776,.T.);
#20177=EDGE_CURVE('',#15801,#15638,#10160,.T.);
#20178=EDGE_CURVE('',#15802,#15801,#3777,.T.);
#20179=EDGE_CURVE('',#15802,#15639,#10161,.T.);
#20180=EDGE_CURVE('',#15803,#15802,#3778,.T.);
#20181=EDGE_CURVE('',#15640,#15803,#10162,.T.);
#20182=EDGE_CURVE('',#15804,#15637,#10163,.T.);
#20183=EDGE_CURVE('',#15801,#15804,#3779,.T.);
#20184=EDGE_CURVE('',#15805,#15642,#10164,.T.);
#20185=EDGE_CURVE('',#15806,#15805,#3780,.T.);
#20186=EDGE_CURVE('',#15806,#15643,#10165,.T.);
#20187=EDGE_CURVE('',#15807,#15806,#3781,.T.);
#20188=EDGE_CURVE('',#15644,#15807,#10166,.T.);
#20189=EDGE_CURVE('',#15808,#15641,#10167,.T.);
#20190=EDGE_CURVE('',#15805,#15808,#3782,.T.);
#20191=EDGE_CURVE('',#15809,#15646,#10168,.T.);
#20192=EDGE_CURVE('',#15810,#15809,#3783,.T.);
#20193=EDGE_CURVE('',#15810,#15647,#10169,.T.);
#20194=EDGE_CURVE('',#15811,#15810,#3784,.T.);
#20195=EDGE_CURVE('',#15648,#15811,#10170,.T.);
#20196=EDGE_CURVE('',#15812,#15645,#10171,.T.);
#20197=EDGE_CURVE('',#15809,#15812,#3785,.T.);
#20198=EDGE_CURVE('',#15813,#15650,#10172,.T.);
#20199=EDGE_CURVE('',#15814,#15813,#3786,.T.);
#20200=EDGE_CURVE('',#15814,#15651,#10173,.T.);
#20201=EDGE_CURVE('',#15815,#15814,#3787,.T.);
#20202=EDGE_CURVE('',#15652,#15815,#10174,.T.);
#20203=EDGE_CURVE('',#15816,#15649,#10175,.T.);
#20204=EDGE_CURVE('',#15813,#15816,#3788,.T.);
#20205=EDGE_CURVE('',#15817,#15654,#10176,.T.);
#20206=EDGE_CURVE('',#15818,#15817,#3789,.T.);
#20207=EDGE_CURVE('',#15818,#15655,#10177,.T.);
#20208=EDGE_CURVE('',#15819,#15818,#3790,.T.);
#20209=EDGE_CURVE('',#15656,#15819,#10178,.T.);
#20210=EDGE_CURVE('',#15820,#15653,#10179,.T.);
#20211=EDGE_CURVE('',#15817,#15820,#3791,.T.);
#20212=EDGE_CURVE('',#15821,#15658,#10180,.T.);
#20213=EDGE_CURVE('',#15822,#15821,#3792,.T.);
#20214=EDGE_CURVE('',#15822,#15659,#10181,.T.);
#20215=EDGE_CURVE('',#15823,#15822,#3793,.T.);
#20216=EDGE_CURVE('',#15660,#15823,#10182,.T.);
#20217=EDGE_CURVE('',#15824,#15657,#10183,.T.);
#20218=EDGE_CURVE('',#15821,#15824,#3794,.T.);
#20219=EDGE_CURVE('',#15825,#15662,#10184,.T.);
#20220=EDGE_CURVE('',#15826,#15825,#3795,.T.);
#20221=EDGE_CURVE('',#15826,#15663,#10185,.T.);
#20222=EDGE_CURVE('',#15827,#15826,#3796,.T.);
#20223=EDGE_CURVE('',#15664,#15827,#10186,.T.);
#20224=EDGE_CURVE('',#15828,#15661,#10187,.T.);
#20225=EDGE_CURVE('',#15825,#15828,#3797,.T.);
#20226=EDGE_CURVE('',#15829,#15666,#10188,.T.);
#20227=EDGE_CURVE('',#15830,#15829,#3798,.T.);
#20228=EDGE_CURVE('',#15830,#15667,#10189,.T.);
#20229=EDGE_CURVE('',#15831,#15830,#3799,.T.);
#20230=EDGE_CURVE('',#15668,#15831,#10190,.T.);
#20231=EDGE_CURVE('',#15832,#15665,#10191,.T.);
#20232=EDGE_CURVE('',#15829,#15832,#3800,.T.);
#20233=EDGE_CURVE('',#15833,#15670,#10192,.T.);
#20234=EDGE_CURVE('',#15834,#15833,#3801,.T.);
#20235=EDGE_CURVE('',#15834,#15671,#10193,.T.);
#20236=EDGE_CURVE('',#15835,#15834,#3802,.T.);
#20237=EDGE_CURVE('',#15672,#15835,#10194,.T.);
#20238=EDGE_CURVE('',#15836,#15669,#10195,.T.);
#20239=EDGE_CURVE('',#15833,#15836,#3803,.T.);
#20240=EDGE_CURVE('',#15837,#15835,#3804,.T.);
#20241=EDGE_CURVE('',#15837,#15673,#10196,.T.);
#20242=EDGE_CURVE('',#15836,#15831,#3805,.T.);
#20243=EDGE_CURVE('',#15832,#15827,#3806,.T.);
#20244=EDGE_CURVE('',#15828,#15823,#3807,.T.);
#20245=EDGE_CURVE('',#15824,#15819,#3808,.T.);
#20246=EDGE_CURVE('',#15820,#15815,#3809,.T.);
#20247=EDGE_CURVE('',#15816,#15811,#3810,.T.);
#20248=EDGE_CURVE('',#15812,#15807,#3811,.T.);
#20249=EDGE_CURVE('',#15808,#15803,#3812,.T.);
#20250=EDGE_CURVE('',#15804,#15799,#3813,.T.);
#20251=EDGE_CURVE('',#15800,#15795,#3814,.T.);
#20252=EDGE_CURVE('',#15796,#15791,#3815,.T.);
#20253=EDGE_CURVE('',#15792,#15787,#3816,.T.);
#20254=EDGE_CURVE('',#15788,#15783,#3817,.T.);
#20255=EDGE_CURVE('',#15784,#15779,#3818,.T.);
#20256=EDGE_CURVE('',#15780,#15775,#3819,.T.);
#20257=EDGE_CURVE('',#15776,#15771,#3820,.T.);
#20258=EDGE_CURVE('',#15772,#15767,#3821,.T.);
#20259=EDGE_CURVE('',#15768,#15763,#3822,.T.);
#20260=EDGE_CURVE('',#15764,#15759,#3823,.T.);
#20261=EDGE_CURVE('',#15760,#15755,#3824,.T.);
#20262=EDGE_CURVE('',#15756,#15751,#3825,.T.);
#20263=EDGE_CURVE('',#15752,#15747,#3826,.T.);
#20264=EDGE_CURVE('',#15748,#15743,#3827,.T.);
#20265=EDGE_CURVE('',#15744,#15739,#3828,.T.);
#20266=EDGE_CURVE('',#15740,#15735,#3829,.T.);
#20267=EDGE_CURVE('',#15736,#15731,#3830,.T.);
#20268=EDGE_CURVE('',#15732,#15727,#3831,.T.);
#20269=EDGE_CURVE('',#15728,#15723,#3832,.T.);
#20270=EDGE_CURVE('',#15724,#15719,#3833,.T.);
#20271=EDGE_CURVE('',#15720,#15715,#3834,.T.);
#20272=EDGE_CURVE('',#15716,#15711,#3835,.T.);
#20273=EDGE_CURVE('',#15712,#15707,#3836,.T.);
#20274=EDGE_CURVE('',#15708,#15703,#3837,.T.);
#20275=EDGE_CURVE('',#15704,#15699,#3838,.T.);
#20276=EDGE_CURVE('',#15700,#15695,#3839,.T.);
#20277=EDGE_CURVE('',#15696,#15691,#3840,.T.);
#20278=EDGE_CURVE('',#15692,#15687,#3841,.T.);
#20279=EDGE_CURVE('',#15688,#15683,#3842,.T.);
#20280=EDGE_CURVE('',#15838,#15674,#10197,.T.);
#20281=EDGE_CURVE('',#15839,#15838,#3843,.T.);
#20282=EDGE_CURVE('',#15839,#15675,#10198,.T.);
#20283=EDGE_CURVE('',#15840,#15839,#3844,.T.);
#20284=EDGE_CURVE('',#15676,#15840,#10199,.T.);
#20285=EDGE_CURVE('',#15838,#15837,#3845,.T.);
#20286=EDGE_CURVE('',#15684,#15840,#3846,.T.);
#20287=EDGE_CURVE('',#15841,#15842,#3847,.T.);
#20288=EDGE_CURVE('',#15842,#15841,#3848,.T.);
#20289=EDGE_CURVE('',#15842,#15843,#10200,.T.);
#20290=EDGE_CURVE('',#15843,#15843,#3849,.T.);
#20291=EDGE_CURVE('',#15844,#15845,#10201,.T.);
#20292=EDGE_CURVE('',#15846,#15845,#3850,.T.);
#20293=EDGE_CURVE('',#15845,#15846,#3851,.T.);
#20294=EDGE_CURVE('',#15846,#15841,#10202,.T.);
#20295=EDGE_CURVE('',#15847,#15847,#3852,.T.);
#20296=EDGE_CURVE('',#15847,#15848,#10203,.T.);
#20297=EDGE_CURVE('',#15848,#15848,#3853,.T.);
#20298=EDGE_CURVE('',#15849,#15849,#3854,.T.);
#20299=EDGE_CURVE('',#15850,#15850,#3855,.T.);
#20300=EDGE_CURVE('',#15849,#15850,#10204,.T.);
#20301=EDGE_CURVE('',#15851,#15852,#3856,.T.);
#20302=EDGE_CURVE('',#15852,#15851,#3857,.T.);
#20303=EDGE_CURVE('',#15852,#15853,#10205,.T.);
#20304=EDGE_CURVE('',#15853,#15853,#3858,.T.);
#20305=EDGE_CURVE('',#15854,#15855,#10206,.T.);
#20306=EDGE_CURVE('',#15856,#15855,#3859,.T.);
#20307=EDGE_CURVE('',#15855,#15856,#3860,.T.);
#20308=EDGE_CURVE('',#15856,#15851,#10207,.T.);
#20309=EDGE_CURVE('',#15857,#15857,#3861,.T.);
#20310=EDGE_CURVE('',#15857,#15858,#10208,.T.);
#20311=EDGE_CURVE('',#15858,#15858,#3862,.T.);
#20312=EDGE_CURVE('',#15859,#15859,#3863,.T.);
#20313=EDGE_CURVE('',#15860,#15860,#3864,.T.);
#20314=EDGE_CURVE('',#15859,#15860,#10209,.T.);
#20315=EDGE_CURVE('',#15861,#15862,#3865,.T.);
#20316=EDGE_CURVE('',#15861,#15863,#10210,.T.);
#20317=EDGE_CURVE('',#15863,#15863,#3866,.T.);
#20318=EDGE_CURVE('',#15862,#15861,#3867,.T.);
#20319=EDGE_CURVE('',#15864,#15865,#3868,.T.);
#20320=EDGE_CURVE('',#15865,#15864,#3869,.T.);
#20321=EDGE_CURVE('',#15864,#15862,#10211,.T.);
#20322=EDGE_CURVE('',#15866,#15865,#10212,.T.);
#20323=EDGE_CURVE('',#15867,#15867,#3870,.T.);
#20324=EDGE_CURVE('',#15867,#15868,#10213,.T.);
#20325=EDGE_CURVE('',#15868,#15868,#3871,.T.);
#20326=EDGE_CURVE('',#15869,#15869,#3872,.T.);
#20327=EDGE_CURVE('',#15870,#15870,#3873,.T.);
#20328=EDGE_CURVE('',#15870,#15869,#10214,.T.);
#20329=EDGE_CURVE('',#15871,#15871,#3874,.T.);
#20330=EDGE_CURVE('',#15871,#15872,#10215,.T.);
#20331=EDGE_CURVE('',#15872,#15872,#3875,.T.);
#20332=EDGE_CURVE('',#15873,#15873,#3876,.T.);
#20333=EDGE_CURVE('',#15873,#15874,#10216,.T.);
#20334=EDGE_CURVE('',#15874,#15874,#3877,.T.);
#20335=EDGE_CURVE('',#15875,#15876,#3878,.T.);
#20336=EDGE_CURVE('',#15876,#15875,#3879,.T.);
#20337=EDGE_CURVE('',#15876,#15877,#10217,.T.);
#20338=EDGE_CURVE('',#15877,#15877,#3880,.T.);
#20339=EDGE_CURVE('',#15878,#15879,#3881,.T.);
#20340=EDGE_CURVE('',#15879,#15878,#3882,.T.);
#20341=EDGE_CURVE('',#15878,#15875,#10218,.T.);
#20342=EDGE_CURVE('',#15880,#15879,#10219,.T.);
#20343=EDGE_CURVE('',#15881,#15881,#3883,.T.);
#20344=EDGE_CURVE('',#15881,#15882,#10220,.T.);
#20345=EDGE_CURVE('',#15882,#15882,#3884,.T.);
#20346=EDGE_CURVE('',#15883,#15883,#3885,.T.);
#20347=EDGE_CURVE('',#15883,#15884,#10221,.T.);
#20348=EDGE_CURVE('',#15884,#15884,#3886,.T.);
#20349=EDGE_CURVE('',#15885,#15886,#3887,.T.);
#20350=EDGE_CURVE('',#15886,#15885,#3888,.T.);
#20351=EDGE_CURVE('',#15886,#15887,#10222,.T.);
#20352=EDGE_CURVE('',#15887,#15887,#3889,.T.);
#20353=EDGE_CURVE('',#15888,#15889,#3890,.T.);
#20354=EDGE_CURVE('',#15889,#15888,#3891,.T.);
#20355=EDGE_CURVE('',#15888,#15885,#10223,.T.);
#20356=EDGE_CURVE('',#15890,#15889,#10224,.T.);
#20357=EDGE_CURVE('',#15891,#15892,#10225,.T.);
#20358=EDGE_CURVE('',#15891,#15893,#10226,.T.);
#20359=EDGE_CURVE('',#15893,#15894,#10227,.T.);
#20360=EDGE_CURVE('',#15895,#15894,#10228,.T.);
#20361=EDGE_CURVE('',#15896,#15895,#511,.T.);
#20362=EDGE_CURVE('',#15897,#15896,#10229,.T.);
#20363=EDGE_CURVE('',#15898,#15897,#10230,.T.);
#20364=EDGE_CURVE('',#15899,#15898,#10231,.T.);
#20365=EDGE_CURVE('',#15900,#15899,#10232,.T.);
#20366=EDGE_CURVE('',#15901,#15900,#10233,.T.);
#20367=EDGE_CURVE('',#15902,#15901,#10234,.T.);
#20368=EDGE_CURVE('',#15903,#15902,#10235,.T.);
#20369=EDGE_CURVE('',#15904,#15903,#10236,.T.);
#20370=EDGE_CURVE('',#15905,#15904,#10237,.T.);
#20371=EDGE_CURVE('',#15906,#15905,#512,.T.);
#20372=EDGE_CURVE('',#15892,#15906,#10238,.T.);
#20373=EDGE_CURVE('',#15907,#15908,#3892,.T.);
#20374=EDGE_CURVE('',#15908,#15909,#10239,.T.);
#20375=EDGE_CURVE('',#15909,#15910,#3893,.T.);
#20376=EDGE_CURVE('',#15910,#15907,#10240,.T.);
#20377=EDGE_CURVE('',#15910,#15911,#10241,.T.);
#20378=EDGE_CURVE('',#15911,#15912,#10242,.T.);
#20379=EDGE_CURVE('',#15912,#15907,#10243,.T.);
#20380=EDGE_CURVE('',#15913,#15914,#3894,.T.);
#20381=EDGE_CURVE('',#15914,#15915,#10244,.T.);
#20382=EDGE_CURVE('',#15915,#15916,#3895,.T.);
#20383=EDGE_CURVE('',#15916,#15913,#10245,.T.);
#20384=EDGE_CURVE('',#15916,#15917,#10246,.T.);
#20385=EDGE_CURVE('',#15917,#15918,#10247,.T.);
#20386=EDGE_CURVE('',#15918,#15919,#10248,.T.);
#20387=EDGE_CURVE('',#15919,#15920,#10249,.T.);
#20388=EDGE_CURVE('',#15920,#15913,#10250,.T.);
#20389=EDGE_CURVE('',#15908,#15921,#10251,.T.);
#20390=EDGE_CURVE('',#15905,#15921,#10252,.T.);
#20391=EDGE_CURVE('',#15904,#15922,#10253,.T.);
#20392=EDGE_CURVE('',#15922,#15909,#10254,.T.);
#20393=EDGE_CURVE('',#15922,#15923,#10255,.T.);
#20394=EDGE_CURVE('',#15923,#15924,#10256,.T.);
#20395=EDGE_CURVE('',#15897,#15924,#10257,.T.);
#20396=EDGE_CURVE('',#15911,#15896,#3896,.T.);
#20397=EDGE_CURVE('',#15925,#15915,#10258,.T.);
#20398=EDGE_CURVE('',#15926,#15925,#3897,.T.);
#20399=EDGE_CURVE('',#15926,#15927,#10259,.T.);
#20400=EDGE_CURVE('',#15928,#15927,#10260,.T.);
#20401=EDGE_CURVE('',#15929,#15928,#10261,.T.);
#20402=EDGE_CURVE('',#15929,#15917,#10262,.T.);
#20403=EDGE_CURVE('',#15914,#15930,#10263,.T.);
#20404=EDGE_CURVE('',#15925,#15930,#10264,.T.);
#20405=EDGE_CURVE('',#15931,#15912,#3898,.T.);
#20406=EDGE_CURVE('',#15932,#15931,#10265,.T.);
#20407=EDGE_CURVE('',#15933,#15932,#10266,.T.);
#20408=EDGE_CURVE('',#15934,#15933,#10267,.T.);
#20409=EDGE_CURVE('',#15930,#15934,#3899,.T.);
#20410=EDGE_CURVE('',#15935,#15920,#3900,.T.);
#20411=EDGE_CURVE('',#15936,#15935,#10268,.T.);
#20412=EDGE_CURVE('',#15937,#15936,#10269,.T.);
#20413=EDGE_CURVE('',#15938,#15937,#10270,.T.);
#20414=EDGE_CURVE('',#15921,#15938,#3901,.T.);
#20415=EDGE_CURVE('',#15939,#15939,#3902,.T.);
#20416=EDGE_CURVE('',#15940,#15940,#3903,.T.);
#20417=EDGE_CURVE('',#15940,#15941,#10271,.T.);
#20418=EDGE_CURVE('',#15942,#15941,#3904,.T.);
#20419=EDGE_CURVE('',#15941,#15942,#3905,.T.);
#20420=EDGE_CURVE('',#15895,#15931,#458,.T.);
#20421=EDGE_CURVE('',#15932,#15894,#10272,.T.);
#20422=EDGE_CURVE('',#15893,#15943,#10273,.T.);
#20423=EDGE_CURVE('',#15944,#15943,#10274,.T.);
#20424=EDGE_CURVE('',#15945,#15944,#10275,.T.);
#20425=EDGE_CURVE('',#15945,#15946,#10276,.T.);
#20426=EDGE_CURVE('',#15947,#15946,#10277,.T.);
#20427=EDGE_CURVE('',#15933,#15947,#10278,.T.);
#20428=EDGE_CURVE('',#15948,#15948,#3906,.T.);
#20429=EDGE_CURVE('',#15949,#15949,#3907,.T.);
#20430=EDGE_CURVE('',#15950,#15950,#3908,.T.);
#20431=EDGE_CURVE('',#15948,#15951,#10279,.T.);
#20432=EDGE_CURVE('',#15952,#15951,#3909,.T.);
#20433=EDGE_CURVE('',#15951,#15952,#3910,.T.);
#20434=EDGE_CURVE('',#15953,#15947,#10280,.T.);
#20435=EDGE_CURVE('',#15934,#15953,#459,.T.);
#20436=EDGE_CURVE('',#15954,#15945,#10281,.T.);
#20437=EDGE_CURVE('',#15955,#15944,#10282,.T.);
#20438=EDGE_CURVE('',#15956,#15955,#460,.T.);
#20439=EDGE_CURVE('',#15957,#15956,#10283,.T.);
#20440=EDGE_CURVE('',#15958,#15957,#461,.T.);
#20441=EDGE_CURVE('',#15959,#15958,#10284,.T.);
#20442=EDGE_CURVE('',#15960,#15959,#10285,.T.);
#20443=EDGE_CURVE('',#15961,#15960,#10286,.T.);
#20444=EDGE_CURVE('',#15962,#15961,#10287,.T.);
#20445=EDGE_CURVE('',#15954,#15962,#10288,.T.);
#20446=EDGE_CURVE('',#15950,#15963,#10289,.T.);
#20447=EDGE_CURVE('',#15964,#15963,#3911,.T.);
#20448=EDGE_CURVE('',#15963,#15964,#3912,.T.);
#20449=EDGE_CURVE('',#15965,#15954,#10290,.T.);
#20450=EDGE_CURVE('',#15965,#15946,#10291,.T.);
#20451=EDGE_CURVE('',#15966,#15891,#10292,.T.);
#20452=EDGE_CURVE('',#15966,#15943,#10293,.T.);
#20453=EDGE_CURVE('',#15949,#15967,#10294,.T.);
#20454=EDGE_CURVE('',#15968,#15967,#3913,.T.);
#20455=EDGE_CURVE('',#15967,#15968,#3914,.T.);
#20456=EDGE_CURVE('',#15969,#15966,#10295,.T.);
#20457=EDGE_CURVE('',#15970,#15969,#10296,.T.);
#20458=EDGE_CURVE('',#15971,#15970,#10297,.T.);
#20459=EDGE_CURVE('',#15959,#15971,#10298,.T.);
#20460=EDGE_CURVE('',#15957,#15958,#462,.T.);
#20461=EDGE_CURVE('',#15955,#15956,#463,.T.);
#20462=EDGE_CURVE('',#15972,#15965,#10299,.T.);
#20463=EDGE_CURVE('',#15973,#15972,#3915,.T.);
#20464=EDGE_CURVE('',#15974,#15973,#10300,.T.);
#20465=EDGE_CURVE('',#15974,#15975,#10301,.T.);
#20466=EDGE_CURVE('',#15919,#15975,#513,.T.);
#20467=EDGE_CURVE('',#15976,#15918,#10302,.T.);
#20468=EDGE_CURVE('',#15977,#15976,#10303,.T.);
#20469=EDGE_CURVE('',#15978,#15977,#10304,.T.);
#20470=EDGE_CURVE('',#15979,#15978,#10305,.T.);
#20471=EDGE_CURVE('',#15980,#15979,#10306,.T.);
#20472=EDGE_CURVE('',#15981,#15980,#10307,.T.);
#20473=EDGE_CURVE('',#15927,#15981,#10308,.T.);
#20474=EDGE_CURVE('',#15953,#15926,#514,.T.);
#20475=EDGE_CURVE('',#15982,#15983,#3916,.T.);
#20476=EDGE_CURVE('',#15983,#15984,#10309,.T.);
#20477=EDGE_CURVE('',#15985,#15984,#3917,.T.);
#20478=EDGE_CURVE('',#15984,#15985,#3918,.T.);
#20479=EDGE_CURVE('',#15983,#15986,#3919,.T.);
#20480=EDGE_CURVE('',#15987,#15986,#10310,.T.);
#20481=EDGE_CURVE('',#15988,#15987,#464,.T.);
#20482=EDGE_CURVE('',#15989,#15988,#465,.T.);
#20483=EDGE_CURVE('',#15982,#15989,#10311,.T.);
#20484=EDGE_CURVE('',#15990,#15991,#3920,.T.);
#20485=EDGE_CURVE('',#15991,#15992,#10312,.T.);
#20486=EDGE_CURVE('',#15992,#15992,#3921,.T.);
#20487=EDGE_CURVE('',#15991,#15993,#3922,.T.);
#20488=EDGE_CURVE('',#15994,#15993,#10313,.T.);
#20489=EDGE_CURVE('',#15995,#15994,#466,.T.);
#20490=EDGE_CURVE('',#15996,#15995,#467,.T.);
#20491=EDGE_CURVE('',#15990,#15996,#10314,.T.);
#20492=EDGE_CURVE('',#15997,#15994,#10315,.T.);
#20493=EDGE_CURVE('',#15997,#15995,#10316,.T.);
#20494=EDGE_CURVE('',#15996,#15997,#10317,.T.);
#20495=EDGE_CURVE('',#15998,#15999,#10318,.T.);
#20496=EDGE_CURVE('',#15998,#16000,#10319,.T.);
#20497=EDGE_CURVE('',#16000,#16001,#10320,.T.);
#20498=EDGE_CURVE('',#15999,#16001,#10321,.T.);
#20499=EDGE_CURVE('',#16002,#15998,#10322,.T.);
#20500=EDGE_CURVE('',#16002,#16003,#10323,.T.);
#20501=EDGE_CURVE('',#16003,#16000,#10324,.T.);
#20502=EDGE_CURVE('',#16004,#16002,#10325,.T.);
#20503=EDGE_CURVE('',#16004,#16005,#10326,.T.);
#20504=EDGE_CURVE('',#16005,#16003,#10327,.T.);
#20505=EDGE_CURVE('',#15986,#15982,#10328,.T.);
#20506=EDGE_CURVE('',#16006,#15990,#515,.T.);
#20507=EDGE_CURVE('',#16006,#16007,#3923,.T.);
#20508=EDGE_CURVE('',#15993,#16007,#516,.T.);
#20509=EDGE_CURVE('',#16007,#16006,#10329,.T.);
#20510=EDGE_CURVE('',#16008,#16008,#3924,.T.);
#20511=EDGE_CURVE('',#16009,#16010,#3925,.T.);
#20512=EDGE_CURVE('',#16010,#16009,#3926,.T.);
#20513=EDGE_CURVE('',#16009,#16011,#10330,.T.);
#20514=EDGE_CURVE('',#16011,#16011,#3927,.T.);
#20515=EDGE_CURVE('',#16012,#16013,#3928,.T.);
#20516=EDGE_CURVE('',#16013,#16012,#3929,.T.);
#20517=EDGE_CURVE('',#16012,#16014,#10331,.T.);
#20518=EDGE_CURVE('',#16014,#16014,#3930,.T.);
#20519=EDGE_CURVE('',#16015,#16016,#3931,.T.);
#20520=EDGE_CURVE('',#16016,#16015,#3932,.T.);
#20521=EDGE_CURVE('',#16015,#16017,#10332,.T.);
#20522=EDGE_CURVE('',#16017,#16017,#3933,.T.);
#20523=EDGE_CURVE('',#16018,#16019,#3934,.T.);
#20524=EDGE_CURVE('',#16019,#16018,#3935,.T.);
#20525=EDGE_CURVE('',#16018,#16020,#10333,.T.);
#20526=EDGE_CURVE('',#16020,#16020,#3936,.T.);
#20527=EDGE_CURVE('',#15988,#16021,#10334,.T.);
#20528=EDGE_CURVE('',#16022,#16021,#10335,.T.);
#20529=EDGE_CURVE('',#16023,#16022,#10336,.T.);
#20530=EDGE_CURVE('',#15969,#16023,#10337,.T.);
#20531=EDGE_CURVE('',#15989,#15969,#10338,.T.);
#20532=EDGE_CURVE('',#15962,#15987,#10339,.T.);
#20533=EDGE_CURVE('',#16024,#15962,#10340,.T.);
#20534=EDGE_CURVE('',#16025,#16024,#10341,.T.);
#20535=EDGE_CURVE('',#16021,#16025,#10342,.T.);
#20536=EDGE_CURVE('',#15973,#15972,#10343,.T.);
#20537=EDGE_CURVE('',#16026,#15973,#3937,.T.);
#20538=EDGE_CURVE('',#15972,#16026,#3938,.T.);
#20539=EDGE_CURVE('',#15999,#16027,#10344,.T.);
#20540=EDGE_CURVE('',#16027,#16028,#10345,.T.);
#20541=EDGE_CURVE('',#16028,#16004,#10346,.T.);
#20542=EDGE_CURVE('',#16029,#16030,#10347,.T.);
#20543=EDGE_CURVE('',#16030,#16031,#10348,.T.);
#20544=EDGE_CURVE('',#16031,#16032,#3939,.T.);
#20545=EDGE_CURVE('',#16032,#16029,#10349,.T.);
#20546=EDGE_CURVE('',#16033,#16033,#3940,.T.);
#20547=EDGE_CURVE('',#16033,#16034,#10350,.T.);
#20548=EDGE_CURVE('',#16034,#16034,#3941,.T.);
#20549=EDGE_CURVE('',#16035,#16036,#517,.T.);
#20550=EDGE_CURVE('',#16036,#16037,#10351,.T.);
#20551=EDGE_CURVE('',#16037,#16038,#518,.T.);
#20552=EDGE_CURVE('',#16038,#16039,#10352,.T.);
#20553=EDGE_CURVE('',#16040,#16039,#10353,.T.);
#20554=EDGE_CURVE('',#16035,#16040,#10354,.T.);
#20555=EDGE_CURVE('',#16041,#16042,#519,.T.);
#20556=EDGE_CURVE('',#16042,#16043,#10355,.T.);
#20557=EDGE_CURVE('',#16043,#16035,#520,.T.);
#20558=EDGE_CURVE('',#16044,#16040,#10356,.T.);
#20559=EDGE_CURVE('',#16041,#16044,#10357,.T.);
#20560=EDGE_CURVE('',#16045,#16046,#521,.T.);
#20561=EDGE_CURVE('',#16046,#16047,#10358,.T.);
#20562=EDGE_CURVE('',#16047,#16041,#522,.T.);
#20563=EDGE_CURVE('',#16048,#16044,#10359,.T.);
#20564=EDGE_CURVE('',#16045,#16048,#10360,.T.);
#20565=EDGE_CURVE('',#16049,#16050,#523,.T.);
#20566=EDGE_CURVE('',#16050,#16051,#10361,.T.);
#20567=EDGE_CURVE('',#16051,#16045,#524,.T.);
#20568=EDGE_CURVE('',#16052,#16048,#10362,.T.);
#20569=EDGE_CURVE('',#16049,#16052,#10363,.T.);
#20570=EDGE_CURVE('',#16053,#16049,#525,.T.);
#20571=EDGE_CURVE('',#16053,#16050,#3942,.T.);
#20572=EDGE_CURVE('',#16051,#16046,#3943,.T.);
#20573=EDGE_CURVE('',#16054,#16055,#526,.T.);
#20574=EDGE_CURVE('',#16056,#16054,#527,.T.);
#20575=EDGE_CURVE('',#16056,#16055,#3944,.T.);
#20576=EDGE_CURVE('',#16038,#16057,#528,.T.);
#20577=EDGE_CURVE('',#16037,#16057,#3945,.T.);
#20578=EDGE_CURVE('',#16043,#16036,#3946,.T.);
#20579=EDGE_CURVE('',#16057,#16056,#10364,.T.);
#20580=EDGE_CURVE('',#16054,#16058,#10365,.T.);
#20581=EDGE_CURVE('',#16039,#16058,#10366,.T.);
#20582=EDGE_CURVE('',#16055,#16053,#10367,.T.);
#20583=EDGE_CURVE('',#16058,#16052,#10368,.T.);
#20584=EDGE_CURVE('',#16047,#16042,#3947,.T.);
#20585=EDGE_CURVE('',#16059,#16060,#529,.T.);
#20586=EDGE_CURVE('',#16060,#16061,#10369,.T.);
#20587=EDGE_CURVE('',#16061,#16062,#530,.T.);
#20588=EDGE_CURVE('',#16062,#16063,#10370,.T.);
#20589=EDGE_CURVE('',#16064,#16063,#10371,.T.);
#20590=EDGE_CURVE('',#16059,#16064,#10372,.T.);
#20591=EDGE_CURVE('',#16065,#16066,#531,.T.);
#20592=EDGE_CURVE('',#16066,#16067,#10373,.T.);
#20593=EDGE_CURVE('',#16067,#16059,#532,.T.);
#20594=EDGE_CURVE('',#16068,#16064,#10374,.T.);
#20595=EDGE_CURVE('',#16065,#16068,#10375,.T.);
#20596=EDGE_CURVE('',#16069,#16070,#533,.T.);
#20597=EDGE_CURVE('',#16070,#16071,#10376,.T.);
#20598=EDGE_CURVE('',#16071,#16065,#534,.T.);
#20599=EDGE_CURVE('',#16072,#16068,#10377,.T.);
#20600=EDGE_CURVE('',#16069,#16072,#10378,.T.);
#20601=EDGE_CURVE('',#16073,#16074,#535,.T.);
#20602=EDGE_CURVE('',#16074,#16075,#10379,.T.);
#20603=EDGE_CURVE('',#16075,#16069,#536,.T.);
#20604=EDGE_CURVE('',#16076,#16072,#10380,.T.);
#20605=EDGE_CURVE('',#16073,#16076,#10381,.T.);
#20606=EDGE_CURVE('',#16077,#16073,#537,.T.);
#20607=EDGE_CURVE('',#16077,#16074,#3948,.T.);
#20608=EDGE_CURVE('',#16075,#16070,#3949,.T.);
#20609=EDGE_CURVE('',#16078,#16079,#538,.T.);
#20610=EDGE_CURVE('',#16080,#16078,#539,.T.);
#20611=EDGE_CURVE('',#16080,#16079,#3950,.T.);
#20612=EDGE_CURVE('',#16062,#16081,#540,.T.);
#20613=EDGE_CURVE('',#16061,#16081,#3951,.T.);
#20614=EDGE_CURVE('',#16067,#16060,#3952,.T.);
#20615=EDGE_CURVE('',#16081,#16080,#10382,.T.);
#20616=EDGE_CURVE('',#16078,#16082,#10383,.T.);
#20617=EDGE_CURVE('',#16063,#16082,#10384,.T.);
#20618=EDGE_CURVE('',#16079,#16077,#10385,.T.);
#20619=EDGE_CURVE('',#16082,#16076,#10386,.T.);
#20620=EDGE_CURVE('',#16071,#16066,#3953,.T.);
#20621=EDGE_CURVE('',#16083,#15929,#10387,.T.);
#20622=EDGE_CURVE('',#16083,#15976,#10388,.T.);
#20623=EDGE_CURVE('',#15903,#16084,#10389,.T.);
#20624=EDGE_CURVE('',#15902,#16085,#10390,.T.);
#20625=EDGE_CURVE('',#16085,#16084,#10391,.T.);
#20626=EDGE_CURVE('',#15901,#16086,#10392,.T.);
#20627=EDGE_CURVE('',#16086,#16085,#10393,.T.);
#20628=EDGE_CURVE('',#15900,#16087,#10394,.T.);
#20629=EDGE_CURVE('',#16087,#16086,#10395,.T.);
#20630=EDGE_CURVE('',#15899,#16088,#10396,.T.);
#20631=EDGE_CURVE('',#16088,#16087,#10397,.T.);
#20632=EDGE_CURVE('',#15898,#16089,#10398,.T.);
#20633=EDGE_CURVE('',#16089,#16088,#10399,.T.);
#20634=EDGE_CURVE('',#15924,#16089,#10400,.T.);
#20635=EDGE_CURVE('',#15975,#15935,#468,.T.);
#20636=EDGE_CURVE('',#15936,#15974,#10401,.T.);
#20637=EDGE_CURVE('',#15892,#15937,#10402,.T.);
#20638=EDGE_CURVE('',#15938,#15906,#469,.T.);
#20639=EDGE_CURVE('',#15956,#15955,#3954,.T.);
#20640=EDGE_CURVE('',#15958,#15957,#3955,.T.);
#20641=EDGE_CURVE('',#16090,#16091,#10403,.T.);
#20642=EDGE_CURVE('',#16091,#16092,#10404,.T.);
#20643=EDGE_CURVE('',#16092,#16093,#10405,.T.);
#20644=EDGE_CURVE('',#16093,#16094,#10406,.T.);
#20645=EDGE_CURVE('',#16094,#16095,#10407,.T.);
#20646=EDGE_CURVE('',#16095,#16090,#10408,.T.);
#20647=EDGE_CURVE('',#16096,#16097,#10409,.T.);
#20648=EDGE_CURVE('',#16090,#16097,#10410,.T.);
#20649=EDGE_CURVE('',#16095,#16096,#10411,.T.);
#20650=EDGE_CURVE('',#16098,#16096,#10412,.T.);
#20651=EDGE_CURVE('',#16094,#16098,#10413,.T.);
#20652=EDGE_CURVE('',#16093,#16099,#10414,.T.);
#20653=EDGE_CURVE('',#16098,#16099,#10415,.T.);
#20654=EDGE_CURVE('',#16100,#16099,#10416,.T.);
#20655=EDGE_CURVE('',#16092,#16100,#10417,.T.);
#20656=EDGE_CURVE('',#16101,#16100,#10418,.T.);
#20657=EDGE_CURVE('',#16091,#16101,#10419,.T.);
#20658=EDGE_CURVE('',#16097,#16101,#10420,.T.);
#20659=EDGE_CURVE('',#15955,#15956,#3956,.T.);
#20660=EDGE_CURVE('',#16102,#16103,#10421,.T.);
#20661=EDGE_CURVE('',#16103,#16104,#10422,.T.);
#20662=EDGE_CURVE('',#16104,#16105,#10423,.T.);
#20663=EDGE_CURVE('',#16105,#16106,#10424,.T.);
#20664=EDGE_CURVE('',#16106,#16107,#10425,.T.);
#20665=EDGE_CURVE('',#16107,#16102,#10426,.T.);
#20666=EDGE_CURVE('',#16108,#16109,#10427,.T.);
#20667=EDGE_CURVE('',#16102,#16109,#10428,.T.);
#20668=EDGE_CURVE('',#16107,#16108,#10429,.T.);
#20669=EDGE_CURVE('',#16110,#16108,#10430,.T.);
#20670=EDGE_CURVE('',#16106,#16110,#10431,.T.);
#20671=EDGE_CURVE('',#16105,#16111,#10432,.T.);
#20672=EDGE_CURVE('',#16110,#16111,#10433,.T.);
#20673=EDGE_CURVE('',#16112,#16111,#10434,.T.);
#20674=EDGE_CURVE('',#16104,#16112,#10435,.T.);
#20675=EDGE_CURVE('',#16113,#16112,#10436,.T.);
#20676=EDGE_CURVE('',#16103,#16113,#10437,.T.);
#20677=EDGE_CURVE('',#16109,#16113,#10438,.T.);
#20678=EDGE_CURVE('',#15957,#15958,#3957,.T.);
#20679=EDGE_CURVE('',#16028,#16114,#10439,.T.);
#20680=EDGE_CURVE('',#16114,#16005,#10440,.T.);
#20681=EDGE_CURVE('',#16027,#16115,#10441,.T.);
#20682=EDGE_CURVE('',#16114,#16115,#10442,.T.);
#20683=EDGE_CURVE('',#16001,#16115,#10443,.T.);
#20684=EDGE_CURVE('',#16116,#16116,#3958,.T.);
#20685=EDGE_CURVE('',#16026,#16116,#10444,.T.);
#20686=EDGE_CURVE('',#16117,#16118,#10445,.T.);
#20687=EDGE_CURVE('',#16119,#16118,#3959,.T.);
#20688=EDGE_CURVE('',#16118,#16119,#3960,.T.);
#20689=EDGE_CURVE('',#16119,#16120,#10446,.T.);
#20690=EDGE_CURVE('',#16121,#16120,#3961,.T.);
#20691=EDGE_CURVE('',#16120,#16121,#3962,.T.);
#20692=EDGE_CURVE('',#16121,#16122,#10447,.T.);
#20693=EDGE_CURVE('',#16122,#16122,#3963,.T.);
#20694=EDGE_CURVE('',#16123,#16124,#10448,.T.);
#20695=EDGE_CURVE('',#16125,#16124,#3964,.T.);
#20696=EDGE_CURVE('',#16124,#16125,#3965,.T.);
#20697=EDGE_CURVE('',#16125,#16126,#10449,.T.);
#20698=EDGE_CURVE('',#16127,#16126,#3966,.T.);
#20699=EDGE_CURVE('',#16126,#16127,#3967,.T.);
#20700=EDGE_CURVE('',#16127,#16128,#10450,.T.);
#20701=EDGE_CURVE('',#16128,#16128,#3968,.T.);
#20702=EDGE_CURVE('',#16129,#16130,#10451,.T.);
#20703=EDGE_CURVE('',#16131,#16130,#3969,.T.);
#20704=EDGE_CURVE('',#16130,#16131,#3970,.T.);
#20705=EDGE_CURVE('',#16131,#16132,#10452,.T.);
#20706=EDGE_CURVE('',#16133,#16132,#3971,.T.);
#20707=EDGE_CURVE('',#16132,#16133,#3972,.T.);
#20708=EDGE_CURVE('',#16133,#16134,#10453,.T.);
#20709=EDGE_CURVE('',#16134,#16134,#3973,.T.);
#20710=EDGE_CURVE('',#16135,#16136,#3974,.T.);
#20711=EDGE_CURVE('',#16136,#16135,#3975,.T.);
#20712=EDGE_CURVE('',#16136,#16137,#10454,.T.);
#20713=EDGE_CURVE('',#16137,#16137,#3976,.T.);
#20714=EDGE_CURVE('',#16135,#16138,#10455,.T.);
#20715=EDGE_CURVE('',#16139,#16138,#3977,.T.);
#20716=EDGE_CURVE('',#16138,#16139,#3978,.T.);
#20717=EDGE_CURVE('',#16140,#16139,#10456,.T.);
#20718=EDGE_CURVE('',#16141,#16142,#3979,.T.);
#20719=EDGE_CURVE('',#16142,#16141,#3980,.T.);
#20720=EDGE_CURVE('',#16142,#16143,#10457,.T.);
#20721=EDGE_CURVE('',#16143,#16143,#3981,.T.);
#20722=EDGE_CURVE('',#16141,#16144,#10458,.T.);
#20723=EDGE_CURVE('',#16145,#16144,#3982,.T.);
#20724=EDGE_CURVE('',#16144,#16145,#3983,.T.);
#20725=EDGE_CURVE('',#16146,#16145,#10459,.T.);
#20726=EDGE_CURVE('',#16147,#16148,#3984,.T.);
#20727=EDGE_CURVE('',#16148,#16147,#3985,.T.);
#20728=EDGE_CURVE('',#16148,#16149,#10460,.T.);
#20729=EDGE_CURVE('',#16149,#16149,#3986,.T.);
#20730=EDGE_CURVE('',#16147,#16150,#10461,.T.);
#20731=EDGE_CURVE('',#16151,#16150,#3987,.T.);
#20732=EDGE_CURVE('',#16150,#16151,#3988,.T.);
#20733=EDGE_CURVE('',#16152,#16151,#10462,.T.);
#20734=EDGE_CURVE('',#16153,#16154,#3989,.T.);
#20735=EDGE_CURVE('',#16154,#16153,#3990,.T.);
#20736=EDGE_CURVE('',#16154,#16155,#10463,.T.);
#20737=EDGE_CURVE('',#16155,#16155,#3991,.T.);
#20738=EDGE_CURVE('',#16153,#16156,#10464,.T.);
#20739=EDGE_CURVE('',#16157,#16156,#3992,.T.);
#20740=EDGE_CURVE('',#16156,#16157,#3993,.T.);
#20741=EDGE_CURVE('',#16158,#16157,#10465,.T.);
#20742=EDGE_CURVE('',#16159,#15968,#10466,.T.);
#20743=EDGE_CURVE('',#16160,#15942,#10467,.T.);
#20744=EDGE_CURVE('',#16161,#16010,#10468,.T.);
#20745=EDGE_CURVE('',#16162,#16013,#10469,.T.);
#20746=EDGE_CURVE('',#16163,#16016,#10470,.T.);
#20747=EDGE_CURVE('',#16164,#16019,#10471,.T.);
#20748=EDGE_CURVE('',#16165,#15952,#10472,.T.);
#20749=EDGE_CURVE('',#16166,#15964,#10473,.T.);
#20750=EDGE_CURVE('',#16167,#15961,#10474,.T.);
#20751=EDGE_CURVE('',#16168,#15960,#10475,.T.);
#20752=EDGE_CURVE('',#16167,#16168,#10476,.T.);
#20753=EDGE_CURVE('',#16169,#15959,#10477,.T.);
#20754=EDGE_CURVE('',#16168,#16169,#10478,.T.);
#20755=EDGE_CURVE('',#16170,#16021,#10479,.T.);
#20756=EDGE_CURVE('',#16171,#16025,#10480,.T.);
#20757=EDGE_CURVE('',#16170,#16171,#10481,.T.);
#20758=EDGE_CURVE('',#16172,#15971,#10482,.T.);
#20759=EDGE_CURVE('',#16169,#16172,#10483,.T.);
#20760=EDGE_CURVE('',#16173,#15970,#10484,.T.);
#20761=EDGE_CURVE('',#16172,#16173,#10485,.T.);
#20762=EDGE_CURVE('',#16174,#16023,#10486,.T.);
#20763=EDGE_CURVE('',#16173,#16174,#10487,.T.);
#20764=EDGE_CURVE('',#16175,#16022,#10488,.T.);
#20765=EDGE_CURVE('',#16174,#16175,#10489,.T.);
#20766=EDGE_CURVE('',#16175,#16170,#10490,.T.);
#20767=EDGE_CURVE('',#16171,#16176,#10491,.T.);
#20768=EDGE_CURVE('',#16176,#16167,#10492,.T.);
#20769=EDGE_CURVE('',#16177,#16178,#10493,.T.);
#20770=EDGE_CURVE('',#16178,#16179,#10494,.T.);
#20771=EDGE_CURVE('',#16179,#16180,#10495,.T.);
#20772=EDGE_CURVE('',#16180,#16181,#10496,.T.);
#20773=EDGE_CURVE('',#16181,#16182,#10497,.T.);
#20774=EDGE_CURVE('',#16182,#16183,#10498,.T.);
#20775=EDGE_CURVE('',#16183,#16184,#10499,.T.);
#20776=EDGE_CURVE('',#16184,#16177,#10500,.T.);
#20777=EDGE_CURVE('',#16185,#16185,#3994,.T.);
#20778=EDGE_CURVE('',#16186,#16186,#3995,.T.);
#20779=EDGE_CURVE('',#16186,#16187,#10501,.T.);
#20780=EDGE_CURVE('',#16187,#16187,#3996,.T.);
#20781=EDGE_CURVE('',#16188,#16189,#3997,.T.);
#20782=EDGE_CURVE('',#16189,#16190,#10502,.T.);
#20783=EDGE_CURVE('',#16190,#16190,#3998,.T.);
#20784=EDGE_CURVE('',#16189,#16188,#3999,.T.);
#20785=EDGE_CURVE('',#16084,#15923,#10503,.T.);
#20786=EDGE_CURVE('',#16191,#15981,#10504,.T.);
#20787=EDGE_CURVE('',#15928,#16191,#10505,.T.);
#20788=EDGE_CURVE('',#16192,#15980,#10506,.T.);
#20789=EDGE_CURVE('',#16191,#16192,#10507,.T.);
#20790=EDGE_CURVE('',#16193,#15979,#10508,.T.);
#20791=EDGE_CURVE('',#16192,#16193,#10509,.T.);
#20792=EDGE_CURVE('',#16194,#15978,#10510,.T.);
#20793=EDGE_CURVE('',#16193,#16194,#10511,.T.);
#20794=EDGE_CURVE('',#16195,#15977,#10512,.T.);
#20795=EDGE_CURVE('',#16194,#16195,#10513,.T.);
#20796=EDGE_CURVE('',#16195,#16083,#10514,.T.);
#20797=EDGE_CURVE('',#16176,#16024,#10515,.T.);
#20798=EDGE_CURVE('',#16196,#16197,#4000,.T.);
#20799=EDGE_CURVE('',#16197,#16196,#4001,.T.);
#20800=EDGE_CURVE('',#16197,#16198,#10516,.T.);
#20801=EDGE_CURVE('',#16198,#16198,#4002,.T.);
#20802=EDGE_CURVE('',#15939,#16199,#10517,.T.);
#20803=EDGE_CURVE('',#16200,#16199,#831,.T.);
#20804=EDGE_CURVE('',#16201,#16200,#832,.T.);
#20805=EDGE_CURVE('',#16199,#16201,#833,.T.);
#20806=EDGE_CURVE('',#15985,#16202,#10518,.T.);
#20807=EDGE_CURVE('',#16202,#16202,#4003,.T.);
#20808=EDGE_CURVE('',#16196,#16201,#10519,.T.);
#20809=EDGE_CURVE('',#16200,#16185,#10520,.T.);
#20810=EDGE_CURVE('',#16203,#16203,#4004,.T.);
#20811=EDGE_CURVE('',#16203,#16204,#10521,.T.);
#20812=EDGE_CURVE('',#16204,#16204,#4005,.T.);
#20813=EDGE_CURVE('',#16205,#16206,#4006,.T.);
#20814=EDGE_CURVE('',#16206,#16205,#4007,.T.);
#20815=EDGE_CURVE('',#16205,#16207,#10522,.T.);
#20816=EDGE_CURVE('',#16207,#16207,#4008,.T.);
#20817=EDGE_CURVE('',#16208,#16209,#10523,.T.);
#20818=EDGE_CURVE('',#16209,#16210,#10524,.T.);
#20819=EDGE_CURVE('',#16210,#16211,#10525,.T.);
#20820=EDGE_CURVE('',#16211,#16212,#10526,.T.);
#20821=EDGE_CURVE('',#16212,#16213,#10527,.T.);
#20822=EDGE_CURVE('',#16213,#16208,#10528,.T.);
#20823=EDGE_CURVE('',#16214,#16215,#10529,.T.);
#20824=EDGE_CURVE('',#16215,#16216,#10530,.T.);
#20825=EDGE_CURVE('',#16216,#16217,#10531,.T.);
#20826=EDGE_CURVE('',#16217,#16218,#10532,.T.);
#20827=EDGE_CURVE('',#16218,#16219,#10533,.T.);
#20828=EDGE_CURVE('',#16219,#16214,#10534,.T.);
#20829=EDGE_CURVE('',#16220,#16220,#4009,.T.);
#20830=EDGE_CURVE('',#16221,#16221,#4010,.T.);
#20831=EDGE_CURVE('',#16221,#16220,#10535,.T.);
#20832=EDGE_CURVE('',#16222,#16223,#4011,.T.);
#20833=EDGE_CURVE('',#16223,#16222,#4012,.T.);
#20834=EDGE_CURVE('',#16222,#16224,#10536,.T.);
#20835=EDGE_CURVE('',#16224,#16224,#4013,.T.);
#20836=EDGE_CURVE('',#16225,#16226,#4014,.T.);
#20837=EDGE_CURVE('',#16226,#16225,#4015,.T.);
#20838=EDGE_CURVE('',#16225,#16227,#10537,.T.);
#20839=EDGE_CURVE('',#16227,#16227,#4016,.T.);
#20840=EDGE_CURVE('',#16228,#16229,#10538,.T.);
#20841=EDGE_CURVE('',#16228,#16230,#10539,.T.);
#20842=EDGE_CURVE('',#16231,#16230,#4017,.T.);
#20843=EDGE_CURVE('',#16229,#16231,#10540,.T.);
#20844=EDGE_CURVE('',#16232,#16233,#4018,.T.);
#20845=EDGE_CURVE('',#16232,#16231,#834,.T.);
#20846=EDGE_CURVE('',#16230,#16233,#835,.T.);
#20847=EDGE_CURVE('',#16234,#16234,#4019,.T.);
#20848=EDGE_CURVE('',#16233,#16235,#10541,.T.);
#20849=EDGE_CURVE('',#16236,#16235,#4020,.T.);
#20850=EDGE_CURVE('',#16236,#16232,#10542,.T.);
#20851=EDGE_CURVE('',#16237,#16237,#836,.T.);
#20852=EDGE_CURVE('',#16238,#16238,#837,.T.);
#20853=EDGE_CURVE('',#16239,#16240,#4021,.T.);
#20854=EDGE_CURVE('',#16240,#16239,#4022,.T.);
#20855=EDGE_CURVE('',#16239,#16241,#10543,.T.);
#20856=EDGE_CURVE('',#16241,#16241,#4023,.T.);
#20857=EDGE_CURVE('',#16228,#16029,#10544,.T.);
#20858=EDGE_CURVE('',#16229,#16030,#10545,.T.);
#20859=EDGE_CURVE('',#16242,#16243,#10546,.T.);
#20860=EDGE_CURVE('',#16243,#16244,#10547,.T.);
#20861=EDGE_CURVE('',#16244,#16245,#10548,.T.);
#20862=EDGE_CURVE('',#16245,#16246,#10549,.T.);
#20863=EDGE_CURVE('',#16246,#16247,#10550,.T.);
#20864=EDGE_CURVE('',#16247,#16242,#10551,.T.);
#20865=EDGE_CURVE('',#16248,#16249,#10552,.T.);
#20866=EDGE_CURVE('',#16242,#16249,#10553,.T.);
#20867=EDGE_CURVE('',#16247,#16248,#10554,.T.);
#20868=EDGE_CURVE('',#16250,#16248,#10555,.T.);
#20869=EDGE_CURVE('',#16246,#16250,#10556,.T.);
#20870=EDGE_CURVE('',#16245,#16251,#10557,.T.);
#20871=EDGE_CURVE('',#16250,#16251,#10558,.T.);
#20872=EDGE_CURVE('',#16252,#16251,#10559,.T.);
#20873=EDGE_CURVE('',#16244,#16252,#10560,.T.);
#20874=EDGE_CURVE('',#16253,#16252,#10561,.T.);
#20875=EDGE_CURVE('',#16243,#16253,#10562,.T.);
#20876=EDGE_CURVE('',#16249,#16253,#10563,.T.);
#20877=EDGE_CURVE('',#16254,#16255,#10564,.T.);
#20878=EDGE_CURVE('',#16255,#16256,#10565,.T.);
#20879=EDGE_CURVE('',#16256,#16257,#10566,.T.);
#20880=EDGE_CURVE('',#16257,#16258,#10567,.T.);
#20881=EDGE_CURVE('',#16258,#16259,#10568,.T.);
#20882=EDGE_CURVE('',#16259,#16254,#10569,.T.);
#20883=EDGE_CURVE('',#16260,#16261,#10570,.T.);
#20884=EDGE_CURVE('',#16254,#16261,#10571,.T.);
#20885=EDGE_CURVE('',#16259,#16260,#10572,.T.);
#20886=EDGE_CURVE('',#16262,#16260,#10573,.T.);
#20887=EDGE_CURVE('',#16258,#16262,#10574,.T.);
#20888=EDGE_CURVE('',#16257,#16263,#10575,.T.);
#20889=EDGE_CURVE('',#16262,#16263,#10576,.T.);
#20890=EDGE_CURVE('',#16264,#16263,#10577,.T.);
#20891=EDGE_CURVE('',#16256,#16264,#10578,.T.);
#20892=EDGE_CURVE('',#16265,#16264,#10579,.T.);
#20893=EDGE_CURVE('',#16255,#16265,#10580,.T.);
#20894=EDGE_CURVE('',#16261,#16265,#10581,.T.);
#20895=EDGE_CURVE('',#16266,#16266,#4024,.T.);
#20896=EDGE_CURVE('',#16267,#16268,#4025,.T.);
#20897=EDGE_CURVE('',#16268,#16267,#4026,.T.);
#20898=EDGE_CURVE('',#16267,#16266,#10582,.T.);
#20899=EDGE_CURVE('',#16269,#16269,#838,.T.);
#20900=EDGE_CURVE('',#16269,#16268,#10583,.T.);
#20901=EDGE_CURVE('',#16270,#16271,#4027,.T.);
#20902=EDGE_CURVE('',#16271,#16270,#4028,.T.);
#20903=EDGE_CURVE('',#16271,#16272,#10584,.T.);
#20904=EDGE_CURVE('',#16272,#16272,#4029,.T.);
#20905=EDGE_CURVE('',#16273,#16273,#4030,.T.);
#20906=EDGE_CURVE('',#16274,#16275,#4031,.T.);
#20907=EDGE_CURVE('',#16275,#16274,#4032,.T.);
#20908=EDGE_CURVE('',#16274,#16273,#10585,.T.);
#20909=EDGE_CURVE('',#16276,#16277,#10586,.T.);
#20910=EDGE_CURVE('',#16277,#16278,#10587,.T.);
#20911=EDGE_CURVE('',#16278,#16279,#10588,.T.);
#20912=EDGE_CURVE('',#16279,#16280,#10589,.T.);
#20913=EDGE_CURVE('',#16280,#16281,#10590,.T.);
#20914=EDGE_CURVE('',#16281,#16276,#10591,.T.);
#20915=EDGE_CURVE('',#16282,#16283,#10592,.T.);
#20916=EDGE_CURVE('',#16276,#16283,#10593,.T.);
#20917=EDGE_CURVE('',#16281,#16282,#10594,.T.);
#20918=EDGE_CURVE('',#16284,#16282,#10595,.T.);
#20919=EDGE_CURVE('',#16280,#16284,#10596,.T.);
#20920=EDGE_CURVE('',#16279,#16285,#10597,.T.);
#20921=EDGE_CURVE('',#16284,#16285,#10598,.T.);
#20922=EDGE_CURVE('',#16286,#16285,#10599,.T.);
#20923=EDGE_CURVE('',#16278,#16286,#10600,.T.);
#20924=EDGE_CURVE('',#16287,#16286,#10601,.T.);
#20925=EDGE_CURVE('',#16277,#16287,#10602,.T.);
#20926=EDGE_CURVE('',#16283,#16287,#10603,.T.);
#20927=EDGE_CURVE('',#16288,#16289,#10604,.T.);
#20928=EDGE_CURVE('',#16289,#16290,#10605,.T.);
#20929=EDGE_CURVE('',#16290,#16291,#10606,.T.);
#20930=EDGE_CURVE('',#16291,#16292,#10607,.T.);
#20931=EDGE_CURVE('',#16292,#16293,#10608,.T.);
#20932=EDGE_CURVE('',#16293,#16288,#10609,.T.);
#20933=EDGE_CURVE('',#16294,#16295,#10610,.T.);
#20934=EDGE_CURVE('',#16288,#16295,#10611,.T.);
#20935=EDGE_CURVE('',#16293,#16294,#10612,.T.);
#20936=EDGE_CURVE('',#16296,#16294,#10613,.T.);
#20937=EDGE_CURVE('',#16292,#16296,#10614,.T.);
#20938=EDGE_CURVE('',#16291,#16297,#10615,.T.);
#20939=EDGE_CURVE('',#16296,#16297,#10616,.T.);
#20940=EDGE_CURVE('',#16298,#16297,#10617,.T.);
#20941=EDGE_CURVE('',#16290,#16298,#10618,.T.);
#20942=EDGE_CURVE('',#16299,#16298,#10619,.T.);
#20943=EDGE_CURVE('',#16289,#16299,#10620,.T.);
#20944=EDGE_CURVE('',#16295,#16299,#10621,.T.);
#20945=EDGE_CURVE('',#16300,#16300,#4033,.T.);
#20946=EDGE_CURVE('',#16301,#16302,#4034,.T.);
#20947=EDGE_CURVE('',#16302,#16301,#4035,.T.);
#20948=EDGE_CURVE('',#16301,#16300,#10622,.T.);
#20949=EDGE_CURVE('',#16303,#16303,#839,.T.);
#20950=EDGE_CURVE('',#16303,#16302,#10623,.T.);
#20951=EDGE_CURVE('',#16304,#16305,#4036,.T.);
#20952=EDGE_CURVE('',#16305,#16304,#4037,.T.);
#20953=EDGE_CURVE('',#16305,#16306,#10624,.T.);
#20954=EDGE_CURVE('',#16306,#16306,#4038,.T.);
#20955=EDGE_CURVE('',#16307,#16307,#4039,.T.);
#20956=EDGE_CURVE('',#16308,#16309,#4040,.T.);
#20957=EDGE_CURVE('',#16309,#16308,#4041,.T.);
#20958=EDGE_CURVE('',#16308,#16307,#10625,.T.);
#20959=EDGE_CURVE('',#16310,#16310,#840,.T.);
#20960=EDGE_CURVE('',#16310,#16309,#10626,.T.);
#20961=EDGE_CURVE('',#16240,#16311,#10627,.T.);
#20962=EDGE_CURVE('',#16311,#16311,#4042,.T.);
#20963=EDGE_CURVE('',#16304,#16237,#10628,.T.);
#20964=EDGE_CURVE('',#16270,#16238,#10629,.T.);
#20965=EDGE_CURVE('',#16312,#16312,#4043,.T.);
#20966=EDGE_CURVE('',#16223,#16312,#10630,.T.);
#20967=EDGE_CURVE('',#16313,#16313,#841,.T.);
#20968=EDGE_CURVE('',#16313,#16275,#10631,.T.);
#20969=EDGE_CURVE('',#16314,#16315,#4044,.T.);
#20970=EDGE_CURVE('',#16315,#16314,#4045,.T.);
#20971=EDGE_CURVE('',#16314,#16316,#10632,.T.);
#20972=EDGE_CURVE('',#16316,#16316,#4046,.T.);
#20973=EDGE_CURVE('',#16315,#16234,#10633,.T.);
#20974=EDGE_CURVE('',#16235,#16032,#842,.T.);
#20975=EDGE_CURVE('',#16031,#16236,#843,.T.);
#20976=EDGE_CURVE('',#16317,#16317,#4047,.T.);
#20977=EDGE_CURVE('',#16317,#16226,#10634,.T.);
#20978=EDGE_CURVE('',#16318,#16318,#4048,.T.);
#20979=EDGE_CURVE('',#16319,#16319,#4049,.T.);
#20980=EDGE_CURVE('',#16188,#16319,#10635,.T.);
#20981=EDGE_CURVE('',#16318,#16320,#10636,.T.);
#20982=EDGE_CURVE('',#16320,#16320,#4050,.T.);
#20983=EDGE_CURVE('',#16321,#16321,#4051,.T.);
#20984=EDGE_CURVE('',#16206,#16321,#10637,.T.);
#20985=EDGE_CURVE('',#16322,#16323,#4052,.T.);
#20986=EDGE_CURVE('',#16324,#16322,#10638,.T.);
#20987=EDGE_CURVE('',#16325,#16324,#4053,.T.);
#20988=EDGE_CURVE('',#16326,#16325,#10639,.T.);
#20989=EDGE_CURVE('',#16327,#16326,#4054,.T.);
#20990=EDGE_CURVE('',#16328,#16327,#10640,.T.);
#20991=EDGE_CURVE('',#16329,#16328,#4055,.T.);
#20992=EDGE_CURVE('',#16330,#16329,#10641,.T.);
#20993=EDGE_CURVE('',#16331,#16330,#4056,.T.);
#20994=EDGE_CURVE('',#16332,#16331,#10642,.T.);
#20995=EDGE_CURVE('',#16333,#16332,#4057,.T.);
#20996=EDGE_CURVE('',#16323,#16333,#10643,.T.);
#20997=EDGE_CURVE('',#16334,#16332,#541,.T.);
#20998=EDGE_CURVE('',#16333,#16334,#542,.T.);
#20999=EDGE_CURVE('',#16335,#16326,#543,.T.);
#21000=EDGE_CURVE('',#16325,#16336,#544,.T.);
#21001=EDGE_CURVE('',#16336,#16217,#10644,.T.);
#21002=EDGE_CURVE('',#16335,#16216,#10645,.T.);
#21003=EDGE_CURVE('',#16337,#16328,#545,.T.);
#21004=EDGE_CURVE('',#16327,#16335,#546,.T.);
#21005=EDGE_CURVE('',#16337,#16215,#10646,.T.);
#21006=EDGE_CURVE('',#16331,#16338,#547,.T.);
#21007=EDGE_CURVE('',#16338,#16330,#548,.T.);
#21008=EDGE_CURVE('',#16329,#16337,#549,.T.);
#21009=EDGE_CURVE('',#16322,#16339,#550,.T.);
#21010=EDGE_CURVE('',#16339,#16323,#551,.T.);
#21011=EDGE_CURVE('',#16336,#16324,#552,.T.);
#21012=EDGE_CURVE('',#16339,#16218,#10647,.T.);
#21013=EDGE_CURVE('',#16334,#16219,#10648,.T.);
#21014=EDGE_CURVE('',#16338,#16214,#10649,.T.);
#21015=EDGE_CURVE('',#16340,#16341,#4058,.T.);
#21016=EDGE_CURVE('',#16342,#16340,#10650,.T.);
#21017=EDGE_CURVE('',#16343,#16342,#4059,.T.);
#21018=EDGE_CURVE('',#16344,#16343,#10651,.T.);
#21019=EDGE_CURVE('',#16345,#16344,#4060,.T.);
#21020=EDGE_CURVE('',#16346,#16345,#10652,.T.);
#21021=EDGE_CURVE('',#16347,#16346,#4061,.T.);
#21022=EDGE_CURVE('',#16348,#16347,#10653,.T.);
#21023=EDGE_CURVE('',#16349,#16348,#4062,.T.);
#21024=EDGE_CURVE('',#16350,#16349,#10654,.T.);
#21025=EDGE_CURVE('',#16351,#16350,#4063,.T.);
#21026=EDGE_CURVE('',#16341,#16351,#10655,.T.);
#21027=EDGE_CURVE('',#16352,#16350,#553,.T.);
#21028=EDGE_CURVE('',#16351,#16352,#554,.T.);
#21029=EDGE_CURVE('',#16353,#16344,#555,.T.);
#21030=EDGE_CURVE('',#16343,#16354,#556,.T.);
#21031=EDGE_CURVE('',#16354,#16211,#10656,.T.);
#21032=EDGE_CURVE('',#16353,#16210,#10657,.T.);
#21033=EDGE_CURVE('',#16355,#16346,#557,.T.);
#21034=EDGE_CURVE('',#16345,#16353,#558,.T.);
#21035=EDGE_CURVE('',#16355,#16209,#10658,.T.);
#21036=EDGE_CURVE('',#16349,#16356,#559,.T.);
#21037=EDGE_CURVE('',#16356,#16348,#560,.T.);
#21038=EDGE_CURVE('',#16347,#16355,#561,.T.);
#21039=EDGE_CURVE('',#16340,#16357,#562,.T.);
#21040=EDGE_CURVE('',#16357,#16341,#563,.T.);
#21041=EDGE_CURVE('',#16354,#16342,#564,.T.);
#21042=EDGE_CURVE('',#16357,#16212,#10659,.T.);
#21043=EDGE_CURVE('',#16352,#16213,#10660,.T.);
#21044=EDGE_CURVE('',#16356,#16208,#10661,.T.);
#21045=EDGE_CURVE('',#16358,#16358,#4064,.T.);
#21046=EDGE_CURVE('',#16359,#16359,#4065,.T.);
#21047=EDGE_CURVE('',#16360,#16360,#4066,.T.);
#21048=EDGE_CURVE('',#16361,#16361,#4067,.T.);
#21049=EDGE_CURVE('',#16361,#16362,#10662,.T.);
#21050=EDGE_CURVE('',#16362,#16362,#4068,.T.);
#21051=EDGE_CURVE('',#16363,#16363,#4069,.T.);
#21052=EDGE_CURVE('',#16363,#16364,#10663,.T.);
#21053=EDGE_CURVE('',#16364,#16364,#4070,.T.);
#21054=EDGE_CURVE('',#16365,#16365,#4071,.T.);
#21055=EDGE_CURVE('',#16365,#16008,#10664,.T.);
#21056=EDGE_CURVE('',#16366,#16366,#4072,.T.);
#21057=EDGE_CURVE('',#16366,#16367,#10665,.T.);
#21058=EDGE_CURVE('',#16367,#16367,#4073,.T.);
#21059=EDGE_CURVE('',#16368,#16368,#4074,.T.);
#21060=EDGE_CURVE('',#16368,#16369,#10666,.T.);
#21061=EDGE_CURVE('',#16369,#16369,#4075,.T.);
#21062=EDGE_CURVE('',#16370,#16370,#4076,.T.);
#21063=EDGE_CURVE('',#16370,#16371,#10667,.T.);
#21064=EDGE_CURVE('',#16371,#16371,#4077,.T.);
#21065=EDGE_CURVE('',#16372,#16372,#4078,.T.);
#21066=EDGE_CURVE('',#16372,#16373,#10668,.T.);
#21067=EDGE_CURVE('',#16373,#16373,#4079,.T.);
#21068=EDGE_CURVE('',#16374,#16375,#4080,.T.);
#21069=EDGE_CURVE('',#16374,#16376,#4081,.T.);
#21070=EDGE_CURVE('',#16376,#16377,#10669,.T.);
#21071=EDGE_CURVE('',#16377,#16378,#4082,.T.);
#21072=EDGE_CURVE('',#16378,#16379,#4083,.T.);
#21073=EDGE_CURVE('',#16379,#16380,#4084,.T.);
#21074=EDGE_CURVE('',#16380,#16381,#10670,.T.);
#21075=EDGE_CURVE('',#16381,#16375,#4085,.T.);
#21076=EDGE_CURVE('',#16382,#16383,#10671,.T.);
#21077=EDGE_CURVE('',#16384,#16383,#10672,.T.);
#21078=EDGE_CURVE('',#16385,#16384,#10673,.T.);
#21079=EDGE_CURVE('',#16385,#16382,#10674,.T.);
#21080=EDGE_CURVE('',#16383,#16386,#4086,.T.);
#21081=EDGE_CURVE('',#16387,#16386,#10675,.T.);
#21082=EDGE_CURVE('',#16384,#16387,#4087,.T.);
#21083=EDGE_CURVE('',#16386,#16388,#4088,.T.);
#21084=EDGE_CURVE('',#16389,#16388,#10676,.T.);
#21085=EDGE_CURVE('',#16387,#16389,#4089,.T.);
#21086=EDGE_CURVE('',#16388,#16390,#4090,.T.);
#21087=EDGE_CURVE('',#16391,#16390,#10677,.T.);
#21088=EDGE_CURVE('',#16389,#16391,#4091,.T.);
#21089=EDGE_CURVE('',#16390,#16392,#10678,.T.);
#21090=EDGE_CURVE('',#16393,#16392,#10679,.T.);
#21091=EDGE_CURVE('',#16391,#16393,#10680,.T.);
#21092=EDGE_CURVE('',#16392,#16394,#4092,.T.);
#21093=EDGE_CURVE('',#16395,#16394,#10681,.T.);
#21094=EDGE_CURVE('',#16393,#16395,#4093,.T.);
#21095=EDGE_CURVE('',#16396,#16394,#4094,.T.);
#21096=EDGE_CURVE('',#16397,#16396,#10682,.T.);
#21097=EDGE_CURVE('',#16397,#16395,#4095,.T.);
#21098=EDGE_CURVE('',#16396,#16382,#4096,.T.);
#21099=EDGE_CURVE('',#16397,#16385,#4097,.T.);
#21100=EDGE_CURVE('',#16398,#16399,#10683,.T.);
#21101=EDGE_CURVE('',#16400,#16399,#10684,.T.);
#21102=EDGE_CURVE('',#16401,#16400,#10685,.T.);
#21103=EDGE_CURVE('',#16401,#16398,#10686,.T.);
#21104=EDGE_CURVE('',#16399,#16402,#4098,.T.);
#21105=EDGE_CURVE('',#16403,#16402,#10687,.T.);
#21106=EDGE_CURVE('',#16400,#16403,#4099,.T.);
#21107=EDGE_CURVE('',#16402,#16404,#4100,.T.);
#21108=EDGE_CURVE('',#16405,#16404,#10688,.T.);
#21109=EDGE_CURVE('',#16403,#16405,#4101,.T.);
#21110=EDGE_CURVE('',#16404,#16406,#4102,.T.);
#21111=EDGE_CURVE('',#16407,#16406,#10689,.T.);
#21112=EDGE_CURVE('',#16405,#16407,#4103,.T.);
#21113=EDGE_CURVE('',#16406,#16408,#10690,.T.);
#21114=EDGE_CURVE('',#16409,#16408,#10691,.T.);
#21115=EDGE_CURVE('',#16407,#16409,#10692,.T.);
#21116=EDGE_CURVE('',#16408,#16410,#4104,.T.);
#21117=EDGE_CURVE('',#16411,#16410,#10693,.T.);
#21118=EDGE_CURVE('',#16409,#16411,#4105,.T.);
#21119=EDGE_CURVE('',#16412,#16410,#4106,.T.);
#21120=EDGE_CURVE('',#16413,#16412,#10694,.T.);
#21121=EDGE_CURVE('',#16413,#16411,#4107,.T.);
#21122=EDGE_CURVE('',#16412,#16398,#4108,.T.);
#21123=EDGE_CURVE('',#16413,#16401,#4109,.T.);
#21124=EDGE_CURVE('',#16414,#16415,#10695,.T.);
#21125=EDGE_CURVE('',#16416,#16415,#10696,.T.);
#21126=EDGE_CURVE('',#16417,#16416,#10697,.T.);
#21127=EDGE_CURVE('',#16417,#16414,#10698,.T.);
#21128=EDGE_CURVE('',#16415,#16418,#4110,.T.);
#21129=EDGE_CURVE('',#16419,#16418,#10699,.T.);
#21130=EDGE_CURVE('',#16416,#16419,#4111,.T.);
#21131=EDGE_CURVE('',#16418,#16420,#4112,.T.);
#21132=EDGE_CURVE('',#16421,#16420,#10700,.T.);
#21133=EDGE_CURVE('',#16419,#16421,#4113,.T.);
#21134=EDGE_CURVE('',#16420,#16422,#4114,.T.);
#21135=EDGE_CURVE('',#16423,#16422,#10701,.T.);
#21136=EDGE_CURVE('',#16421,#16423,#4115,.T.);
#21137=EDGE_CURVE('',#16422,#16424,#10702,.T.);
#21138=EDGE_CURVE('',#16425,#16424,#10703,.T.);
#21139=EDGE_CURVE('',#16423,#16425,#10704,.T.);
#21140=EDGE_CURVE('',#16424,#16426,#4116,.T.);
#21141=EDGE_CURVE('',#16427,#16426,#10705,.T.);
#21142=EDGE_CURVE('',#16425,#16427,#4117,.T.);
#21143=EDGE_CURVE('',#16428,#16426,#4118,.T.);
#21144=EDGE_CURVE('',#16429,#16428,#10706,.T.);
#21145=EDGE_CURVE('',#16429,#16427,#4119,.T.);
#21146=EDGE_CURVE('',#16428,#16414,#4120,.T.);
#21147=EDGE_CURVE('',#16429,#16417,#4121,.T.);
#21148=EDGE_CURVE('',#16360,#16430,#10707,.T.);
#21149=EDGE_CURVE('',#16430,#16430,#4122,.T.);
#21150=EDGE_CURVE('',#16359,#16431,#10708,.T.);
#21151=EDGE_CURVE('',#16431,#16431,#4123,.T.);
#21152=EDGE_CURVE('',#16358,#16432,#10709,.T.);
#21153=EDGE_CURVE('',#16432,#16432,#4124,.T.);
#21154=EDGE_CURVE('',#16433,#16434,#4125,.T.);
#21155=EDGE_CURVE('',#16435,#16434,#470,.T.);
#21156=EDGE_CURVE('',#16436,#16435,#4126,.T.);
#21157=EDGE_CURVE('',#16433,#16436,#471,.T.);
#21158=EDGE_CURVE('',#16435,#16436,#10710,.T.);
#21159=EDGE_CURVE('',#16437,#16438,#4127,.T.);
#21160=EDGE_CURVE('',#16439,#16438,#4128,.T.);
#21161=EDGE_CURVE('',#16440,#16439,#4129,.T.);
#21162=EDGE_CURVE('',#16437,#16440,#4130,.T.);
#21163=EDGE_CURVE('',#16439,#16440,#10711,.T.);
#21164=EDGE_CURVE('',#16441,#16442,#472,.T.);
#21165=EDGE_CURVE('',#16441,#16443,#4131,.T.);
#21166=EDGE_CURVE('',#16444,#16443,#473,.T.);
#21167=EDGE_CURVE('',#16442,#16444,#4132,.T.);
#21168=EDGE_CURVE('',#16444,#16442,#10712,.T.);
#21169=EDGE_CURVE('',#16445,#16446,#10713,.T.);
#21170=EDGE_CURVE('',#16447,#16445,#10714,.T.);
#21171=EDGE_CURVE('',#16447,#16448,#4133,.T.);
#21172=EDGE_CURVE('',#16449,#16448,#10715,.T.);
#21173=EDGE_CURVE('',#16450,#16449,#10716,.T.);
#21174=EDGE_CURVE('',#16446,#16450,#4134,.T.);
#21175=EDGE_CURVE('',#16451,#16452,#10717,.T.);
#21176=EDGE_CURVE('',#16453,#16451,#4135,.T.);
#21177=EDGE_CURVE('',#16454,#16453,#10718,.T.);
#21178=EDGE_CURVE('',#16455,#16454,#10719,.T.);
#21179=EDGE_CURVE('',#16455,#16456,#4136,.T.);
#21180=EDGE_CURVE('',#16452,#16456,#10720,.T.);
#21181=EDGE_CURVE('',#16457,#16458,#10721,.T.);
#21182=EDGE_CURVE('',#16459,#16457,#4137,.T.);
#21183=EDGE_CURVE('',#16460,#16459,#10722,.T.);
#21184=EDGE_CURVE('',#16461,#16460,#10723,.T.);
#21185=EDGE_CURVE('',#16461,#16462,#4138,.T.);
#21186=EDGE_CURVE('',#16458,#16462,#10724,.T.);
#21187=EDGE_CURVE('',#16463,#16463,#4139,.T.);
#21188=EDGE_CURVE('',#16464,#16464,#4140,.T.);
#21189=EDGE_CURVE('',#16464,#16465,#10725,.T.);
#21190=EDGE_CURVE('',#16465,#16466,#4141,.T.);
#21191=EDGE_CURVE('',#16466,#16465,#4142,.T.);
#21192=EDGE_CURVE('',#16467,#16177,#10726,.T.);
#21193=EDGE_CURVE('',#16184,#16468,#10727,.T.);
#21194=EDGE_CURVE('',#16468,#16467,#10728,.T.);
#21195=EDGE_CURVE('',#16178,#16469,#10729,.T.);
#21196=EDGE_CURVE('',#16469,#16470,#10730,.T.);
#21197=EDGE_CURVE('',#16470,#16179,#10731,.T.);
#21198=EDGE_CURVE('',#16471,#16183,#10732,.T.);
#21199=EDGE_CURVE('',#16182,#16472,#10733,.T.);
#21200=EDGE_CURVE('',#16472,#16471,#10734,.T.);
#21201=EDGE_CURVE('',#16473,#16181,#10735,.T.);
#21202=EDGE_CURVE('',#16180,#16474,#10736,.T.);
#21203=EDGE_CURVE('',#16474,#16473,#10737,.T.);
#21204=EDGE_CURVE('',#16475,#16441,#10738,.T.);
#21205=EDGE_CURVE('',#16443,#16476,#10739,.T.);
#21206=EDGE_CURVE('',#16450,#16476,#10740,.T.);
#21207=EDGE_CURVE('',#16449,#16477,#10741,.T.);
#21208=EDGE_CURVE('',#16478,#16477,#10742,.T.);
#21209=EDGE_CURVE('',#16478,#16454,#10743,.T.);
#21210=EDGE_CURVE('',#16453,#16475,#10744,.T.);
#21211=EDGE_CURVE('',#16451,#16479,#10745,.T.);
#21212=EDGE_CURVE('',#16479,#16475,#4143,.T.);
#21213=EDGE_CURVE('',#16480,#16437,#10746,.T.);
#21214=EDGE_CURVE('',#16438,#16479,#10747,.T.);
#21215=EDGE_CURVE('',#16452,#16481,#10748,.T.);
#21216=EDGE_CURVE('',#16482,#16481,#10749,.T.);
#21217=EDGE_CURVE('',#16482,#16460,#10750,.T.);
#21218=EDGE_CURVE('',#16459,#16480,#10751,.T.);
#21219=EDGE_CURVE('',#16457,#16483,#10752,.T.);
#21220=EDGE_CURVE('',#16483,#16480,#4144,.T.);
#21221=EDGE_CURVE('',#16484,#16433,#10753,.T.);
#21222=EDGE_CURVE('',#16434,#16483,#10754,.T.);
#21223=EDGE_CURVE('',#16458,#16485,#10755,.T.);
#21224=EDGE_CURVE('',#16486,#16485,#10756,.T.);
#21225=EDGE_CURVE('',#16486,#16487,#10757,.T.);
#21226=EDGE_CURVE('',#16487,#16488,#10758,.T.);
#21227=EDGE_CURVE('',#16488,#16484,#10759,.T.);
#21228=EDGE_CURVE('',#16488,#16489,#4145,.T.);
#21229=EDGE_CURVE('',#16489,#16490,#10760,.T.);
#21230=EDGE_CURVE('',#16490,#16484,#4146,.T.);
#21231=EDGE_CURVE('',#16491,#16492,#10761,.T.);
#21232=EDGE_CURVE('',#16492,#16493,#4147,.T.);
#21233=EDGE_CURVE('',#16494,#16493,#10762,.T.);
#21234=EDGE_CURVE('',#16494,#16495,#4148,.T.);
#21235=EDGE_CURVE('',#16495,#16490,#10763,.T.);
#21236=EDGE_CURVE('',#16489,#16496,#10764,.T.);
#21237=EDGE_CURVE('',#16496,#16497,#10765,.T.);
#21238=EDGE_CURVE('',#16498,#16497,#10766,.T.);
#21239=EDGE_CURVE('',#16498,#16445,#10767,.T.);
#21240=EDGE_CURVE('',#16446,#16491,#10768,.T.);
#21241=EDGE_CURVE('',#16476,#16491,#4149,.T.);
#21242=EDGE_CURVE('',#16499,#16498,#10769,.T.);
#21243=EDGE_CURVE('',#16500,#16497,#10770,.T.);
#21244=EDGE_CURVE('',#16501,#16500,#4150,.T.);
#21245=EDGE_CURVE('',#16501,#16486,#10771,.T.);
#21246=EDGE_CURVE('',#16502,#16485,#10772,.T.);
#21247=EDGE_CURVE('',#16503,#16502,#4151,.T.);
#21248=EDGE_CURVE('',#16503,#16482,#10773,.T.);
#21249=EDGE_CURVE('',#16504,#16481,#10774,.T.);
#21250=EDGE_CURVE('',#16505,#16504,#4152,.T.);
#21251=EDGE_CURVE('',#16505,#16478,#10775,.T.);
#21252=EDGE_CURVE('',#16506,#16477,#10776,.T.);
#21253=EDGE_CURVE('',#16499,#16506,#4153,.T.);
#21254=EDGE_CURVE('',#16496,#16507,#10777,.T.);
#21255=EDGE_CURVE('',#16507,#16500,#10778,.T.);
#21256=EDGE_CURVE('',#16508,#16507,#4154,.T.);
#21257=EDGE_CURVE('',#16508,#16501,#10779,.T.);
#21258=EDGE_CURVE('',#16508,#16487,#10780,.T.);
#21259=EDGE_CURVE('',#16462,#16502,#10781,.T.);
#21260=EDGE_CURVE('',#16461,#16503,#10782,.T.);
#21261=EDGE_CURVE('',#16456,#16504,#10783,.T.);
#21262=EDGE_CURVE('',#16455,#16505,#10784,.T.);
#21263=EDGE_CURVE('',#16448,#16506,#10785,.T.);
#21264=EDGE_CURVE('',#16447,#16499,#10786,.T.);
#21265=EDGE_CURVE('',#16492,#16495,#4155,.T.);
#21266=EDGE_CURVE('',#16493,#16494,#4156,.T.);
#21267=EDGE_CURVE('',#16509,#16510,#4157,.T.);
#21268=EDGE_CURVE('',#16511,#16510,#10787,.T.);
#21269=EDGE_CURVE('',#16512,#16511,#4158,.T.);
#21270=EDGE_CURVE('',#16512,#16509,#10788,.T.);
#21271=EDGE_CURVE('',#16510,#16513,#10789,.T.);
#21272=EDGE_CURVE('',#16514,#16513,#10790,.T.);
#21273=EDGE_CURVE('',#16511,#16514,#10791,.T.);
#21274=EDGE_CURVE('',#16513,#16515,#4159,.T.);
#21275=EDGE_CURVE('',#16516,#16515,#10792,.T.);
#21276=EDGE_CURVE('',#16514,#16516,#4160,.T.);
#21277=EDGE_CURVE('',#16517,#16515,#4161,.T.);
#21278=EDGE_CURVE('',#16518,#16517,#10793,.T.);
#21279=EDGE_CURVE('',#16518,#16516,#4162,.T.);
#21280=EDGE_CURVE('',#16517,#16519,#4163,.T.);
#21281=EDGE_CURVE('',#16520,#16519,#10794,.T.);
#21282=EDGE_CURVE('',#16518,#16520,#4164,.T.);
#21283=EDGE_CURVE('',#16519,#16521,#10795,.T.);
#21284=EDGE_CURVE('',#16522,#16521,#10796,.T.);
#21285=EDGE_CURVE('',#16520,#16522,#10797,.T.);
#21286=EDGE_CURVE('',#16521,#16523,#4165,.T.);
#21287=EDGE_CURVE('',#16524,#16523,#10798,.T.);
#21288=EDGE_CURVE('',#16522,#16524,#4166,.T.);
#21289=EDGE_CURVE('',#16523,#16509,#4167,.T.);
#21290=EDGE_CURVE('',#16524,#16512,#4168,.T.);
#21291=EDGE_CURVE('',#16525,#16526,#10799,.T.);
#21292=EDGE_CURVE('',#16527,#16526,#10800,.T.);
#21293=EDGE_CURVE('',#16528,#16527,#10801,.T.);
#21294=EDGE_CURVE('',#16528,#16525,#10802,.T.);
#21295=EDGE_CURVE('',#16526,#16529,#4169,.T.);
#21296=EDGE_CURVE('',#16530,#16529,#10803,.T.);
#21297=EDGE_CURVE('',#16527,#16530,#4170,.T.);
#21298=EDGE_CURVE('',#16531,#16529,#4171,.T.);
#21299=EDGE_CURVE('',#16532,#16531,#10804,.T.);
#21300=EDGE_CURVE('',#16532,#16530,#4172,.T.);
#21301=EDGE_CURVE('',#16531,#16533,#4173,.T.);
#21302=EDGE_CURVE('',#16534,#16533,#10805,.T.);
#21303=EDGE_CURVE('',#16532,#16534,#4174,.T.);
#21304=EDGE_CURVE('',#16533,#16535,#10806,.T.);
#21305=EDGE_CURVE('',#16536,#16535,#10807,.T.);
#21306=EDGE_CURVE('',#16534,#16536,#10808,.T.);
#21307=EDGE_CURVE('',#16535,#16537,#4175,.T.);
#21308=EDGE_CURVE('',#16538,#16537,#10809,.T.);
#21309=EDGE_CURVE('',#16536,#16538,#4176,.T.);
#21310=EDGE_CURVE('',#16537,#16539,#4177,.T.);
#21311=EDGE_CURVE('',#16540,#16539,#10810,.T.);
#21312=EDGE_CURVE('',#16538,#16540,#4178,.T.);
#21313=EDGE_CURVE('',#16539,#16525,#4179,.T.);
#21314=EDGE_CURVE('',#16540,#16528,#4180,.T.);
#21315=EDGE_CURVE('',#16541,#16542,#4181,.T.);
#21316=EDGE_CURVE('',#16543,#16542,#10811,.T.);
#21317=EDGE_CURVE('',#16544,#16543,#4182,.T.);
#21318=EDGE_CURVE('',#16544,#16541,#10812,.T.);
#21319=EDGE_CURVE('',#16542,#16545,#4183,.T.);
#21320=EDGE_CURVE('',#16546,#16545,#10813,.T.);
#21321=EDGE_CURVE('',#16543,#16546,#4184,.T.);
#21322=EDGE_CURVE('',#16545,#16547,#10814,.T.);
#21323=EDGE_CURVE('',#16548,#16547,#10815,.T.);
#21324=EDGE_CURVE('',#16546,#16548,#10816,.T.);
#21325=EDGE_CURVE('',#16547,#16549,#4185,.T.);
#21326=EDGE_CURVE('',#16550,#16549,#10817,.T.);
#21327=EDGE_CURVE('',#16548,#16550,#4186,.T.);
#21328=EDGE_CURVE('',#16551,#16549,#4187,.T.);
#21329=EDGE_CURVE('',#16552,#16551,#10818,.T.);
#21330=EDGE_CURVE('',#16552,#16550,#4188,.T.);
#21331=EDGE_CURVE('',#16551,#16553,#4189,.T.);
#21332=EDGE_CURVE('',#16554,#16553,#10819,.T.);
#21333=EDGE_CURVE('',#16552,#16554,#4190,.T.);
#21334=EDGE_CURVE('',#16553,#16555,#10820,.T.);
#21335=EDGE_CURVE('',#16556,#16555,#10821,.T.);
#21336=EDGE_CURVE('',#16554,#16556,#10822,.T.);
#21337=EDGE_CURVE('',#16555,#16541,#4191,.T.);
#21338=EDGE_CURVE('',#16556,#16544,#4192,.T.);
#21339=EDGE_CURVE('',#16557,#16558,#4193,.T.);
#21340=EDGE_CURVE('',#16559,#16558,#10823,.T.);
#21341=EDGE_CURVE('',#16560,#16559,#4194,.T.);
#21342=EDGE_CURVE('',#16560,#16557,#10824,.T.);
#21343=EDGE_CURVE('',#16558,#16561,#4195,.T.);
#21344=EDGE_CURVE('',#16562,#16561,#10825,.T.);
#21345=EDGE_CURVE('',#16559,#16562,#4196,.T.);
#21346=EDGE_CURVE('',#16561,#16563,#10826,.T.);
#21347=EDGE_CURVE('',#16564,#16563,#10827,.T.);
#21348=EDGE_CURVE('',#16562,#16564,#10828,.T.);
#21349=EDGE_CURVE('',#16563,#16565,#4197,.T.);
#21350=EDGE_CURVE('',#16566,#16565,#10829,.T.);
#21351=EDGE_CURVE('',#16564,#16566,#4198,.T.);
#21352=EDGE_CURVE('',#16567,#16565,#4199,.T.);
#21353=EDGE_CURVE('',#16568,#16567,#10830,.T.);
#21354=EDGE_CURVE('',#16568,#16566,#4200,.T.);
#21355=EDGE_CURVE('',#16567,#16569,#4201,.T.);
#21356=EDGE_CURVE('',#16570,#16569,#10831,.T.);
#21357=EDGE_CURVE('',#16568,#16570,#4202,.T.);
#21358=EDGE_CURVE('',#16569,#16571,#10832,.T.);
#21359=EDGE_CURVE('',#16572,#16571,#10833,.T.);
#21360=EDGE_CURVE('',#16570,#16572,#10834,.T.);
#21361=EDGE_CURVE('',#16571,#16557,#4203,.T.);
#21362=EDGE_CURVE('',#16572,#16560,#4204,.T.);
#21363=EDGE_CURVE('',#16573,#16574,#4205,.T.);
#21364=EDGE_CURVE('',#16374,#16573,#10835,.T.);
#21365=EDGE_CURVE('',#16375,#16574,#10836,.T.);
#21366=EDGE_CURVE('',#16575,#16574,#4206,.T.);
#21367=EDGE_CURVE('',#16381,#16575,#10837,.T.);
#21368=EDGE_CURVE('',#16576,#16575,#10838,.T.);
#21369=EDGE_CURVE('',#16380,#16576,#10839,.T.);
#21370=EDGE_CURVE('',#16577,#16576,#4207,.T.);
#21371=EDGE_CURVE('',#16379,#16577,#10840,.T.);
#21372=EDGE_CURVE('',#16578,#16577,#4208,.T.);
#21373=EDGE_CURVE('',#16378,#16578,#10841,.T.);
#21374=EDGE_CURVE('',#16579,#16578,#4209,.T.);
#21375=EDGE_CURVE('',#16377,#16579,#10842,.T.);
#21376=EDGE_CURVE('',#16573,#16580,#4210,.T.);
#21377=EDGE_CURVE('',#16376,#16580,#10843,.T.);
#21378=EDGE_CURVE('',#16580,#16579,#10844,.T.);
#21379=EDGE_CURVE('',#16466,#16581,#4211,.T.);
#21380=EDGE_CURVE('',#16581,#16581,#4212,.T.);
#21381=EDGE_CURVE('',#16582,#16583,#10845,.T.);
#21382=EDGE_CURVE('',#16583,#16584,#10846,.T.);
#21383=EDGE_CURVE('',#16584,#16585,#10847,.T.);
#21384=EDGE_CURVE('',#16585,#16586,#10848,.T.);
#21385=EDGE_CURVE('',#16586,#16587,#10849,.T.);
#21386=EDGE_CURVE('',#16587,#16588,#10850,.T.);
#21387=EDGE_CURVE('',#16588,#16589,#10851,.T.);
#21388=EDGE_CURVE('',#16589,#16582,#10852,.T.);
#21389=EDGE_CURVE('',#16582,#16468,#10853,.T.);
#21390=EDGE_CURVE('',#16589,#16467,#10854,.T.);
#21391=EDGE_CURVE('',#16588,#16469,#10855,.T.);
#21392=EDGE_CURVE('',#16587,#16470,#10856,.T.);
#21393=EDGE_CURVE('',#16585,#16473,#10857,.T.);
#21394=EDGE_CURVE('',#16584,#16472,#10858,.T.);
#21395=EDGE_CURVE('',#16583,#16471,#10859,.T.);
#21396=EDGE_CURVE('',#16586,#16474,#10860,.T.);
#21397=EDGE_CURVE('',#16590,#16591,#4213,.T.);
#21398=EDGE_CURVE('',#16591,#16590,#4214,.T.);
#21399=EDGE_CURVE('',#16591,#16592,#10861,.T.);
#21400=EDGE_CURVE('',#16592,#16592,#4215,.T.);
#21401=EDGE_CURVE('',#16590,#16593,#10862,.T.);
#21402=EDGE_CURVE('',#16594,#16593,#4216,.T.);
#21403=EDGE_CURVE('',#16593,#16594,#4217,.T.);
#21404=EDGE_CURVE('',#16594,#16463,#10863,.T.);
#21405=EDGE_CURVE('',#16595,#16596,#10864,.T.);
#21406=EDGE_CURVE('',#16597,#16596,#10865,.T.);
#21407=EDGE_CURVE('',#16598,#16597,#10866,.T.);
#21408=EDGE_CURVE('',#16598,#16595,#10867,.T.);
#21409=EDGE_CURVE('',#16596,#16599,#10868,.T.);
#21410=EDGE_CURVE('',#16600,#16599,#10869,.T.);
#21411=EDGE_CURVE('',#16597,#16600,#10870,.T.);
#21412=EDGE_CURVE('',#16599,#16601,#10871,.T.);
#21413=EDGE_CURVE('',#16602,#16601,#10872,.T.);
#21414=EDGE_CURVE('',#16600,#16602,#10873,.T.);
#21415=EDGE_CURVE('',#16603,#16601,#10874,.T.);
#21416=EDGE_CURVE('',#16604,#16603,#10875,.T.);
#21417=EDGE_CURVE('',#16602,#16604,#10876,.T.);
#21418=EDGE_CURVE('',#16603,#16605,#10877,.T.);
#21419=EDGE_CURVE('',#16606,#16605,#10878,.T.);
#21420=EDGE_CURVE('',#16604,#16606,#10879,.T.);
#21421=EDGE_CURVE('',#16606,#16598,#10880,.T.);
#21422=EDGE_CURVE('',#16605,#16595,#10881,.T.);
#21423=EDGE_CURVE('',#16607,#16607,#4218,.T.);
#21424=EDGE_CURVE('',#16607,#16608,#10882,.T.);
#21425=EDGE_CURVE('',#16608,#16608,#4219,.T.);
#21426=EDGE_CURVE('',#16609,#16609,#844,.T.);
#21427=EDGE_CURVE('',#16610,#16610,#845,.T.);
#21428=EDGE_CURVE('',#16611,#16611,#846,.T.);
#21429=EDGE_CURVE('',#16611,#16612,#10883,.T.);
#21430=EDGE_CURVE('',#16612,#16612,#847,.T.);
#21431=EDGE_CURVE('',#16613,#16613,#848,.T.);
#21432=EDGE_CURVE('',#16613,#16614,#10884,.T.);
#21433=EDGE_CURVE('',#16614,#16614,#849,.T.);
#21434=EDGE_CURVE('',#16609,#16615,#10885,.T.);
#21435=EDGE_CURVE('',#16616,#16615,#850,.T.);
#21436=EDGE_CURVE('',#16615,#16616,#851,.T.);
#21437=EDGE_CURVE('',#16610,#16617,#10886,.T.);
#21438=EDGE_CURVE('',#16618,#16617,#852,.T.);
#21439=EDGE_CURVE('',#16617,#16618,#853,.T.);
#21440=EDGE_CURVE('',#16619,#16619,#4220,.T.);
#21441=EDGE_CURVE('',#16619,#16620,#10887,.T.);
#21442=EDGE_CURVE('',#16620,#16620,#4221,.T.);
#21443=EDGE_CURVE('',#16621,#16622,#4222,.T.);
#21444=EDGE_CURVE('',#16622,#16621,#4223,.T.);
#21445=EDGE_CURVE('',#16622,#16623,#10888,.T.);
#21446=EDGE_CURVE('',#16624,#16623,#4224,.T.);
#21447=EDGE_CURVE('',#16623,#16624,#4225,.T.);
#21448=EDGE_CURVE('',#16621,#16625,#10889,.T.);
#21449=EDGE_CURVE('',#16625,#16625,#4226,.T.);
#21450=EDGE_CURVE('',#16626,#16627,#4227,.T.);
#21451=EDGE_CURVE('',#16627,#16626,#4228,.T.);
#21452=EDGE_CURVE('',#16626,#16628,#10890,.T.);
#21453=EDGE_CURVE('',#16628,#16628,#4229,.T.);
#21454=EDGE_CURVE('',#16627,#16629,#10891,.T.);
#21455=EDGE_CURVE('',#16630,#16629,#4230,.T.);
#21456=EDGE_CURVE('',#16629,#16630,#4231,.T.);
#21457=EDGE_CURVE('',#16630,#16624,#10892,.T.);
#21458=ORIENTED_EDGE('',*,*,#16631,.F.);
#21459=ORIENTED_EDGE('',*,*,#16632,.T.);
#21460=ORIENTED_EDGE('',*,*,#16633,.F.);
#21461=ORIENTED_EDGE('',*,*,#16634,.F.);
#21462=ORIENTED_EDGE('',*,*,#16635,.F.);
#21463=ORIENTED_EDGE('',*,*,#16636,.F.);
#21464=ORIENTED_EDGE('',*,*,#16637,.F.);
#21465=ORIENTED_EDGE('',*,*,#16638,.F.);
#21466=ORIENTED_EDGE('',*,*,#16639,.F.);
#21467=ORIENTED_EDGE('',*,*,#16638,.T.);
#21468=ORIENTED_EDGE('',*,*,#16640,.F.);
#21469=ORIENTED_EDGE('',*,*,#16632,.F.);
#21470=ORIENTED_EDGE('',*,*,#16641,.T.);
#21471=ORIENTED_EDGE('',*,*,#16642,.T.);
#21472=ORIENTED_EDGE('',*,*,#16643,.T.);
#21473=ORIENTED_EDGE('',*,*,#16644,.T.);
#21474=ORIENTED_EDGE('',*,*,#16645,.F.);
#21475=ORIENTED_EDGE('',*,*,#16646,.T.);
#21476=ORIENTED_EDGE('',*,*,#16647,.T.);
#21477=ORIENTED_EDGE('',*,*,#16648,.T.);
#21478=ORIENTED_EDGE('',*,*,#16649,.T.);
#21479=ORIENTED_EDGE('',*,*,#16650,.F.);
#21480=ORIENTED_EDGE('',*,*,#16651,.T.);
#21481=ORIENTED_EDGE('',*,*,#16652,.T.);
#21482=ORIENTED_EDGE('',*,*,#16653,.T.);
#21483=ORIENTED_EDGE('',*,*,#16654,.T.);
#21484=ORIENTED_EDGE('',*,*,#16655,.F.);
#21485=ORIENTED_EDGE('',*,*,#16633,.T.);
#21486=ORIENTED_EDGE('',*,*,#16640,.T.);
#21487=ORIENTED_EDGE('',*,*,#16637,.T.);
#21488=ORIENTED_EDGE('',*,*,#16656,.T.);
#21489=ORIENTED_EDGE('',*,*,#16634,.T.);
#21490=ORIENTED_EDGE('',*,*,#16656,.F.);
#21491=ORIENTED_EDGE('',*,*,#16636,.T.);
#21492=ORIENTED_EDGE('',*,*,#16657,.F.);
#21493=ORIENTED_EDGE('',*,*,#16658,.F.);
#21494=ORIENTED_EDGE('',*,*,#16644,.F.);
#21495=ORIENTED_EDGE('',*,*,#16659,.T.);
#21496=ORIENTED_EDGE('',*,*,#16660,.F.);
#21497=ORIENTED_EDGE('',*,*,#16643,.F.);
#21498=ORIENTED_EDGE('',*,*,#16661,.T.);
#21499=ORIENTED_EDGE('',*,*,#16662,.F.);
#21500=ORIENTED_EDGE('',*,*,#16659,.F.);
#21501=ORIENTED_EDGE('',*,*,#16642,.F.);
#21502=ORIENTED_EDGE('',*,*,#16663,.T.);
#21503=ORIENTED_EDGE('',*,*,#16664,.F.);
#21504=ORIENTED_EDGE('',*,*,#16661,.F.);
#21505=ORIENTED_EDGE('',*,*,#16665,.F.);
#21506=ORIENTED_EDGE('',*,*,#16666,.F.);
#21507=ORIENTED_EDGE('',*,*,#16663,.F.);
#21508=ORIENTED_EDGE('',*,*,#16641,.F.);
#21509=ORIENTED_EDGE('',*,*,#16667,.F.);
#21510=ORIENTED_EDGE('',*,*,#16649,.F.);
#21511=ORIENTED_EDGE('',*,*,#16668,.T.);
#21512=ORIENTED_EDGE('',*,*,#16669,.F.);
#21513=ORIENTED_EDGE('',*,*,#16648,.F.);
#21514=ORIENTED_EDGE('',*,*,#16670,.T.);
#21515=ORIENTED_EDGE('',*,*,#16671,.F.);
#21516=ORIENTED_EDGE('',*,*,#16668,.F.);
#21517=ORIENTED_EDGE('',*,*,#16647,.F.);
#21518=ORIENTED_EDGE('',*,*,#16672,.T.);
#21519=ORIENTED_EDGE('',*,*,#16673,.F.);
#21520=ORIENTED_EDGE('',*,*,#16670,.F.);
#21521=ORIENTED_EDGE('',*,*,#16674,.F.);
#21522=ORIENTED_EDGE('',*,*,#16675,.F.);
#21523=ORIENTED_EDGE('',*,*,#16672,.F.);
#21524=ORIENTED_EDGE('',*,*,#16646,.F.);
#21525=ORIENTED_EDGE('',*,*,#16667,.T.);
#21526=ORIENTED_EDGE('',*,*,#16676,.F.);
#21527=ORIENTED_EDGE('',*,*,#16677,.T.);
#21528=ORIENTED_EDGE('',*,*,#16650,.T.);
#21529=ORIENTED_EDGE('',*,*,#16658,.T.);
#21530=ORIENTED_EDGE('',*,*,#16678,.F.);
#21531=ORIENTED_EDGE('',*,*,#16674,.T.);
#21532=ORIENTED_EDGE('',*,*,#16645,.T.);
#21533=ORIENTED_EDGE('',*,*,#16653,.F.);
#21534=ORIENTED_EDGE('',*,*,#16679,.T.);
#21535=ORIENTED_EDGE('',*,*,#16680,.F.);
#21536=ORIENTED_EDGE('',*,*,#16681,.F.);
#21537=ORIENTED_EDGE('',*,*,#16652,.F.);
#21538=ORIENTED_EDGE('',*,*,#16682,.T.);
#21539=ORIENTED_EDGE('',*,*,#16683,.F.);
#21540=ORIENTED_EDGE('',*,*,#16679,.F.);
#21541=ORIENTED_EDGE('',*,*,#16677,.F.);
#21542=ORIENTED_EDGE('',*,*,#16684,.F.);
#21543=ORIENTED_EDGE('',*,*,#16682,.F.);
#21544=ORIENTED_EDGE('',*,*,#16651,.F.);
#21545=ORIENTED_EDGE('',*,*,#16685,.F.);
#21546=ORIENTED_EDGE('',*,*,#16654,.F.);
#21547=ORIENTED_EDGE('',*,*,#16681,.T.);
#21548=ORIENTED_EDGE('',*,*,#16686,.F.);
#21549=ORIENTED_EDGE('',*,*,#16665,.T.);
#21550=ORIENTED_EDGE('',*,*,#16655,.T.);
#21551=ORIENTED_EDGE('',*,*,#16685,.T.);
#21552=ORIENTED_EDGE('',*,*,#16687,.F.);
#21553=ORIENTED_EDGE('',*,*,#16666,.T.);
#21554=ORIENTED_EDGE('',*,*,#16687,.T.);
#21555=ORIENTED_EDGE('',*,*,#16686,.T.);
#21556=ORIENTED_EDGE('',*,*,#16680,.T.);
#21557=ORIENTED_EDGE('',*,*,#16683,.T.);
#21558=ORIENTED_EDGE('',*,*,#16684,.T.);
#21559=ORIENTED_EDGE('',*,*,#16676,.T.);
#21560=ORIENTED_EDGE('',*,*,#16669,.T.);
#21561=ORIENTED_EDGE('',*,*,#16671,.T.);
#21562=ORIENTED_EDGE('',*,*,#16673,.T.);
#21563=ORIENTED_EDGE('',*,*,#16675,.T.);
#21564=ORIENTED_EDGE('',*,*,#16678,.T.);
#21565=ORIENTED_EDGE('',*,*,#16660,.T.);
#21566=ORIENTED_EDGE('',*,*,#16662,.T.);
#21567=ORIENTED_EDGE('',*,*,#16664,.T.);
#21568=ORIENTED_EDGE('',*,*,#16631,.T.);
#21569=ORIENTED_EDGE('',*,*,#16657,.T.);
#21570=ORIENTED_EDGE('',*,*,#16635,.T.);
#21571=ORIENTED_EDGE('',*,*,#16639,.T.);
#21572=ORIENTED_EDGE('',*,*,#16688,.T.);
#21573=ORIENTED_EDGE('',*,*,#16689,.T.);
#21574=ORIENTED_EDGE('',*,*,#16690,.T.);
#21575=ORIENTED_EDGE('',*,*,#16691,.T.);
#21576=ORIENTED_EDGE('',*,*,#16692,.T.);
#21577=ORIENTED_EDGE('',*,*,#16693,.T.);
#21578=ORIENTED_EDGE('',*,*,#16694,.T.);
#21579=ORIENTED_EDGE('',*,*,#16695,.T.);
#21580=ORIENTED_EDGE('',*,*,#16696,.T.);
#21581=ORIENTED_EDGE('',*,*,#16697,.T.);
#21582=ORIENTED_EDGE('',*,*,#16698,.T.);
#21583=ORIENTED_EDGE('',*,*,#16699,.T.);
#21584=ORIENTED_EDGE('',*,*,#16700,.T.);
#21585=ORIENTED_EDGE('',*,*,#16701,.F.);
#21586=ORIENTED_EDGE('',*,*,#16702,.T.);
#21587=ORIENTED_EDGE('',*,*,#16703,.F.);
#21588=ORIENTED_EDGE('',*,*,#16704,.T.);
#21589=ORIENTED_EDGE('',*,*,#16705,.F.);
#21590=ORIENTED_EDGE('',*,*,#16706,.T.);
#21591=ORIENTED_EDGE('',*,*,#16707,.F.);
#21592=ORIENTED_EDGE('',*,*,#16708,.T.);
#21593=ORIENTED_EDGE('',*,*,#16709,.F.);
#21594=ORIENTED_EDGE('',*,*,#16688,.F.);
#21595=ORIENTED_EDGE('',*,*,#16710,.T.);
#21596=ORIENTED_EDGE('',*,*,#16708,.F.);
#21597=ORIENTED_EDGE('',*,*,#16711,.T.);
#21598=ORIENTED_EDGE('',*,*,#16712,.T.);
#21599=ORIENTED_EDGE('',*,*,#16713,.F.);
#21600=ORIENTED_EDGE('',*,*,#16714,.T.);
#21601=ORIENTED_EDGE('',*,*,#16715,.F.);
#21602=ORIENTED_EDGE('',*,*,#16716,.F.);
#21603=ORIENTED_EDGE('',*,*,#16713,.T.);
#21604=ORIENTED_EDGE('',*,*,#16717,.F.);
#21605=ORIENTED_EDGE('',*,*,#16718,.T.);
#21606=ORIENTED_EDGE('',*,*,#16719,.F.);
#21607=ORIENTED_EDGE('',*,*,#16720,.F.);
#21608=ORIENTED_EDGE('',*,*,#16721,.F.);
#21609=ORIENTED_EDGE('',*,*,#16722,.T.);
#21610=ORIENTED_EDGE('',*,*,#16723,.F.);
#21611=ORIENTED_EDGE('',*,*,#16724,.F.);
#21612=ORIENTED_EDGE('',*,*,#16725,.T.);
#21613=ORIENTED_EDGE('',*,*,#16726,.F.);
#21614=ORIENTED_EDGE('',*,*,#16727,.F.);
#21615=ORIENTED_EDGE('',*,*,#16728,.F.);
#21616=ORIENTED_EDGE('',*,*,#16729,.T.);
#21617=ORIENTED_EDGE('',*,*,#16730,.F.);
#21618=ORIENTED_EDGE('',*,*,#16731,.F.);
#21619=ORIENTED_EDGE('',*,*,#16732,.T.);
#21620=ORIENTED_EDGE('',*,*,#16714,.F.);
#21621=ORIENTED_EDGE('',*,*,#16712,.F.);
#21622=ORIENTED_EDGE('',*,*,#16733,.F.);
#21623=ORIENTED_EDGE('',*,*,#16734,.T.);
#21624=ORIENTED_EDGE('',*,*,#16735,.F.);
#21625=ORIENTED_EDGE('',*,*,#16736,.F.);
#21626=ORIENTED_EDGE('',*,*,#16737,.T.);
#21627=ORIENTED_EDGE('',*,*,#16738,.F.);
#21628=ORIENTED_EDGE('',*,*,#16739,.F.);
#21629=ORIENTED_EDGE('',*,*,#16740,.F.);
#21630=ORIENTED_EDGE('',*,*,#16741,.T.);
#21631=ORIENTED_EDGE('',*,*,#16742,.F.);
#21632=ORIENTED_EDGE('',*,*,#16696,.F.);
#21633=ORIENTED_EDGE('',*,*,#16743,.T.);
#21634=ORIENTED_EDGE('',*,*,#16735,.T.);
#21635=ORIENTED_EDGE('',*,*,#16743,.F.);
#21636=ORIENTED_EDGE('',*,*,#16697,.F.);
#21637=ORIENTED_EDGE('',*,*,#16744,.T.);
#21638=ORIENTED_EDGE('',*,*,#16730,.T.);
#21639=ORIENTED_EDGE('',*,*,#16744,.F.);
#21640=ORIENTED_EDGE('',*,*,#16698,.F.);
#21641=ORIENTED_EDGE('',*,*,#16745,.T.);
#21642=ORIENTED_EDGE('',*,*,#16723,.T.);
#21643=ORIENTED_EDGE('',*,*,#16745,.F.);
#21644=ORIENTED_EDGE('',*,*,#16699,.F.);
#21645=ORIENTED_EDGE('',*,*,#16746,.T.);
#21646=ORIENTED_EDGE('',*,*,#16742,.T.);
#21647=ORIENTED_EDGE('',*,*,#16746,.F.);
#21648=ORIENTED_EDGE('',*,*,#16717,.T.);
#21649=ORIENTED_EDGE('',*,*,#16747,.T.);
#21650=ORIENTED_EDGE('',*,*,#16748,.F.);
#21651=ORIENTED_EDGE('',*,*,#16749,.F.);
#21652=ORIENTED_EDGE('',*,*,#16750,.F.);
#21653=ORIENTED_EDGE('',*,*,#16751,.F.);
#21654=ORIENTED_EDGE('',*,*,#16752,.T.);
#21655=ORIENTED_EDGE('',*,*,#16749,.T.);
#21656=ORIENTED_EDGE('',*,*,#16753,.F.);
#21657=ORIENTED_EDGE('',*,*,#16754,.T.);
#21658=ORIENTED_EDGE('',*,*,#16755,.T.);
#21659=ORIENTED_EDGE('',*,*,#16750,.T.);
#21660=ORIENTED_EDGE('',*,*,#16748,.T.);
#21661=ORIENTED_EDGE('',*,*,#16756,.T.);
#21662=ORIENTED_EDGE('',*,*,#16757,.T.);
#21663=ORIENTED_EDGE('',*,*,#16758,.T.);
#21664=ORIENTED_EDGE('',*,*,#16759,.T.);
#21665=ORIENTED_EDGE('',*,*,#16760,.T.);
#21666=ORIENTED_EDGE('',*,*,#16761,.T.);
#21667=ORIENTED_EDGE('',*,*,#16762,.T.);
#21668=ORIENTED_EDGE('',*,*,#16763,.T.);
#21669=ORIENTED_EDGE('',*,*,#16764,.T.);
#21670=ORIENTED_EDGE('',*,*,#16765,.T.);
#21671=ORIENTED_EDGE('',*,*,#16766,.T.);
#21672=ORIENTED_EDGE('',*,*,#16767,.T.);
#21673=ORIENTED_EDGE('',*,*,#16768,.T.);
#21674=ORIENTED_EDGE('',*,*,#16769,.T.);
#21675=ORIENTED_EDGE('',*,*,#16754,.F.);
#21676=ORIENTED_EDGE('',*,*,#16770,.F.);
#21677=ORIENTED_EDGE('',*,*,#16771,.F.);
#21678=ORIENTED_EDGE('',*,*,#16772,.T.);
#21679=ORIENTED_EDGE('',*,*,#16755,.F.);
#21680=ORIENTED_EDGE('',*,*,#16769,.F.);
#21681=ORIENTED_EDGE('',*,*,#16773,.F.);
#21682=ORIENTED_EDGE('',*,*,#16771,.T.);
#21683=ORIENTED_EDGE('',*,*,#16774,.F.);
#21684=ORIENTED_EDGE('',*,*,#16775,.F.);
#21685=ORIENTED_EDGE('',*,*,#16776,.F.);
#21686=ORIENTED_EDGE('',*,*,#16777,.F.);
#21687=ORIENTED_EDGE('',*,*,#16778,.F.);
#21688=ORIENTED_EDGE('',*,*,#16779,.F.);
#21689=ORIENTED_EDGE('',*,*,#16780,.F.);
#21690=ORIENTED_EDGE('',*,*,#16781,.T.);
#21691=ORIENTED_EDGE('',*,*,#16782,.F.);
#21692=ORIENTED_EDGE('',*,*,#16783,.F.);
#21693=ORIENTED_EDGE('',*,*,#16784,.F.);
#21694=ORIENTED_EDGE('',*,*,#16785,.F.);
#21695=ORIENTED_EDGE('',*,*,#16786,.F.);
#21696=ORIENTED_EDGE('',*,*,#16787,.F.);
#21697=ORIENTED_EDGE('',*,*,#16788,.F.);
#21698=ORIENTED_EDGE('',*,*,#16789,.T.);
#21699=ORIENTED_EDGE('',*,*,#16776,.T.);
#21700=ORIENTED_EDGE('',*,*,#16790,.F.);
#21701=ORIENTED_EDGE('',*,*,#16791,.F.);
#21702=ORIENTED_EDGE('',*,*,#16789,.F.);
#21703=ORIENTED_EDGE('',*,*,#16751,.T.);
#21704=ORIENTED_EDGE('',*,*,#16772,.F.);
#21705=ORIENTED_EDGE('',*,*,#16752,.F.);
#21706=ORIENTED_EDGE('',*,*,#16791,.T.);
#21707=ORIENTED_EDGE('',*,*,#16792,.T.);
#21708=ORIENTED_EDGE('',*,*,#16718,.F.);
#21709=ORIENTED_EDGE('',*,*,#16792,.F.);
#21710=ORIENTED_EDGE('',*,*,#16793,.F.);
#21711=ORIENTED_EDGE('',*,*,#16794,.T.);
#21712=ORIENTED_EDGE('',*,*,#16719,.T.);
#21713=ORIENTED_EDGE('',*,*,#16794,.F.);
#21714=ORIENTED_EDGE('',*,*,#16795,.F.);
#21715=ORIENTED_EDGE('',*,*,#16796,.T.);
#21716=ORIENTED_EDGE('',*,*,#16797,.F.);
#21717=ORIENTED_EDGE('',*,*,#16798,.T.);
#21718=ORIENTED_EDGE('',*,*,#16720,.T.);
#21719=ORIENTED_EDGE('',*,*,#16796,.F.);
#21720=ORIENTED_EDGE('',*,*,#16797,.T.);
#21721=ORIENTED_EDGE('',*,*,#16799,.F.);
#21722=ORIENTED_EDGE('',*,*,#16692,.F.);
#21723=ORIENTED_EDGE('',*,*,#16800,.T.);
#21724=ORIENTED_EDGE('',*,*,#16801,.T.);
#21725=ORIENTED_EDGE('',*,*,#16802,.T.);
#21726=ORIENTED_EDGE('',*,*,#16803,.T.);
#21727=ORIENTED_EDGE('',*,*,#16804,.T.);
#21728=ORIENTED_EDGE('',*,*,#16805,.T.);
#21729=ORIENTED_EDGE('',*,*,#16800,.F.);
#21730=ORIENTED_EDGE('',*,*,#16691,.F.);
#21731=ORIENTED_EDGE('',*,*,#16806,.T.);
#21732=ORIENTED_EDGE('',*,*,#16726,.T.);
#21733=ORIENTED_EDGE('',*,*,#16807,.F.);
#21734=ORIENTED_EDGE('',*,*,#16801,.F.);
#21735=ORIENTED_EDGE('',*,*,#16808,.T.);
#21736=ORIENTED_EDGE('',*,*,#16809,.F.);
#21737=ORIENTED_EDGE('',*,*,#16810,.T.);
#21738=ORIENTED_EDGE('',*,*,#16727,.T.);
#21739=ORIENTED_EDGE('',*,*,#16808,.F.);
#21740=ORIENTED_EDGE('',*,*,#16809,.T.);
#21741=ORIENTED_EDGE('',*,*,#16806,.F.);
#21742=ORIENTED_EDGE('',*,*,#16690,.F.);
#21743=ORIENTED_EDGE('',*,*,#16811,.T.);
#21744=ORIENTED_EDGE('',*,*,#16812,.T.);
#21745=ORIENTED_EDGE('',*,*,#16813,.T.);
#21746=ORIENTED_EDGE('',*,*,#16811,.F.);
#21747=ORIENTED_EDGE('',*,*,#16689,.F.);
#21748=ORIENTED_EDGE('',*,*,#16709,.T.);
#21749=ORIENTED_EDGE('',*,*,#16716,.T.);
#21750=ORIENTED_EDGE('',*,*,#16814,.T.);
#21751=ORIENTED_EDGE('',*,*,#16815,.T.);
#21752=ORIENTED_EDGE('',*,*,#16816,.T.);
#21753=ORIENTED_EDGE('',*,*,#16817,.F.);
#21754=ORIENTED_EDGE('',*,*,#16812,.F.);
#21755=ORIENTED_EDGE('',*,*,#16818,.T.);
#21756=ORIENTED_EDGE('',*,*,#16819,.T.);
#21757=ORIENTED_EDGE('',*,*,#16820,.F.);
#21758=ORIENTED_EDGE('',*,*,#16816,.F.);
#21759=ORIENTED_EDGE('',*,*,#16782,.T.);
#21760=ORIENTED_EDGE('',*,*,#16819,.F.);
#21761=ORIENTED_EDGE('',*,*,#16821,.T.);
#21762=ORIENTED_EDGE('',*,*,#16822,.F.);
#21763=ORIENTED_EDGE('',*,*,#16823,.T.);
#21764=ORIENTED_EDGE('',*,*,#16822,.T.);
#21765=ORIENTED_EDGE('',*,*,#16760,.F.);
#21766=ORIENTED_EDGE('',*,*,#16824,.F.);
#21767=ORIENTED_EDGE('',*,*,#16823,.F.);
#21768=ORIENTED_EDGE('',*,*,#16729,.F.);
#21769=ORIENTED_EDGE('',*,*,#16825,.T.);
#21770=ORIENTED_EDGE('',*,*,#16820,.T.);
#21771=ORIENTED_EDGE('',*,*,#16825,.F.);
#21772=ORIENTED_EDGE('',*,*,#16826,.F.);
#21773=ORIENTED_EDGE('',*,*,#16817,.T.);
#21774=ORIENTED_EDGE('',*,*,#16813,.F.);
#21775=ORIENTED_EDGE('',*,*,#16826,.T.);
#21776=ORIENTED_EDGE('',*,*,#16728,.T.);
#21777=ORIENTED_EDGE('',*,*,#16810,.F.);
#21778=ORIENTED_EDGE('',*,*,#16724,.T.);
#21779=ORIENTED_EDGE('',*,*,#16824,.T.);
#21780=ORIENTED_EDGE('',*,*,#16759,.F.);
#21781=ORIENTED_EDGE('',*,*,#16827,.F.);
#21782=ORIENTED_EDGE('',*,*,#16758,.F.);
#21783=ORIENTED_EDGE('',*,*,#16828,.F.);
#21784=ORIENTED_EDGE('',*,*,#16829,.T.);
#21785=ORIENTED_EDGE('',*,*,#16827,.T.);
#21786=ORIENTED_EDGE('',*,*,#16829,.F.);
#21787=ORIENTED_EDGE('',*,*,#16830,.T.);
#21788=ORIENTED_EDGE('',*,*,#16831,.T.);
#21789=ORIENTED_EDGE('',*,*,#16725,.F.);
#21790=ORIENTED_EDGE('',*,*,#16831,.F.);
#21791=ORIENTED_EDGE('',*,*,#16832,.F.);
#21792=ORIENTED_EDGE('',*,*,#16807,.T.);
#21793=ORIENTED_EDGE('',*,*,#16802,.F.);
#21794=ORIENTED_EDGE('',*,*,#16832,.T.);
#21795=ORIENTED_EDGE('',*,*,#16833,.T.);
#21796=ORIENTED_EDGE('',*,*,#16834,.F.);
#21797=ORIENTED_EDGE('',*,*,#16803,.F.);
#21798=ORIENTED_EDGE('',*,*,#16834,.T.);
#21799=ORIENTED_EDGE('',*,*,#16779,.T.);
#21800=ORIENTED_EDGE('',*,*,#16835,.F.);
#21801=ORIENTED_EDGE('',*,*,#16836,.T.);
#21802=ORIENTED_EDGE('',*,*,#16837,.F.);
#21803=ORIENTED_EDGE('',*,*,#16804,.F.);
#21804=ORIENTED_EDGE('',*,*,#16835,.T.);
#21805=ORIENTED_EDGE('',*,*,#16838,.T.);
#21806=ORIENTED_EDGE('',*,*,#16839,.F.);
#21807=ORIENTED_EDGE('',*,*,#16836,.F.);
#21808=ORIENTED_EDGE('',*,*,#16778,.T.);
#21809=ORIENTED_EDGE('',*,*,#16838,.F.);
#21810=ORIENTED_EDGE('',*,*,#16840,.T.);
#21811=ORIENTED_EDGE('',*,*,#16841,.F.);
#21812=ORIENTED_EDGE('',*,*,#16842,.T.);
#21813=ORIENTED_EDGE('',*,*,#16841,.T.);
#21814=ORIENTED_EDGE('',*,*,#16756,.F.);
#21815=ORIENTED_EDGE('',*,*,#16747,.F.);
#21816=ORIENTED_EDGE('',*,*,#16842,.F.);
#21817=ORIENTED_EDGE('',*,*,#16722,.F.);
#21818=ORIENTED_EDGE('',*,*,#16843,.T.);
#21819=ORIENTED_EDGE('',*,*,#16839,.T.);
#21820=ORIENTED_EDGE('',*,*,#16843,.F.);
#21821=ORIENTED_EDGE('',*,*,#16844,.F.);
#21822=ORIENTED_EDGE('',*,*,#16837,.T.);
#21823=ORIENTED_EDGE('',*,*,#16805,.F.);
#21824=ORIENTED_EDGE('',*,*,#16844,.T.);
#21825=ORIENTED_EDGE('',*,*,#16721,.T.);
#21826=ORIENTED_EDGE('',*,*,#16798,.F.);
#21827=ORIENTED_EDGE('',*,*,#16777,.T.);
#21828=ORIENTED_EDGE('',*,*,#16845,.T.);
#21829=ORIENTED_EDGE('',*,*,#16757,.F.);
#21830=ORIENTED_EDGE('',*,*,#16840,.F.);
#21831=ORIENTED_EDGE('',*,*,#16846,.F.);
#21832=ORIENTED_EDGE('',*,*,#16828,.T.);
#21833=ORIENTED_EDGE('',*,*,#16845,.F.);
#21834=ORIENTED_EDGE('',*,*,#16846,.T.);
#21835=ORIENTED_EDGE('',*,*,#16780,.T.);
#21836=ORIENTED_EDGE('',*,*,#16833,.F.);
#21837=ORIENTED_EDGE('',*,*,#16830,.F.);
#21838=ORIENTED_EDGE('',*,*,#16781,.F.);
#21839=ORIENTED_EDGE('',*,*,#16847,.T.);
#21840=ORIENTED_EDGE('',*,*,#16761,.F.);
#21841=ORIENTED_EDGE('',*,*,#16821,.F.);
#21842=ORIENTED_EDGE('',*,*,#16848,.T.);
#21843=ORIENTED_EDGE('',*,*,#16849,.T.);
#21844=ORIENTED_EDGE('',*,*,#16768,.F.);
#21845=ORIENTED_EDGE('',*,*,#16850,.F.);
#21846=ORIENTED_EDGE('',*,*,#16848,.F.);
#21847=ORIENTED_EDGE('',*,*,#16741,.F.);
#21848=ORIENTED_EDGE('',*,*,#16851,.T.);
#21849=ORIENTED_EDGE('',*,*,#16852,.T.);
#21850=ORIENTED_EDGE('',*,*,#16853,.T.);
#21851=ORIENTED_EDGE('',*,*,#16852,.F.);
#21852=ORIENTED_EDGE('',*,*,#16854,.F.);
#21853=ORIENTED_EDGE('',*,*,#16774,.T.);
#21854=ORIENTED_EDGE('',*,*,#16853,.F.);
#21855=ORIENTED_EDGE('',*,*,#16773,.T.);
#21856=ORIENTED_EDGE('',*,*,#16849,.F.);
#21857=ORIENTED_EDGE('',*,*,#16854,.T.);
#21858=ORIENTED_EDGE('',*,*,#16855,.F.);
#21859=ORIENTED_EDGE('',*,*,#16856,.F.);
#21860=ORIENTED_EDGE('',*,*,#16857,.T.);
#21861=ORIENTED_EDGE('',*,*,#16858,.F.);
#21862=ORIENTED_EDGE('',*,*,#16859,.T.);
#21863=ORIENTED_EDGE('',*,*,#16775,.T.);
#21864=ORIENTED_EDGE('',*,*,#16857,.F.);
#21865=ORIENTED_EDGE('',*,*,#16795,.T.);
#21866=ORIENTED_EDGE('',*,*,#16860,.T.);
#21867=ORIENTED_EDGE('',*,*,#16858,.T.);
#21868=ORIENTED_EDGE('',*,*,#16856,.T.);
#21869=ORIENTED_EDGE('',*,*,#16861,.T.);
#21870=ORIENTED_EDGE('',*,*,#16862,.F.);
#21871=ORIENTED_EDGE('',*,*,#16693,.F.);
#21872=ORIENTED_EDGE('',*,*,#16799,.T.);
#21873=ORIENTED_EDGE('',*,*,#16863,.T.);
#21874=ORIENTED_EDGE('',*,*,#16864,.F.);
#21875=ORIENTED_EDGE('',*,*,#16694,.F.);
#21876=ORIENTED_EDGE('',*,*,#16862,.T.);
#21877=ORIENTED_EDGE('',*,*,#16863,.F.);
#21878=ORIENTED_EDGE('',*,*,#16865,.T.);
#21879=ORIENTED_EDGE('',*,*,#16739,.T.);
#21880=ORIENTED_EDGE('',*,*,#16866,.F.);
#21881=ORIENTED_EDGE('',*,*,#16738,.T.);
#21882=ORIENTED_EDGE('',*,*,#16867,.F.);
#21883=ORIENTED_EDGE('',*,*,#16868,.F.);
#21884=ORIENTED_EDGE('',*,*,#16866,.T.);
#21885=ORIENTED_EDGE('',*,*,#16868,.T.);
#21886=ORIENTED_EDGE('',*,*,#16869,.T.);
#21887=ORIENTED_EDGE('',*,*,#16870,.T.);
#21888=ORIENTED_EDGE('',*,*,#16871,.T.);
#21889=ORIENTED_EDGE('',*,*,#16872,.T.);
#21890=ORIENTED_EDGE('',*,*,#16710,.F.);
#21891=ORIENTED_EDGE('',*,*,#16695,.F.);
#21892=ORIENTED_EDGE('',*,*,#16864,.T.);
#21893=ORIENTED_EDGE('',*,*,#16872,.F.);
#21894=ORIENTED_EDGE('',*,*,#16873,.T.);
#21895=ORIENTED_EDGE('',*,*,#16733,.T.);
#21896=ORIENTED_EDGE('',*,*,#16711,.F.);
#21897=ORIENTED_EDGE('',*,*,#16874,.F.);
#21898=ORIENTED_EDGE('',*,*,#16873,.F.);
#21899=ORIENTED_EDGE('',*,*,#16875,.T.);
#21900=ORIENTED_EDGE('',*,*,#16876,.F.);
#21901=ORIENTED_EDGE('',*,*,#16734,.F.);
#21902=ORIENTED_EDGE('',*,*,#16874,.T.);
#21903=ORIENTED_EDGE('',*,*,#16877,.T.);
#21904=ORIENTED_EDGE('',*,*,#16876,.T.);
#21905=ORIENTED_EDGE('',*,*,#16878,.T.);
#21906=ORIENTED_EDGE('',*,*,#16764,.F.);
#21907=ORIENTED_EDGE('',*,*,#16879,.F.);
#21908=ORIENTED_EDGE('',*,*,#16731,.T.);
#21909=ORIENTED_EDGE('',*,*,#16879,.T.);
#21910=ORIENTED_EDGE('',*,*,#16763,.F.);
#21911=ORIENTED_EDGE('',*,*,#16880,.F.);
#21912=ORIENTED_EDGE('',*,*,#16762,.F.);
#21913=ORIENTED_EDGE('',*,*,#16881,.F.);
#21914=ORIENTED_EDGE('',*,*,#16882,.T.);
#21915=ORIENTED_EDGE('',*,*,#16880,.T.);
#21916=ORIENTED_EDGE('',*,*,#16882,.F.);
#21917=ORIENTED_EDGE('',*,*,#16883,.T.);
#21918=ORIENTED_EDGE('',*,*,#16884,.T.);
#21919=ORIENTED_EDGE('',*,*,#16732,.F.);
#21920=ORIENTED_EDGE('',*,*,#16884,.F.);
#21921=ORIENTED_EDGE('',*,*,#16885,.F.);
#21922=ORIENTED_EDGE('',*,*,#16715,.T.);
#21923=ORIENTED_EDGE('',*,*,#16814,.F.);
#21924=ORIENTED_EDGE('',*,*,#16885,.T.);
#21925=ORIENTED_EDGE('',*,*,#16886,.T.);
#21926=ORIENTED_EDGE('',*,*,#16887,.F.);
#21927=ORIENTED_EDGE('',*,*,#16815,.F.);
#21928=ORIENTED_EDGE('',*,*,#16887,.T.);
#21929=ORIENTED_EDGE('',*,*,#16783,.T.);
#21930=ORIENTED_EDGE('',*,*,#16818,.F.);
#21931=ORIENTED_EDGE('',*,*,#16888,.T.);
#21932=ORIENTED_EDGE('',*,*,#16784,.T.);
#21933=ORIENTED_EDGE('',*,*,#16886,.F.);
#21934=ORIENTED_EDGE('',*,*,#16883,.F.);
#21935=ORIENTED_EDGE('',*,*,#16888,.F.);
#21936=ORIENTED_EDGE('',*,*,#16881,.T.);
#21937=ORIENTED_EDGE('',*,*,#16847,.F.);
#21938=ORIENTED_EDGE('',*,*,#16889,.F.);
#21939=ORIENTED_EDGE('',*,*,#16890,.T.);
#21940=ORIENTED_EDGE('',*,*,#16878,.F.);
#21941=ORIENTED_EDGE('',*,*,#16889,.T.);
#21942=ORIENTED_EDGE('',*,*,#16877,.F.);
#21943=ORIENTED_EDGE('',*,*,#16891,.F.);
#21944=ORIENTED_EDGE('',*,*,#16786,.T.);
#21945=ORIENTED_EDGE('',*,*,#16891,.T.);
#21946=ORIENTED_EDGE('',*,*,#16875,.F.);
#21947=ORIENTED_EDGE('',*,*,#16871,.F.);
#21948=ORIENTED_EDGE('',*,*,#16892,.T.);
#21949=ORIENTED_EDGE('',*,*,#16870,.F.);
#21950=ORIENTED_EDGE('',*,*,#16893,.T.);
#21951=ORIENTED_EDGE('',*,*,#16787,.T.);
#21952=ORIENTED_EDGE('',*,*,#16892,.F.);
#21953=ORIENTED_EDGE('',*,*,#16869,.F.);
#21954=ORIENTED_EDGE('',*,*,#16894,.T.);
#21955=ORIENTED_EDGE('',*,*,#16895,.T.);
#21956=ORIENTED_EDGE('',*,*,#16893,.F.);
#21957=ORIENTED_EDGE('',*,*,#16896,.T.);
#21958=ORIENTED_EDGE('',*,*,#16788,.T.);
#21959=ORIENTED_EDGE('',*,*,#16895,.F.);
#21960=ORIENTED_EDGE('',*,*,#16897,.F.);
#21961=ORIENTED_EDGE('',*,*,#16896,.F.);
#21962=ORIENTED_EDGE('',*,*,#16898,.T.);
#21963=ORIENTED_EDGE('',*,*,#16899,.F.);
#21964=ORIENTED_EDGE('',*,*,#16765,.F.);
#21965=ORIENTED_EDGE('',*,*,#16890,.F.);
#21966=ORIENTED_EDGE('',*,*,#16785,.T.);
#21967=ORIENTED_EDGE('',*,*,#16899,.T.);
#21968=ORIENTED_EDGE('',*,*,#16766,.F.);
#21969=ORIENTED_EDGE('',*,*,#16898,.F.);
#21970=ORIENTED_EDGE('',*,*,#16900,.T.);
#21971=ORIENTED_EDGE('',*,*,#16901,.T.);
#21972=ORIENTED_EDGE('',*,*,#16736,.T.);
#21973=ORIENTED_EDGE('',*,*,#16850,.T.);
#21974=ORIENTED_EDGE('',*,*,#16767,.F.);
#21975=ORIENTED_EDGE('',*,*,#16901,.F.);
#21976=ORIENTED_EDGE('',*,*,#16900,.F.);
#21977=ORIENTED_EDGE('',*,*,#16897,.T.);
#21978=ORIENTED_EDGE('',*,*,#16902,.T.);
#21979=ORIENTED_EDGE('',*,*,#16737,.F.);
#21980=ORIENTED_EDGE('',*,*,#16902,.F.);
#21981=ORIENTED_EDGE('',*,*,#16894,.F.);
#21982=ORIENTED_EDGE('',*,*,#16867,.T.);
#21983=ORIENTED_EDGE('',*,*,#16861,.F.);
#21984=ORIENTED_EDGE('',*,*,#16903,.T.);
#21985=ORIENTED_EDGE('',*,*,#16740,.T.);
#21986=ORIENTED_EDGE('',*,*,#16865,.F.);
#21987=ORIENTED_EDGE('',*,*,#16851,.F.);
#21988=ORIENTED_EDGE('',*,*,#16903,.F.);
#21989=ORIENTED_EDGE('',*,*,#16855,.T.);
#21990=ORIENTED_EDGE('',*,*,#16860,.F.);
#21991=ORIENTED_EDGE('',*,*,#16793,.T.);
#21992=ORIENTED_EDGE('',*,*,#16790,.T.);
#21993=ORIENTED_EDGE('',*,*,#16859,.F.);
#21994=ORIENTED_EDGE('',*,*,#16904,.F.);
#21995=ORIENTED_EDGE('',*,*,#16905,.T.);
#21996=ORIENTED_EDGE('',*,*,#16770,.T.);
#21997=ORIENTED_EDGE('',*,*,#16753,.T.);
#21998=ORIENTED_EDGE('',*,*,#16905,.F.);
#21999=ORIENTED_EDGE('',*,*,#16904,.T.);
#22000=ORIENTED_EDGE('',*,*,#16906,.T.);
#22001=ORIENTED_EDGE('',*,*,#16907,.F.);
#22002=ORIENTED_EDGE('',*,*,#16908,.F.);
#22003=ORIENTED_EDGE('',*,*,#16909,.T.);
#22004=ORIENTED_EDGE('',*,*,#16906,.F.);
#22005=ORIENTED_EDGE('',*,*,#16909,.F.);
#22006=ORIENTED_EDGE('',*,*,#16910,.T.);
#22007=ORIENTED_EDGE('',*,*,#16911,.T.);
#22008=ORIENTED_EDGE('',*,*,#16907,.T.);
#22009=ORIENTED_EDGE('',*,*,#16908,.T.);
#22010=ORIENTED_EDGE('',*,*,#16911,.F.);
#22011=ORIENTED_EDGE('',*,*,#16910,.F.);
#22012=ORIENTED_EDGE('',*,*,#16912,.T.);
#22013=ORIENTED_EDGE('',*,*,#16913,.T.);
#22014=ORIENTED_EDGE('',*,*,#16914,.T.);
#22015=ORIENTED_EDGE('',*,*,#16912,.F.);
#22016=ORIENTED_EDGE('',*,*,#16914,.F.);
#22017=ORIENTED_EDGE('',*,*,#16913,.F.);
#22018=ORIENTED_EDGE('',*,*,#16915,.T.);
#22019=ORIENTED_EDGE('',*,*,#16916,.T.);
#22020=ORIENTED_EDGE('',*,*,#16917,.T.);
#22021=ORIENTED_EDGE('',*,*,#16915,.F.);
#22022=ORIENTED_EDGE('',*,*,#16917,.F.);
#22023=ORIENTED_EDGE('',*,*,#16916,.F.);
#22024=ORIENTED_EDGE('',*,*,#16918,.T.);
#22025=ORIENTED_EDGE('',*,*,#16919,.T.);
#22026=ORIENTED_EDGE('',*,*,#16920,.T.);
#22027=ORIENTED_EDGE('',*,*,#16918,.F.);
#22028=ORIENTED_EDGE('',*,*,#16920,.F.);
#22029=ORIENTED_EDGE('',*,*,#16921,.T.);
#22030=ORIENTED_EDGE('',*,*,#16919,.F.);
#22031=ORIENTED_EDGE('',*,*,#16922,.T.);
#22032=ORIENTED_EDGE('',*,*,#16923,.T.);
#22033=ORIENTED_EDGE('',*,*,#16921,.F.);
#22034=ORIENTED_EDGE('',*,*,#16923,.F.);
#22035=ORIENTED_EDGE('',*,*,#16924,.T.);
#22036=ORIENTED_EDGE('',*,*,#16922,.F.);
#22037=ORIENTED_EDGE('',*,*,#16925,.T.);
#22038=ORIENTED_EDGE('',*,*,#16926,.T.);
#22039=ORIENTED_EDGE('',*,*,#16924,.F.);
#22040=ORIENTED_EDGE('',*,*,#16926,.F.);
#22041=ORIENTED_EDGE('',*,*,#16927,.T.);
#22042=ORIENTED_EDGE('',*,*,#16925,.F.);
#22043=ORIENTED_EDGE('',*,*,#16928,.F.);
#22044=ORIENTED_EDGE('',*,*,#16929,.T.);
#22045=ORIENTED_EDGE('',*,*,#16927,.F.);
#22046=ORIENTED_EDGE('',*,*,#16929,.F.);
#22047=ORIENTED_EDGE('',*,*,#16930,.T.);
#22048=ORIENTED_EDGE('',*,*,#16931,.T.);
#22049=ORIENTED_EDGE('',*,*,#16932,.T.);
#22050=ORIENTED_EDGE('',*,*,#16933,.T.);
#22051=ORIENTED_EDGE('',*,*,#16934,.T.);
#22052=ORIENTED_EDGE('',*,*,#16935,.T.);
#22053=ORIENTED_EDGE('',*,*,#16936,.T.);
#22054=ORIENTED_EDGE('',*,*,#16937,.T.);
#22055=ORIENTED_EDGE('',*,*,#16928,.T.);
#22056=ORIENTED_EDGE('',*,*,#16700,.F.);
#22057=ORIENTED_EDGE('',*,*,#16938,.T.);
#22058=ORIENTED_EDGE('',*,*,#16930,.F.);
#22059=ORIENTED_EDGE('',*,*,#16939,.F.);
#22060=ORIENTED_EDGE('',*,*,#16701,.T.);
#22061=ORIENTED_EDGE('',*,*,#16939,.T.);
#22062=ORIENTED_EDGE('',*,*,#16937,.F.);
#22063=ORIENTED_EDGE('',*,*,#16940,.F.);
#22064=ORIENTED_EDGE('',*,*,#16702,.F.);
#22065=ORIENTED_EDGE('',*,*,#16940,.T.);
#22066=ORIENTED_EDGE('',*,*,#16936,.F.);
#22067=ORIENTED_EDGE('',*,*,#16941,.F.);
#22068=ORIENTED_EDGE('',*,*,#16703,.T.);
#22069=ORIENTED_EDGE('',*,*,#16941,.T.);
#22070=ORIENTED_EDGE('',*,*,#16935,.F.);
#22071=ORIENTED_EDGE('',*,*,#16942,.F.);
#22072=ORIENTED_EDGE('',*,*,#16704,.F.);
#22073=ORIENTED_EDGE('',*,*,#16942,.T.);
#22074=ORIENTED_EDGE('',*,*,#16934,.F.);
#22075=ORIENTED_EDGE('',*,*,#16943,.F.);
#22076=ORIENTED_EDGE('',*,*,#16705,.T.);
#22077=ORIENTED_EDGE('',*,*,#16943,.T.);
#22078=ORIENTED_EDGE('',*,*,#16933,.F.);
#22079=ORIENTED_EDGE('',*,*,#16944,.F.);
#22080=ORIENTED_EDGE('',*,*,#16706,.F.);
#22081=ORIENTED_EDGE('',*,*,#16944,.T.);
#22082=ORIENTED_EDGE('',*,*,#16932,.F.);
#22083=ORIENTED_EDGE('',*,*,#16945,.F.);
#22084=ORIENTED_EDGE('',*,*,#16707,.T.);
#22085=ORIENTED_EDGE('',*,*,#16945,.T.);
#22086=ORIENTED_EDGE('',*,*,#16931,.F.);
#22087=ORIENTED_EDGE('',*,*,#16938,.F.);
#22088=ORIENTED_EDGE('',*,*,#16946,.T.);
#22089=ORIENTED_EDGE('',*,*,#16947,.T.);
#22090=ORIENTED_EDGE('',*,*,#16948,.T.);
#22091=ORIENTED_EDGE('',*,*,#16949,.T.);
#22092=ORIENTED_EDGE('',*,*,#16948,.F.);
#22093=ORIENTED_EDGE('',*,*,#16950,.F.);
#22094=ORIENTED_EDGE('',*,*,#16951,.F.);
#22095=ORIENTED_EDGE('',*,*,#16952,.T.);
#22096=ORIENTED_EDGE('',*,*,#16946,.F.);
#22097=ORIENTED_EDGE('',*,*,#16947,.F.);
#22098=ORIENTED_EDGE('',*,*,#16952,.F.);
#22099=ORIENTED_EDGE('',*,*,#16953,.T.);
#22100=ORIENTED_EDGE('',*,*,#16949,.F.);
#22101=ORIENTED_EDGE('',*,*,#16950,.T.);
#22102=ORIENTED_EDGE('',*,*,#16951,.T.);
#22103=ORIENTED_EDGE('',*,*,#16954,.T.);
#22104=ORIENTED_EDGE('',*,*,#16955,.T.);
#22105=ORIENTED_EDGE('',*,*,#16954,.F.);
#22106=ORIENTED_EDGE('',*,*,#16955,.F.);
#22107=ORIENTED_EDGE('',*,*,#16956,.T.);
#22108=ORIENTED_EDGE('',*,*,#16957,.T.);
#22109=ORIENTED_EDGE('',*,*,#16958,.T.);
#22110=ORIENTED_EDGE('',*,*,#16959,.T.);
#22111=ORIENTED_EDGE('',*,*,#16958,.F.);
#22112=ORIENTED_EDGE('',*,*,#16959,.F.);
#22113=ORIENTED_EDGE('',*,*,#16960,.T.);
#22114=ORIENTED_EDGE('',*,*,#16961,.T.);
#22115=ORIENTED_EDGE('',*,*,#16962,.T.);
#22116=ORIENTED_EDGE('',*,*,#16963,.T.);
#22117=ORIENTED_EDGE('',*,*,#16964,.T.);
#22118=ORIENTED_EDGE('',*,*,#16965,.T.);
#22119=ORIENTED_EDGE('',*,*,#16953,.F.);
#22120=ORIENTED_EDGE('',*,*,#16966,.T.);
#22121=ORIENTED_EDGE('',*,*,#16956,.F.);
#22122=ORIENTED_EDGE('',*,*,#16957,.F.);
#22123=ORIENTED_EDGE('',*,*,#16966,.F.);
#22124=ORIENTED_EDGE('',*,*,#16967,.F.);
#22125=ORIENTED_EDGE('',*,*,#16968,.T.);
#22126=ORIENTED_EDGE('',*,*,#16964,.F.);
#22127=ORIENTED_EDGE('',*,*,#16969,.F.);
#22128=ORIENTED_EDGE('',*,*,#16970,.F.);
#22129=ORIENTED_EDGE('',*,*,#16971,.T.);
#22130=ORIENTED_EDGE('',*,*,#16965,.F.);
#22131=ORIENTED_EDGE('',*,*,#16968,.F.);
#22132=ORIENTED_EDGE('',*,*,#16972,.F.);
#22133=ORIENTED_EDGE('',*,*,#16973,.T.);
#22134=ORIENTED_EDGE('',*,*,#16960,.F.);
#22135=ORIENTED_EDGE('',*,*,#16971,.F.);
#22136=ORIENTED_EDGE('',*,*,#16974,.F.);
#22137=ORIENTED_EDGE('',*,*,#16975,.F.);
#22138=ORIENTED_EDGE('',*,*,#16961,.F.);
#22139=ORIENTED_EDGE('',*,*,#16973,.F.);
#22140=ORIENTED_EDGE('',*,*,#16976,.F.);
#22141=ORIENTED_EDGE('',*,*,#16969,.T.);
#22142=ORIENTED_EDGE('',*,*,#16963,.F.);
#22143=ORIENTED_EDGE('',*,*,#16977,.F.);
#22144=ORIENTED_EDGE('',*,*,#16978,.F.);
#22145=ORIENTED_EDGE('',*,*,#16979,.F.);
#22146=ORIENTED_EDGE('',*,*,#16977,.T.);
#22147=ORIENTED_EDGE('',*,*,#16962,.F.);
#22148=ORIENTED_EDGE('',*,*,#16975,.T.);
#22149=ORIENTED_EDGE('',*,*,#16980,.T.);
#22150=ORIENTED_EDGE('',*,*,#16978,.T.);
#22151=ORIENTED_EDGE('',*,*,#16979,.T.);
#22152=ORIENTED_EDGE('',*,*,#16974,.T.);
#22153=ORIENTED_EDGE('',*,*,#16972,.T.);
#22154=ORIENTED_EDGE('',*,*,#16970,.T.);
#22155=ORIENTED_EDGE('',*,*,#16967,.T.);
#22156=ORIENTED_EDGE('',*,*,#16976,.T.);
#22157=ORIENTED_EDGE('',*,*,#16980,.F.);
#22158=ORIENTED_EDGE('',*,*,#16981,.T.);
#22159=ORIENTED_EDGE('',*,*,#16982,.T.);
#22160=ORIENTED_EDGE('',*,*,#16983,.T.);
#22161=ORIENTED_EDGE('',*,*,#16984,.T.);
#22162=ORIENTED_EDGE('',*,*,#16983,.F.);
#22163=ORIENTED_EDGE('',*,*,#16985,.F.);
#22164=ORIENTED_EDGE('',*,*,#16986,.F.);
#22165=ORIENTED_EDGE('',*,*,#16987,.T.);
#22166=ORIENTED_EDGE('',*,*,#16981,.F.);
#22167=ORIENTED_EDGE('',*,*,#16982,.F.);
#22168=ORIENTED_EDGE('',*,*,#16987,.F.);
#22169=ORIENTED_EDGE('',*,*,#16988,.T.);
#22170=ORIENTED_EDGE('',*,*,#16984,.F.);
#22171=ORIENTED_EDGE('',*,*,#16985,.T.);
#22172=ORIENTED_EDGE('',*,*,#16986,.T.);
#22173=ORIENTED_EDGE('',*,*,#16989,.T.);
#22174=ORIENTED_EDGE('',*,*,#16990,.T.);
#22175=ORIENTED_EDGE('',*,*,#16989,.F.);
#22176=ORIENTED_EDGE('',*,*,#16990,.F.);
#22177=ORIENTED_EDGE('',*,*,#16991,.T.);
#22178=ORIENTED_EDGE('',*,*,#16992,.T.);
#22179=ORIENTED_EDGE('',*,*,#16993,.T.);
#22180=ORIENTED_EDGE('',*,*,#16994,.T.);
#22181=ORIENTED_EDGE('',*,*,#16993,.F.);
#22182=ORIENTED_EDGE('',*,*,#16994,.F.);
#22183=ORIENTED_EDGE('',*,*,#16995,.T.);
#22184=ORIENTED_EDGE('',*,*,#16996,.T.);
#22185=ORIENTED_EDGE('',*,*,#16997,.T.);
#22186=ORIENTED_EDGE('',*,*,#16998,.T.);
#22187=ORIENTED_EDGE('',*,*,#16999,.T.);
#22188=ORIENTED_EDGE('',*,*,#17000,.T.);
#22189=ORIENTED_EDGE('',*,*,#16988,.F.);
#22190=ORIENTED_EDGE('',*,*,#17001,.T.);
#22191=ORIENTED_EDGE('',*,*,#16991,.F.);
#22192=ORIENTED_EDGE('',*,*,#16992,.F.);
#22193=ORIENTED_EDGE('',*,*,#17001,.F.);
#22194=ORIENTED_EDGE('',*,*,#17002,.F.);
#22195=ORIENTED_EDGE('',*,*,#17003,.T.);
#22196=ORIENTED_EDGE('',*,*,#16999,.F.);
#22197=ORIENTED_EDGE('',*,*,#17004,.F.);
#22198=ORIENTED_EDGE('',*,*,#17005,.F.);
#22199=ORIENTED_EDGE('',*,*,#17006,.T.);
#22200=ORIENTED_EDGE('',*,*,#17000,.F.);
#22201=ORIENTED_EDGE('',*,*,#17003,.F.);
#22202=ORIENTED_EDGE('',*,*,#17007,.F.);
#22203=ORIENTED_EDGE('',*,*,#17008,.T.);
#22204=ORIENTED_EDGE('',*,*,#16995,.F.);
#22205=ORIENTED_EDGE('',*,*,#17006,.F.);
#22206=ORIENTED_EDGE('',*,*,#17009,.F.);
#22207=ORIENTED_EDGE('',*,*,#17010,.F.);
#22208=ORIENTED_EDGE('',*,*,#16996,.F.);
#22209=ORIENTED_EDGE('',*,*,#17008,.F.);
#22210=ORIENTED_EDGE('',*,*,#17011,.F.);
#22211=ORIENTED_EDGE('',*,*,#17004,.T.);
#22212=ORIENTED_EDGE('',*,*,#16998,.F.);
#22213=ORIENTED_EDGE('',*,*,#17012,.F.);
#22214=ORIENTED_EDGE('',*,*,#17013,.F.);
#22215=ORIENTED_EDGE('',*,*,#17014,.F.);
#22216=ORIENTED_EDGE('',*,*,#17012,.T.);
#22217=ORIENTED_EDGE('',*,*,#16997,.F.);
#22218=ORIENTED_EDGE('',*,*,#17010,.T.);
#22219=ORIENTED_EDGE('',*,*,#17015,.T.);
#22220=ORIENTED_EDGE('',*,*,#17013,.T.);
#22221=ORIENTED_EDGE('',*,*,#17014,.T.);
#22222=ORIENTED_EDGE('',*,*,#17009,.T.);
#22223=ORIENTED_EDGE('',*,*,#17007,.T.);
#22224=ORIENTED_EDGE('',*,*,#17005,.T.);
#22225=ORIENTED_EDGE('',*,*,#17002,.T.);
#22226=ORIENTED_EDGE('',*,*,#17011,.T.);
#22227=ORIENTED_EDGE('',*,*,#17015,.F.);
#22228=ORIENTED_EDGE('',*,*,#17016,.T.);
#22229=ORIENTED_EDGE('',*,*,#17017,.T.);
#22230=ORIENTED_EDGE('',*,*,#17018,.T.);
#22231=ORIENTED_EDGE('',*,*,#17019,.T.);
#22232=ORIENTED_EDGE('',*,*,#17018,.F.);
#22233=ORIENTED_EDGE('',*,*,#17020,.F.);
#22234=ORIENTED_EDGE('',*,*,#17021,.F.);
#22235=ORIENTED_EDGE('',*,*,#17022,.T.);
#22236=ORIENTED_EDGE('',*,*,#17016,.F.);
#22237=ORIENTED_EDGE('',*,*,#17017,.F.);
#22238=ORIENTED_EDGE('',*,*,#17022,.F.);
#22239=ORIENTED_EDGE('',*,*,#17023,.T.);
#22240=ORIENTED_EDGE('',*,*,#17019,.F.);
#22241=ORIENTED_EDGE('',*,*,#17020,.T.);
#22242=ORIENTED_EDGE('',*,*,#17021,.T.);
#22243=ORIENTED_EDGE('',*,*,#17024,.T.);
#22244=ORIENTED_EDGE('',*,*,#17025,.T.);
#22245=ORIENTED_EDGE('',*,*,#17024,.F.);
#22246=ORIENTED_EDGE('',*,*,#17025,.F.);
#22247=ORIENTED_EDGE('',*,*,#17026,.T.);
#22248=ORIENTED_EDGE('',*,*,#17027,.T.);
#22249=ORIENTED_EDGE('',*,*,#17028,.T.);
#22250=ORIENTED_EDGE('',*,*,#17029,.T.);
#22251=ORIENTED_EDGE('',*,*,#17028,.F.);
#22252=ORIENTED_EDGE('',*,*,#17029,.F.);
#22253=ORIENTED_EDGE('',*,*,#17030,.T.);
#22254=ORIENTED_EDGE('',*,*,#17031,.T.);
#22255=ORIENTED_EDGE('',*,*,#17032,.T.);
#22256=ORIENTED_EDGE('',*,*,#17033,.T.);
#22257=ORIENTED_EDGE('',*,*,#17034,.T.);
#22258=ORIENTED_EDGE('',*,*,#17035,.T.);
#22259=ORIENTED_EDGE('',*,*,#17023,.F.);
#22260=ORIENTED_EDGE('',*,*,#17036,.T.);
#22261=ORIENTED_EDGE('',*,*,#17026,.F.);
#22262=ORIENTED_EDGE('',*,*,#17027,.F.);
#22263=ORIENTED_EDGE('',*,*,#17036,.F.);
#22264=ORIENTED_EDGE('',*,*,#17037,.F.);
#22265=ORIENTED_EDGE('',*,*,#17038,.T.);
#22266=ORIENTED_EDGE('',*,*,#17034,.F.);
#22267=ORIENTED_EDGE('',*,*,#17039,.F.);
#22268=ORIENTED_EDGE('',*,*,#17040,.F.);
#22269=ORIENTED_EDGE('',*,*,#17041,.T.);
#22270=ORIENTED_EDGE('',*,*,#17035,.F.);
#22271=ORIENTED_EDGE('',*,*,#17038,.F.);
#22272=ORIENTED_EDGE('',*,*,#17042,.F.);
#22273=ORIENTED_EDGE('',*,*,#17043,.T.);
#22274=ORIENTED_EDGE('',*,*,#17030,.F.);
#22275=ORIENTED_EDGE('',*,*,#17041,.F.);
#22276=ORIENTED_EDGE('',*,*,#17044,.F.);
#22277=ORIENTED_EDGE('',*,*,#17045,.F.);
#22278=ORIENTED_EDGE('',*,*,#17031,.F.);
#22279=ORIENTED_EDGE('',*,*,#17043,.F.);
#22280=ORIENTED_EDGE('',*,*,#17046,.F.);
#22281=ORIENTED_EDGE('',*,*,#17039,.T.);
#22282=ORIENTED_EDGE('',*,*,#17033,.F.);
#22283=ORIENTED_EDGE('',*,*,#17047,.F.);
#22284=ORIENTED_EDGE('',*,*,#17048,.F.);
#22285=ORIENTED_EDGE('',*,*,#17049,.F.);
#22286=ORIENTED_EDGE('',*,*,#17047,.T.);
#22287=ORIENTED_EDGE('',*,*,#17032,.F.);
#22288=ORIENTED_EDGE('',*,*,#17045,.T.);
#22289=ORIENTED_EDGE('',*,*,#17050,.T.);
#22290=ORIENTED_EDGE('',*,*,#17048,.T.);
#22291=ORIENTED_EDGE('',*,*,#17049,.T.);
#22292=ORIENTED_EDGE('',*,*,#17044,.T.);
#22293=ORIENTED_EDGE('',*,*,#17042,.T.);
#22294=ORIENTED_EDGE('',*,*,#17040,.T.);
#22295=ORIENTED_EDGE('',*,*,#17037,.T.);
#22296=ORIENTED_EDGE('',*,*,#17046,.T.);
#22297=ORIENTED_EDGE('',*,*,#17050,.F.);
#22298=ORIENTED_EDGE('',*,*,#17051,.T.);
#22299=ORIENTED_EDGE('',*,*,#17052,.T.);
#22300=ORIENTED_EDGE('',*,*,#17053,.T.);
#22301=ORIENTED_EDGE('',*,*,#17054,.T.);
#22302=ORIENTED_EDGE('',*,*,#17053,.F.);
#22303=ORIENTED_EDGE('',*,*,#17055,.F.);
#22304=ORIENTED_EDGE('',*,*,#17056,.F.);
#22305=ORIENTED_EDGE('',*,*,#17057,.T.);
#22306=ORIENTED_EDGE('',*,*,#17051,.F.);
#22307=ORIENTED_EDGE('',*,*,#17052,.F.);
#22308=ORIENTED_EDGE('',*,*,#17057,.F.);
#22309=ORIENTED_EDGE('',*,*,#17058,.T.);
#22310=ORIENTED_EDGE('',*,*,#17054,.F.);
#22311=ORIENTED_EDGE('',*,*,#17055,.T.);
#22312=ORIENTED_EDGE('',*,*,#17056,.T.);
#22313=ORIENTED_EDGE('',*,*,#17059,.T.);
#22314=ORIENTED_EDGE('',*,*,#17060,.T.);
#22315=ORIENTED_EDGE('',*,*,#17059,.F.);
#22316=ORIENTED_EDGE('',*,*,#17060,.F.);
#22317=ORIENTED_EDGE('',*,*,#17061,.F.);
#22318=ORIENTED_EDGE('',*,*,#17062,.F.);
#22319=ORIENTED_EDGE('',*,*,#17063,.F.);
#22320=ORIENTED_EDGE('',*,*,#17064,.F.);
#22321=ORIENTED_EDGE('',*,*,#17065,.F.);
#22322=ORIENTED_EDGE('',*,*,#17066,.F.);
#22323=ORIENTED_EDGE('',*,*,#17067,.F.);
#22324=ORIENTED_EDGE('',*,*,#17068,.F.);
#22325=ORIENTED_EDGE('',*,*,#17069,.F.);
#22326=ORIENTED_EDGE('',*,*,#17070,.F.);
#22327=ORIENTED_EDGE('',*,*,#17071,.F.);
#22328=ORIENTED_EDGE('',*,*,#17072,.F.);
#22329=ORIENTED_EDGE('',*,*,#17073,.F.);
#22330=ORIENTED_EDGE('',*,*,#17074,.F.);
#22331=ORIENTED_EDGE('',*,*,#17075,.F.);
#22332=ORIENTED_EDGE('',*,*,#17076,.F.);
#22333=ORIENTED_EDGE('',*,*,#17077,.F.);
#22334=ORIENTED_EDGE('',*,*,#17078,.F.);
#22335=ORIENTED_EDGE('',*,*,#17076,.T.);
#22336=ORIENTED_EDGE('',*,*,#17073,.T.);
#22337=ORIENTED_EDGE('',*,*,#17079,.F.);
#22338=ORIENTED_EDGE('',*,*,#17080,.F.);
#22339=ORIENTED_EDGE('',*,*,#17081,.T.);
#22340=ORIENTED_EDGE('',*,*,#17075,.T.);
#22341=ORIENTED_EDGE('',*,*,#17067,.T.);
#22342=ORIENTED_EDGE('',*,*,#17082,.F.);
#22343=ORIENTED_EDGE('',*,*,#17083,.F.);
#22344=ORIENTED_EDGE('',*,*,#17079,.T.);
#22345=ORIENTED_EDGE('',*,*,#17069,.T.);
#22346=ORIENTED_EDGE('',*,*,#17061,.T.);
#22347=ORIENTED_EDGE('',*,*,#17084,.F.);
#22348=ORIENTED_EDGE('',*,*,#17085,.F.);
#22349=ORIENTED_EDGE('',*,*,#17082,.T.);
#22350=ORIENTED_EDGE('',*,*,#17085,.T.);
#22351=ORIENTED_EDGE('',*,*,#17086,.T.);
#22352=ORIENTED_EDGE('',*,*,#17087,.T.);
#22353=ORIENTED_EDGE('',*,*,#17088,.T.);
#22354=ORIENTED_EDGE('',*,*,#17080,.T.);
#22355=ORIENTED_EDGE('',*,*,#17083,.T.);
#22356=ORIENTED_EDGE('',*,*,#17089,.F.);
#22357=ORIENTED_EDGE('',*,*,#17065,.T.);
#22358=ORIENTED_EDGE('',*,*,#17090,.F.);
#22359=ORIENTED_EDGE('',*,*,#17086,.F.);
#22360=ORIENTED_EDGE('',*,*,#17084,.T.);
#22361=ORIENTED_EDGE('',*,*,#17063,.T.);
#22362=ORIENTED_EDGE('',*,*,#17071,.T.);
#22363=ORIENTED_EDGE('',*,*,#17091,.F.);
#22364=ORIENTED_EDGE('',*,*,#17087,.F.);
#22365=ORIENTED_EDGE('',*,*,#17090,.T.);
#22366=ORIENTED_EDGE('',*,*,#17064,.T.);
#22367=ORIENTED_EDGE('',*,*,#17077,.T.);
#22368=ORIENTED_EDGE('',*,*,#17081,.F.);
#22369=ORIENTED_EDGE('',*,*,#17088,.F.);
#22370=ORIENTED_EDGE('',*,*,#17091,.T.);
#22371=ORIENTED_EDGE('',*,*,#17070,.T.);
#22372=ORIENTED_EDGE('',*,*,#17062,.T.);
#22373=ORIENTED_EDGE('',*,*,#17068,.T.);
#22374=ORIENTED_EDGE('',*,*,#17074,.T.);
#22375=ORIENTED_EDGE('',*,*,#17078,.T.);
#22376=ORIENTED_EDGE('',*,*,#17072,.T.);
#22377=ORIENTED_EDGE('',*,*,#17066,.T.);
#22378=ORIENTED_EDGE('',*,*,#17058,.F.);
#22379=ORIENTED_EDGE('',*,*,#17092,.T.);
#22380=ORIENTED_EDGE('',*,*,#17089,.T.);
#22381=ORIENTED_EDGE('',*,*,#17092,.F.);
#22382=ORIENTED_EDGE('',*,*,#17093,.F.);
#22383=ORIENTED_EDGE('',*,*,#17094,.F.);
#22384=ORIENTED_EDGE('',*,*,#17095,.F.);
#22385=ORIENTED_EDGE('',*,*,#17096,.T.);
#22386=ORIENTED_EDGE('',*,*,#17097,.F.);
#22387=ORIENTED_EDGE('',*,*,#17096,.F.);
#22388=ORIENTED_EDGE('',*,*,#17098,.F.);
#22389=ORIENTED_EDGE('',*,*,#17099,.T.);
#22390=ORIENTED_EDGE('',*,*,#17100,.F.);
#22391=ORIENTED_EDGE('',*,*,#17099,.F.);
#22392=ORIENTED_EDGE('',*,*,#17101,.F.);
#22393=ORIENTED_EDGE('',*,*,#17102,.T.);
#22394=ORIENTED_EDGE('',*,*,#17103,.F.);
#22395=ORIENTED_EDGE('',*,*,#17102,.F.);
#22396=ORIENTED_EDGE('',*,*,#17104,.F.);
#22397=ORIENTED_EDGE('',*,*,#17094,.T.);
#22398=ORIENTED_EDGE('',*,*,#17105,.F.);
#22399=ORIENTED_EDGE('',*,*,#17106,.F.);
#22400=ORIENTED_EDGE('',*,*,#17107,.F.);
#22401=ORIENTED_EDGE('',*,*,#17108,.T.);
#22402=ORIENTED_EDGE('',*,*,#17109,.F.);
#22403=ORIENTED_EDGE('',*,*,#17108,.F.);
#22404=ORIENTED_EDGE('',*,*,#17110,.F.);
#22405=ORIENTED_EDGE('',*,*,#17111,.T.);
#22406=ORIENTED_EDGE('',*,*,#17112,.F.);
#22407=ORIENTED_EDGE('',*,*,#17111,.F.);
#22408=ORIENTED_EDGE('',*,*,#17113,.F.);
#22409=ORIENTED_EDGE('',*,*,#17114,.T.);
#22410=ORIENTED_EDGE('',*,*,#17115,.F.);
#22411=ORIENTED_EDGE('',*,*,#17114,.F.);
#22412=ORIENTED_EDGE('',*,*,#17116,.F.);
#22413=ORIENTED_EDGE('',*,*,#17106,.T.);
#22414=ORIENTED_EDGE('',*,*,#17116,.T.);
#22415=ORIENTED_EDGE('',*,*,#17113,.T.);
#22416=ORIENTED_EDGE('',*,*,#17110,.T.);
#22417=ORIENTED_EDGE('',*,*,#17107,.T.);
#22418=ORIENTED_EDGE('',*,*,#17101,.T.);
#22419=ORIENTED_EDGE('',*,*,#17098,.T.);
#22420=ORIENTED_EDGE('',*,*,#17095,.T.);
#22421=ORIENTED_EDGE('',*,*,#17104,.T.);
#22422=ORIENTED_EDGE('',*,*,#17117,.T.);
#22423=ORIENTED_EDGE('',*,*,#17118,.F.);
#22424=ORIENTED_EDGE('',*,*,#17119,.T.);
#22425=ORIENTED_EDGE('',*,*,#17120,.T.);
#22426=ORIENTED_EDGE('',*,*,#17121,.T.);
#22427=ORIENTED_EDGE('',*,*,#17122,.F.);
#22428=ORIENTED_EDGE('',*,*,#17123,.T.);
#22429=ORIENTED_EDGE('',*,*,#17118,.T.);
#22430=ORIENTED_EDGE('',*,*,#17124,.T.);
#22431=ORIENTED_EDGE('',*,*,#17125,.F.);
#22432=ORIENTED_EDGE('',*,*,#17126,.T.);
#22433=ORIENTED_EDGE('',*,*,#17122,.T.);
#22434=ORIENTED_EDGE('',*,*,#17127,.T.);
#22435=ORIENTED_EDGE('',*,*,#17120,.F.);
#22436=ORIENTED_EDGE('',*,*,#17128,.T.);
#22437=ORIENTED_EDGE('',*,*,#17125,.T.);
#22438=ORIENTED_EDGE('',*,*,#17117,.F.);
#22439=ORIENTED_EDGE('',*,*,#17127,.F.);
#22440=ORIENTED_EDGE('',*,*,#17124,.F.);
#22441=ORIENTED_EDGE('',*,*,#17121,.F.);
#22442=ORIENTED_EDGE('',*,*,#17105,.T.);
#22443=ORIENTED_EDGE('',*,*,#17109,.T.);
#22444=ORIENTED_EDGE('',*,*,#17112,.T.);
#22445=ORIENTED_EDGE('',*,*,#17115,.T.);
#22446=ORIENTED_EDGE('',*,*,#17128,.F.);
#22447=ORIENTED_EDGE('',*,*,#17119,.F.);
#22448=ORIENTED_EDGE('',*,*,#17123,.F.);
#22449=ORIENTED_EDGE('',*,*,#17126,.F.);
#22450=ORIENTED_EDGE('',*,*,#17100,.T.);
#22451=ORIENTED_EDGE('',*,*,#17103,.T.);
#22452=ORIENTED_EDGE('',*,*,#17093,.T.);
#22453=ORIENTED_EDGE('',*,*,#17097,.T.);
#22454=ORIENTED_EDGE('',*,*,#17129,.F.);
#22455=ORIENTED_EDGE('',*,*,#17130,.T.);
#22456=ORIENTED_EDGE('',*,*,#17131,.F.);
#22457=ORIENTED_EDGE('',*,*,#17130,.F.);
#22458=ORIENTED_EDGE('',*,*,#17132,.F.);
#22459=ORIENTED_EDGE('',*,*,#17133,.T.);
#22460=ORIENTED_EDGE('',*,*,#17134,.F.);
#22461=ORIENTED_EDGE('',*,*,#17133,.F.);
#22462=ORIENTED_EDGE('',*,*,#17135,.F.);
#22463=ORIENTED_EDGE('',*,*,#17136,.T.);
#22464=ORIENTED_EDGE('',*,*,#17137,.F.);
#22465=ORIENTED_EDGE('',*,*,#17136,.F.);
#22466=ORIENTED_EDGE('',*,*,#17138,.F.);
#22467=ORIENTED_EDGE('',*,*,#17139,.T.);
#22468=ORIENTED_EDGE('',*,*,#17140,.F.);
#22469=ORIENTED_EDGE('',*,*,#17139,.F.);
#22470=ORIENTED_EDGE('',*,*,#17141,.F.);
#22471=ORIENTED_EDGE('',*,*,#17142,.T.);
#22472=ORIENTED_EDGE('',*,*,#17143,.F.);
#22473=ORIENTED_EDGE('',*,*,#17142,.F.);
#22474=ORIENTED_EDGE('',*,*,#17144,.F.);
#22475=ORIENTED_EDGE('',*,*,#17145,.T.);
#22476=ORIENTED_EDGE('',*,*,#17146,.F.);
#22477=ORIENTED_EDGE('',*,*,#17145,.F.);
#22478=ORIENTED_EDGE('',*,*,#17147,.T.);
#22479=ORIENTED_EDGE('',*,*,#17148,.T.);
#22480=ORIENTED_EDGE('',*,*,#17149,.T.);
#22481=ORIENTED_EDGE('',*,*,#17150,.T.);
#22482=ORIENTED_EDGE('',*,*,#17131,.T.);
#22483=ORIENTED_EDGE('',*,*,#17134,.T.);
#22484=ORIENTED_EDGE('',*,*,#17137,.T.);
#22485=ORIENTED_EDGE('',*,*,#17140,.T.);
#22486=ORIENTED_EDGE('',*,*,#17143,.T.);
#22487=ORIENTED_EDGE('',*,*,#17146,.T.);
#22488=ORIENTED_EDGE('',*,*,#17151,.F.);
#22489=ORIENTED_EDGE('',*,*,#17152,.F.);
#22490=ORIENTED_EDGE('',*,*,#17153,.F.);
#22491=ORIENTED_EDGE('',*,*,#17154,.F.);
#22492=ORIENTED_EDGE('',*,*,#17155,.T.);
#22493=ORIENTED_EDGE('',*,*,#17156,.T.);
#22494=ORIENTED_EDGE('',*,*,#17150,.F.);
#22495=ORIENTED_EDGE('',*,*,#17157,.F.);
#22496=ORIENTED_EDGE('',*,*,#17158,.T.);
#22497=ORIENTED_EDGE('',*,*,#17157,.T.);
#22498=ORIENTED_EDGE('',*,*,#17149,.F.);
#22499=ORIENTED_EDGE('',*,*,#17159,.F.);
#22500=ORIENTED_EDGE('',*,*,#17160,.T.);
#22501=ORIENTED_EDGE('',*,*,#17159,.T.);
#22502=ORIENTED_EDGE('',*,*,#17148,.F.);
#22503=ORIENTED_EDGE('',*,*,#17161,.F.);
#22504=ORIENTED_EDGE('',*,*,#17162,.T.);
#22505=ORIENTED_EDGE('',*,*,#17161,.T.);
#22506=ORIENTED_EDGE('',*,*,#17147,.F.);
#22507=ORIENTED_EDGE('',*,*,#17156,.F.);
#22508=ORIENTED_EDGE('',*,*,#17154,.T.);
#22509=ORIENTED_EDGE('',*,*,#17163,.T.);
#22510=ORIENTED_EDGE('',*,*,#17164,.T.);
#22511=ORIENTED_EDGE('',*,*,#17165,.F.);
#22512=ORIENTED_EDGE('',*,*,#17153,.T.);
#22513=ORIENTED_EDGE('',*,*,#17166,.F.);
#22514=ORIENTED_EDGE('',*,*,#17167,.F.);
#22515=ORIENTED_EDGE('',*,*,#17168,.F.);
#22516=ORIENTED_EDGE('',*,*,#17169,.F.);
#22517=ORIENTED_EDGE('',*,*,#17163,.F.);
#22518=ORIENTED_EDGE('',*,*,#17170,.F.);
#22519=ORIENTED_EDGE('',*,*,#17171,.F.);
#22520=ORIENTED_EDGE('',*,*,#17172,.F.);
#22521=ORIENTED_EDGE('',*,*,#17173,.T.);
#22522=ORIENTED_EDGE('',*,*,#17170,.T.);
#22523=ORIENTED_EDGE('',*,*,#17174,.F.);
#22524=ORIENTED_EDGE('',*,*,#17175,.T.);
#22525=ORIENTED_EDGE('',*,*,#17176,.T.);
#22526=ORIENTED_EDGE('',*,*,#17177,.T.);
#22527=ORIENTED_EDGE('',*,*,#17178,.F.);
#22528=ORIENTED_EDGE('',*,*,#17179,.F.);
#22529=ORIENTED_EDGE('',*,*,#17180,.F.);
#22530=ORIENTED_EDGE('',*,*,#17181,.T.);
#22531=ORIENTED_EDGE('',*,*,#17175,.F.);
#22532=ORIENTED_EDGE('',*,*,#17182,.F.);
#22533=ORIENTED_EDGE('',*,*,#17183,.T.);
#22534=ORIENTED_EDGE('',*,*,#17184,.T.);
#22535=ORIENTED_EDGE('',*,*,#17183,.F.);
#22536=ORIENTED_EDGE('',*,*,#17185,.F.);
#22537=ORIENTED_EDGE('',*,*,#17186,.F.);
#22538=ORIENTED_EDGE('',*,*,#17187,.T.);
#22539=ORIENTED_EDGE('',*,*,#17188,.F.);
#22540=ORIENTED_EDGE('',*,*,#17189,.F.);
#22541=ORIENTED_EDGE('',*,*,#17178,.T.);
#22542=ORIENTED_EDGE('',*,*,#17179,.T.);
#22543=ORIENTED_EDGE('',*,*,#17189,.T.);
#22544=ORIENTED_EDGE('',*,*,#17190,.F.);
#22545=ORIENTED_EDGE('',*,*,#17185,.T.);
#22546=ORIENTED_EDGE('',*,*,#17182,.T.);
#22547=ORIENTED_EDGE('',*,*,#17174,.T.);
#22548=ORIENTED_EDGE('',*,*,#17173,.F.);
#22549=ORIENTED_EDGE('',*,*,#17191,.F.);
#22550=ORIENTED_EDGE('',*,*,#17176,.F.);
#22551=ORIENTED_EDGE('',*,*,#17181,.F.);
#22552=ORIENTED_EDGE('',*,*,#17184,.F.);
#22553=ORIENTED_EDGE('',*,*,#17192,.F.);
#22554=ORIENTED_EDGE('',*,*,#17187,.F.);
#22555=ORIENTED_EDGE('',*,*,#17177,.F.);
#22556=ORIENTED_EDGE('',*,*,#17193,.F.);
#22557=ORIENTED_EDGE('',*,*,#17171,.T.);
#22558=ORIENTED_EDGE('',*,*,#17162,.F.);
#22559=ORIENTED_EDGE('',*,*,#17155,.F.);
#22560=ORIENTED_EDGE('',*,*,#17158,.F.);
#22561=ORIENTED_EDGE('',*,*,#17160,.F.);
#22562=ORIENTED_EDGE('',*,*,#17129,.T.);
#22563=ORIENTED_EDGE('',*,*,#17132,.T.);
#22564=ORIENTED_EDGE('',*,*,#17135,.T.);
#22565=ORIENTED_EDGE('',*,*,#17138,.T.);
#22566=ORIENTED_EDGE('',*,*,#17141,.T.);
#22567=ORIENTED_EDGE('',*,*,#17144,.T.);
#22568=ORIENTED_EDGE('',*,*,#17180,.T.);
#22569=ORIENTED_EDGE('',*,*,#17191,.T.);
#22570=ORIENTED_EDGE('',*,*,#17172,.T.);
#22571=ORIENTED_EDGE('',*,*,#17193,.T.);
#22572=ORIENTED_EDGE('',*,*,#17152,.T.);
#22573=ORIENTED_EDGE('',*,*,#17194,.F.);
#22574=ORIENTED_EDGE('',*,*,#17195,.F.);
#22575=ORIENTED_EDGE('',*,*,#17166,.T.);
#22576=ORIENTED_EDGE('',*,*,#17196,.F.);
#22577=ORIENTED_EDGE('',*,*,#17197,.F.);
#22578=ORIENTED_EDGE('',*,*,#17167,.T.);
#22579=ORIENTED_EDGE('',*,*,#17195,.T.);
#22580=ORIENTED_EDGE('',*,*,#17198,.F.);
#22581=ORIENTED_EDGE('',*,*,#17199,.F.);
#22582=ORIENTED_EDGE('',*,*,#17168,.T.);
#22583=ORIENTED_EDGE('',*,*,#17197,.T.);
#22584=ORIENTED_EDGE('',*,*,#17188,.T.);
#22585=ORIENTED_EDGE('',*,*,#17192,.T.);
#22586=ORIENTED_EDGE('',*,*,#17186,.T.);
#22587=ORIENTED_EDGE('',*,*,#17190,.T.);
#22588=ORIENTED_EDGE('',*,*,#17200,.F.);
#22589=ORIENTED_EDGE('',*,*,#17164,.F.);
#22590=ORIENTED_EDGE('',*,*,#17169,.T.);
#22591=ORIENTED_EDGE('',*,*,#17199,.T.);
#22592=ORIENTED_EDGE('',*,*,#17151,.T.);
#22593=ORIENTED_EDGE('',*,*,#17165,.T.);
#22594=ORIENTED_EDGE('',*,*,#17200,.T.);
#22595=ORIENTED_EDGE('',*,*,#17198,.T.);
#22596=ORIENTED_EDGE('',*,*,#17196,.T.);
#22597=ORIENTED_EDGE('',*,*,#17194,.T.);
#22598=ORIENTED_EDGE('',*,*,#17201,.T.);
#22599=ORIENTED_EDGE('',*,*,#17202,.T.);
#22600=ORIENTED_EDGE('',*,*,#17203,.F.);
#22601=ORIENTED_EDGE('',*,*,#17204,.F.);
#22602=ORIENTED_EDGE('',*,*,#17202,.F.);
#22603=ORIENTED_EDGE('',*,*,#17205,.T.);
#22604=ORIENTED_EDGE('',*,*,#17206,.T.);
#22605=ORIENTED_EDGE('',*,*,#17207,.T.);
#22606=ORIENTED_EDGE('',*,*,#17208,.T.);
#22607=ORIENTED_EDGE('',*,*,#17209,.T.);
#22608=ORIENTED_EDGE('',*,*,#17210,.T.);
#22609=ORIENTED_EDGE('',*,*,#17211,.T.);
#22610=ORIENTED_EDGE('',*,*,#17212,.T.);
#22611=ORIENTED_EDGE('',*,*,#17213,.T.);
#22612=ORIENTED_EDGE('',*,*,#17214,.T.);
#22613=ORIENTED_EDGE('',*,*,#17215,.T.);
#22614=ORIENTED_EDGE('',*,*,#17216,.T.);
#22615=ORIENTED_EDGE('',*,*,#17207,.F.);
#22616=ORIENTED_EDGE('',*,*,#17217,.F.);
#22617=ORIENTED_EDGE('',*,*,#17218,.F.);
#22618=ORIENTED_EDGE('',*,*,#17219,.T.);
#22619=ORIENTED_EDGE('',*,*,#17208,.F.);
#22620=ORIENTED_EDGE('',*,*,#17219,.F.);
#22621=ORIENTED_EDGE('',*,*,#17220,.F.);
#22622=ORIENTED_EDGE('',*,*,#17221,.T.);
#22623=ORIENTED_EDGE('',*,*,#17209,.F.);
#22624=ORIENTED_EDGE('',*,*,#17221,.F.);
#22625=ORIENTED_EDGE('',*,*,#17222,.F.);
#22626=ORIENTED_EDGE('',*,*,#17223,.T.);
#22627=ORIENTED_EDGE('',*,*,#17224,.T.);
#22628=ORIENTED_EDGE('',*,*,#17225,.T.);
#22629=ORIENTED_EDGE('',*,*,#17203,.T.);
#22630=ORIENTED_EDGE('',*,*,#17204,.T.);
#22631=ORIENTED_EDGE('',*,*,#17226,.T.);
#22632=ORIENTED_EDGE('',*,*,#17227,.T.);
#22633=ORIENTED_EDGE('',*,*,#17224,.F.);
#22634=ORIENTED_EDGE('',*,*,#17228,.T.);
#22635=ORIENTED_EDGE('',*,*,#17226,.F.);
#22636=ORIENTED_EDGE('',*,*,#17229,.F.);
#22637=ORIENTED_EDGE('',*,*,#17230,.T.);
#22638=ORIENTED_EDGE('',*,*,#17231,.T.);
#22639=ORIENTED_EDGE('',*,*,#17232,.T.);
#22640=ORIENTED_EDGE('',*,*,#17233,.F.);
#22641=ORIENTED_EDGE('',*,*,#17234,.T.);
#22642=ORIENTED_EDGE('',*,*,#17235,.T.);
#22643=ORIENTED_EDGE('',*,*,#17236,.T.);
#22644=ORIENTED_EDGE('',*,*,#17237,.T.);
#22645=ORIENTED_EDGE('',*,*,#17238,.F.);
#22646=ORIENTED_EDGE('',*,*,#17239,.F.);
#22647=ORIENTED_EDGE('',*,*,#17240,.F.);
#22648=ORIENTED_EDGE('',*,*,#17241,.F.);
#22649=ORIENTED_EDGE('',*,*,#17228,.F.);
#22650=ORIENTED_EDGE('',*,*,#17225,.F.);
#22651=ORIENTED_EDGE('',*,*,#17227,.F.);
#22652=ORIENTED_EDGE('',*,*,#17242,.T.);
#22653=ORIENTED_EDGE('',*,*,#17233,.T.);
#22654=ORIENTED_EDGE('',*,*,#17243,.F.);
#22655=ORIENTED_EDGE('',*,*,#17244,.F.);
#22656=ORIENTED_EDGE('',*,*,#17245,.T.);
#22657=ORIENTED_EDGE('',*,*,#17246,.F.);
#22658=ORIENTED_EDGE('',*,*,#17247,.F.);
#22659=ORIENTED_EDGE('',*,*,#17248,.T.);
#22660=ORIENTED_EDGE('',*,*,#17249,.T.);
#22661=ORIENTED_EDGE('',*,*,#17250,.F.);
#22662=ORIENTED_EDGE('',*,*,#17251,.T.);
#22663=ORIENTED_EDGE('',*,*,#17252,.F.);
#22664=ORIENTED_EDGE('',*,*,#17251,.F.);
#22665=ORIENTED_EDGE('',*,*,#17253,.F.);
#22666=ORIENTED_EDGE('',*,*,#17254,.T.);
#22667=ORIENTED_EDGE('',*,*,#17255,.F.);
#22668=ORIENTED_EDGE('',*,*,#17256,.T.);
#22669=ORIENTED_EDGE('',*,*,#17231,.F.);
#22670=ORIENTED_EDGE('',*,*,#17257,.F.);
#22671=ORIENTED_EDGE('',*,*,#17258,.F.);
#22672=ORIENTED_EDGE('',*,*,#17259,.T.);
#22673=ORIENTED_EDGE('',*,*,#17260,.T.);
#22674=ORIENTED_EDGE('',*,*,#17261,.T.);
#22675=ORIENTED_EDGE('',*,*,#17262,.F.);
#22676=ORIENTED_EDGE('',*,*,#17261,.F.);
#22677=ORIENTED_EDGE('',*,*,#17263,.T.);
#22678=ORIENTED_EDGE('',*,*,#17264,.T.);
#22679=ORIENTED_EDGE('',*,*,#17252,.T.);
#22680=ORIENTED_EDGE('',*,*,#17255,.T.);
#22681=ORIENTED_EDGE('',*,*,#17265,.T.);
#22682=ORIENTED_EDGE('',*,*,#17245,.F.);
#22683=ORIENTED_EDGE('',*,*,#17266,.T.);
#22684=ORIENTED_EDGE('',*,*,#17267,.T.);
#22685=ORIENTED_EDGE('',*,*,#17268,.T.);
#22686=ORIENTED_EDGE('',*,*,#17269,.F.);
#22687=ORIENTED_EDGE('',*,*,#17270,.T.);
#22688=ORIENTED_EDGE('',*,*,#17271,.F.);
#22689=ORIENTED_EDGE('',*,*,#17263,.F.);
#22690=ORIENTED_EDGE('',*,*,#17260,.F.);
#22691=ORIENTED_EDGE('',*,*,#17272,.F.);
#22692=ORIENTED_EDGE('',*,*,#17273,.F.);
#22693=ORIENTED_EDGE('',*,*,#17274,.F.);
#22694=ORIENTED_EDGE('',*,*,#17259,.F.);
#22695=ORIENTED_EDGE('',*,*,#17271,.T.);
#22696=ORIENTED_EDGE('',*,*,#17262,.T.);
#22697=ORIENTED_EDGE('',*,*,#17275,.T.);
#22698=ORIENTED_EDGE('',*,*,#17276,.T.);
#22699=ORIENTED_EDGE('',*,*,#17277,.T.);
#22700=ORIENTED_EDGE('',*,*,#17278,.T.);
#22701=ORIENTED_EDGE('',*,*,#17279,.T.);
#22702=ORIENTED_EDGE('',*,*,#17280,.T.);
#22703=ORIENTED_EDGE('',*,*,#17281,.T.);
#22704=ORIENTED_EDGE('',*,*,#17282,.T.);
#22705=ORIENTED_EDGE('',*,*,#17283,.T.);
#22706=ORIENTED_EDGE('',*,*,#17284,.T.);
#22707=ORIENTED_EDGE('',*,*,#17285,.T.);
#22708=ORIENTED_EDGE('',*,*,#17286,.T.);
#22709=ORIENTED_EDGE('',*,*,#17287,.F.);
#22710=ORIENTED_EDGE('',*,*,#17288,.F.);
#22711=ORIENTED_EDGE('',*,*,#17289,.F.);
#22712=ORIENTED_EDGE('',*,*,#17290,.T.);
#22713=ORIENTED_EDGE('',*,*,#17291,.F.);
#22714=ORIENTED_EDGE('',*,*,#17292,.F.);
#22715=ORIENTED_EDGE('',*,*,#17293,.F.);
#22716=ORIENTED_EDGE('',*,*,#17288,.T.);
#22717=ORIENTED_EDGE('',*,*,#17294,.T.);
#22718=ORIENTED_EDGE('',*,*,#17240,.T.);
#22719=ORIENTED_EDGE('',*,*,#17295,.T.);
#22720=ORIENTED_EDGE('',*,*,#17296,.T.);
#22721=ORIENTED_EDGE('',*,*,#17241,.T.);
#22722=ORIENTED_EDGE('',*,*,#17294,.F.);
#22723=ORIENTED_EDGE('',*,*,#17239,.T.);
#22724=ORIENTED_EDGE('',*,*,#17296,.F.);
#22725=ORIENTED_EDGE('',*,*,#17297,.T.);
#22726=ORIENTED_EDGE('',*,*,#17274,.T.);
#22727=ORIENTED_EDGE('',*,*,#17298,.T.);
#22728=ORIENTED_EDGE('',*,*,#17299,.F.);
#22729=ORIENTED_EDGE('',*,*,#17298,.F.);
#22730=ORIENTED_EDGE('',*,*,#17273,.T.);
#22731=ORIENTED_EDGE('',*,*,#17300,.F.);
#22732=ORIENTED_EDGE('',*,*,#17301,.F.);
#22733=ORIENTED_EDGE('',*,*,#17302,.F.);
#22734=ORIENTED_EDGE('',*,*,#17303,.T.);
#22735=ORIENTED_EDGE('',*,*,#17304,.F.);
#22736=ORIENTED_EDGE('',*,*,#17305,.F.);
#22737=ORIENTED_EDGE('',*,*,#17306,.F.);
#22738=ORIENTED_EDGE('',*,*,#17301,.T.);
#22739=ORIENTED_EDGE('',*,*,#17307,.F.);
#22740=ORIENTED_EDGE('',*,*,#17308,.F.);
#22741=ORIENTED_EDGE('',*,*,#17309,.F.);
#22742=ORIENTED_EDGE('',*,*,#17305,.T.);
#22743=ORIENTED_EDGE('',*,*,#17310,.F.);
#22744=ORIENTED_EDGE('',*,*,#17311,.F.);
#22745=ORIENTED_EDGE('',*,*,#17312,.F.);
#22746=ORIENTED_EDGE('',*,*,#17308,.T.);
#22747=ORIENTED_EDGE('',*,*,#17313,.F.);
#22748=ORIENTED_EDGE('',*,*,#17314,.F.);
#22749=ORIENTED_EDGE('',*,*,#17315,.F.);
#22750=ORIENTED_EDGE('',*,*,#17311,.T.);
#22751=ORIENTED_EDGE('',*,*,#17316,.F.);
#22752=ORIENTED_EDGE('',*,*,#17317,.F.);
#22753=ORIENTED_EDGE('',*,*,#17318,.F.);
#22754=ORIENTED_EDGE('',*,*,#17314,.T.);
#22755=ORIENTED_EDGE('',*,*,#17319,.F.);
#22756=ORIENTED_EDGE('',*,*,#17320,.F.);
#22757=ORIENTED_EDGE('',*,*,#17321,.F.);
#22758=ORIENTED_EDGE('',*,*,#17317,.T.);
#22759=ORIENTED_EDGE('',*,*,#17322,.F.);
#22760=ORIENTED_EDGE('',*,*,#17323,.F.);
#22761=ORIENTED_EDGE('',*,*,#17324,.F.);
#22762=ORIENTED_EDGE('',*,*,#17320,.T.);
#22763=ORIENTED_EDGE('',*,*,#17325,.F.);
#22764=ORIENTED_EDGE('',*,*,#17326,.F.);
#22765=ORIENTED_EDGE('',*,*,#17327,.F.);
#22766=ORIENTED_EDGE('',*,*,#17323,.T.);
#22767=ORIENTED_EDGE('',*,*,#17328,.F.);
#22768=ORIENTED_EDGE('',*,*,#17329,.F.);
#22769=ORIENTED_EDGE('',*,*,#17330,.F.);
#22770=ORIENTED_EDGE('',*,*,#17326,.T.);
#22771=ORIENTED_EDGE('',*,*,#17331,.F.);
#22772=ORIENTED_EDGE('',*,*,#17332,.F.);
#22773=ORIENTED_EDGE('',*,*,#17333,.F.);
#22774=ORIENTED_EDGE('',*,*,#17329,.T.);
#22775=ORIENTED_EDGE('',*,*,#17334,.F.);
#22776=ORIENTED_EDGE('',*,*,#17303,.F.);
#22777=ORIENTED_EDGE('',*,*,#17335,.F.);
#22778=ORIENTED_EDGE('',*,*,#17332,.T.);
#22779=ORIENTED_EDGE('',*,*,#17302,.T.);
#22780=ORIENTED_EDGE('',*,*,#17306,.T.);
#22781=ORIENTED_EDGE('',*,*,#17309,.T.);
#22782=ORIENTED_EDGE('',*,*,#17312,.T.);
#22783=ORIENTED_EDGE('',*,*,#17315,.T.);
#22784=ORIENTED_EDGE('',*,*,#17318,.T.);
#22785=ORIENTED_EDGE('',*,*,#17321,.T.);
#22786=ORIENTED_EDGE('',*,*,#17324,.T.);
#22787=ORIENTED_EDGE('',*,*,#17327,.T.);
#22788=ORIENTED_EDGE('',*,*,#17330,.T.);
#22789=ORIENTED_EDGE('',*,*,#17333,.T.);
#22790=ORIENTED_EDGE('',*,*,#17335,.T.);
#22791=ORIENTED_EDGE('',*,*,#17299,.T.);
#22792=ORIENTED_EDGE('',*,*,#17322,.T.);
#22793=ORIENTED_EDGE('',*,*,#17319,.T.);
#22794=ORIENTED_EDGE('',*,*,#17316,.T.);
#22795=ORIENTED_EDGE('',*,*,#17313,.T.);
#22796=ORIENTED_EDGE('',*,*,#17310,.T.);
#22797=ORIENTED_EDGE('',*,*,#17307,.T.);
#22798=ORIENTED_EDGE('',*,*,#17304,.T.);
#22799=ORIENTED_EDGE('',*,*,#17300,.T.);
#22800=ORIENTED_EDGE('',*,*,#17334,.T.);
#22801=ORIENTED_EDGE('',*,*,#17331,.T.);
#22802=ORIENTED_EDGE('',*,*,#17328,.T.);
#22803=ORIENTED_EDGE('',*,*,#17325,.T.);
#22804=ORIENTED_EDGE('',*,*,#17297,.F.);
#22805=ORIENTED_EDGE('',*,*,#17272,.T.);
#22806=ORIENTED_EDGE('',*,*,#17336,.F.);
#22807=ORIENTED_EDGE('',*,*,#17257,.T.);
#22808=ORIENTED_EDGE('',*,*,#17230,.F.);
#22809=ORIENTED_EDGE('',*,*,#17337,.T.);
#22810=ORIENTED_EDGE('',*,*,#17338,.F.);
#22811=ORIENTED_EDGE('',*,*,#17339,.F.);
#22812=ORIENTED_EDGE('',*,*,#17340,.T.);
#22813=ORIENTED_EDGE('',*,*,#17341,.T.);
#22814=ORIENTED_EDGE('',*,*,#17342,.F.);
#22815=ORIENTED_EDGE('',*,*,#17341,.F.);
#22816=ORIENTED_EDGE('',*,*,#17343,.T.);
#22817=ORIENTED_EDGE('',*,*,#17344,.T.);
#22818=ORIENTED_EDGE('',*,*,#17345,.F.);
#22819=ORIENTED_EDGE('',*,*,#17344,.F.);
#22820=ORIENTED_EDGE('',*,*,#17346,.T.);
#22821=ORIENTED_EDGE('',*,*,#17347,.T.);
#22822=ORIENTED_EDGE('',*,*,#17348,.F.);
#22823=ORIENTED_EDGE('',*,*,#17347,.F.);
#22824=ORIENTED_EDGE('',*,*,#17349,.T.);
#22825=ORIENTED_EDGE('',*,*,#17350,.T.);
#22826=ORIENTED_EDGE('',*,*,#17351,.F.);
#22827=ORIENTED_EDGE('',*,*,#17350,.F.);
#22828=ORIENTED_EDGE('',*,*,#17352,.T.);
#22829=ORIENTED_EDGE('',*,*,#17353,.T.);
#22830=ORIENTED_EDGE('',*,*,#17354,.F.);
#22831=ORIENTED_EDGE('',*,*,#17353,.F.);
#22832=ORIENTED_EDGE('',*,*,#17355,.T.);
#22833=ORIENTED_EDGE('',*,*,#17356,.T.);
#22834=ORIENTED_EDGE('',*,*,#17357,.F.);
#22835=ORIENTED_EDGE('',*,*,#17356,.F.);
#22836=ORIENTED_EDGE('',*,*,#17358,.T.);
#22837=ORIENTED_EDGE('',*,*,#17359,.T.);
#22838=ORIENTED_EDGE('',*,*,#17360,.F.);
#22839=ORIENTED_EDGE('',*,*,#17359,.F.);
#22840=ORIENTED_EDGE('',*,*,#17361,.T.);
#22841=ORIENTED_EDGE('',*,*,#17339,.T.);
#22842=ORIENTED_EDGE('',*,*,#17338,.T.);
#22843=ORIENTED_EDGE('',*,*,#17342,.T.);
#22844=ORIENTED_EDGE('',*,*,#17345,.T.);
#22845=ORIENTED_EDGE('',*,*,#17348,.T.);
#22846=ORIENTED_EDGE('',*,*,#17351,.T.);
#22847=ORIENTED_EDGE('',*,*,#17354,.T.);
#22848=ORIENTED_EDGE('',*,*,#17357,.T.);
#22849=ORIENTED_EDGE('',*,*,#17360,.T.);
#22850=ORIENTED_EDGE('',*,*,#17362,.T.);
#22851=ORIENTED_EDGE('',*,*,#17363,.T.);
#22852=ORIENTED_EDGE('',*,*,#17364,.F.);
#22853=ORIENTED_EDGE('',*,*,#17365,.F.);
#22854=ORIENTED_EDGE('',*,*,#17340,.F.);
#22855=ORIENTED_EDGE('',*,*,#17361,.F.);
#22856=ORIENTED_EDGE('',*,*,#17358,.F.);
#22857=ORIENTED_EDGE('',*,*,#17355,.F.);
#22858=ORIENTED_EDGE('',*,*,#17352,.F.);
#22859=ORIENTED_EDGE('',*,*,#17349,.F.);
#22860=ORIENTED_EDGE('',*,*,#17346,.F.);
#22861=ORIENTED_EDGE('',*,*,#17343,.F.);
#22862=ORIENTED_EDGE('',*,*,#17366,.F.);
#22863=ORIENTED_EDGE('',*,*,#17367,.F.);
#22864=ORIENTED_EDGE('',*,*,#17368,.T.);
#22865=ORIENTED_EDGE('',*,*,#17369,.T.);
#22866=ORIENTED_EDGE('',*,*,#17370,.T.);
#22867=ORIENTED_EDGE('',*,*,#17371,.T.);
#22868=ORIENTED_EDGE('',*,*,#17372,.T.);
#22869=ORIENTED_EDGE('',*,*,#17373,.T.);
#22870=ORIENTED_EDGE('',*,*,#17374,.T.);
#22871=ORIENTED_EDGE('',*,*,#17375,.T.);
#22872=ORIENTED_EDGE('',*,*,#17369,.F.);
#22873=ORIENTED_EDGE('',*,*,#17376,.F.);
#22874=ORIENTED_EDGE('',*,*,#17377,.T.);
#22875=ORIENTED_EDGE('',*,*,#17378,.T.);
#22876=ORIENTED_EDGE('',*,*,#17370,.F.);
#22877=ORIENTED_EDGE('',*,*,#17378,.F.);
#22878=ORIENTED_EDGE('',*,*,#17379,.T.);
#22879=ORIENTED_EDGE('',*,*,#17380,.T.);
#22880=ORIENTED_EDGE('',*,*,#17371,.F.);
#22881=ORIENTED_EDGE('',*,*,#17380,.F.);
#22882=ORIENTED_EDGE('',*,*,#17381,.T.);
#22883=ORIENTED_EDGE('',*,*,#17382,.T.);
#22884=ORIENTED_EDGE('',*,*,#17372,.F.);
#22885=ORIENTED_EDGE('',*,*,#17382,.F.);
#22886=ORIENTED_EDGE('',*,*,#17383,.T.);
#22887=ORIENTED_EDGE('',*,*,#17384,.T.);
#22888=ORIENTED_EDGE('',*,*,#17373,.F.);
#22889=ORIENTED_EDGE('',*,*,#17384,.F.);
#22890=ORIENTED_EDGE('',*,*,#17385,.T.);
#22891=ORIENTED_EDGE('',*,*,#17386,.T.);
#22892=ORIENTED_EDGE('',*,*,#17374,.F.);
#22893=ORIENTED_EDGE('',*,*,#17386,.F.);
#22894=ORIENTED_EDGE('',*,*,#17387,.T.);
#22895=ORIENTED_EDGE('',*,*,#17388,.T.);
#22896=ORIENTED_EDGE('',*,*,#17375,.F.);
#22897=ORIENTED_EDGE('',*,*,#17388,.F.);
#22898=ORIENTED_EDGE('',*,*,#17389,.T.);
#22899=ORIENTED_EDGE('',*,*,#17390,.T.);
#22900=ORIENTED_EDGE('',*,*,#17368,.F.);
#22901=ORIENTED_EDGE('',*,*,#17390,.F.);
#22902=ORIENTED_EDGE('',*,*,#17391,.T.);
#22903=ORIENTED_EDGE('',*,*,#17376,.T.);
#22904=ORIENTED_EDGE('',*,*,#17377,.F.);
#22905=ORIENTED_EDGE('',*,*,#17391,.F.);
#22906=ORIENTED_EDGE('',*,*,#17389,.F.);
#22907=ORIENTED_EDGE('',*,*,#17387,.F.);
#22908=ORIENTED_EDGE('',*,*,#17385,.F.);
#22909=ORIENTED_EDGE('',*,*,#17383,.F.);
#22910=ORIENTED_EDGE('',*,*,#17381,.F.);
#22911=ORIENTED_EDGE('',*,*,#17379,.F.);
#22912=ORIENTED_EDGE('',*,*,#17392,.F.);
#22913=ORIENTED_EDGE('',*,*,#17393,.T.);
#22914=ORIENTED_EDGE('',*,*,#17394,.T.);
#22915=ORIENTED_EDGE('',*,*,#17395,.T.);
#22916=ORIENTED_EDGE('',*,*,#17396,.T.);
#22917=ORIENTED_EDGE('',*,*,#17397,.T.);
#22918=ORIENTED_EDGE('',*,*,#17398,.T.);
#22919=ORIENTED_EDGE('',*,*,#17399,.T.);
#22920=ORIENTED_EDGE('',*,*,#17400,.T.);
#22921=ORIENTED_EDGE('',*,*,#17401,.T.);
#22922=ORIENTED_EDGE('',*,*,#17402,.T.);
#22923=ORIENTED_EDGE('',*,*,#17403,.T.);
#22924=ORIENTED_EDGE('',*,*,#17404,.T.);
#22925=ORIENTED_EDGE('',*,*,#17392,.T.);
#22926=ORIENTED_EDGE('',*,*,#17405,.T.);
#22927=ORIENTED_EDGE('',*,*,#17367,.T.);
#22928=ORIENTED_EDGE('',*,*,#17405,.F.);
#22929=ORIENTED_EDGE('',*,*,#17406,.F.);
#22930=ORIENTED_EDGE('',*,*,#17407,.T.);
#22931=ORIENTED_EDGE('',*,*,#17408,.T.);
#22932=ORIENTED_EDGE('',*,*,#17409,.T.);
#22933=ORIENTED_EDGE('',*,*,#17410,.T.);
#22934=ORIENTED_EDGE('',*,*,#17411,.T.);
#22935=ORIENTED_EDGE('',*,*,#17412,.T.);
#22936=ORIENTED_EDGE('',*,*,#17413,.T.);
#22937=ORIENTED_EDGE('',*,*,#17414,.T.);
#22938=ORIENTED_EDGE('',*,*,#17415,.T.);
#22939=ORIENTED_EDGE('',*,*,#17416,.T.);
#22940=ORIENTED_EDGE('',*,*,#17417,.T.);
#22941=ORIENTED_EDGE('',*,*,#17418,.T.);
#22942=ORIENTED_EDGE('',*,*,#17406,.T.);
#22943=ORIENTED_EDGE('',*,*,#17419,.T.);
#22944=ORIENTED_EDGE('',*,*,#17366,.T.);
#22945=ORIENTED_EDGE('',*,*,#17419,.F.);
#22946=ORIENTED_EDGE('',*,*,#17420,.F.);
#22947=ORIENTED_EDGE('',*,*,#17421,.T.);
#22948=ORIENTED_EDGE('',*,*,#17422,.T.);
#22949=ORIENTED_EDGE('',*,*,#17417,.F.);
#22950=ORIENTED_EDGE('',*,*,#17422,.F.);
#22951=ORIENTED_EDGE('',*,*,#17423,.T.);
#22952=ORIENTED_EDGE('',*,*,#17424,.T.);
#22953=ORIENTED_EDGE('',*,*,#17418,.F.);
#22954=ORIENTED_EDGE('',*,*,#17424,.F.);
#22955=ORIENTED_EDGE('',*,*,#17425,.T.);
#22956=ORIENTED_EDGE('',*,*,#17426,.T.);
#22957=ORIENTED_EDGE('',*,*,#17407,.F.);
#22958=ORIENTED_EDGE('',*,*,#17426,.F.);
#22959=ORIENTED_EDGE('',*,*,#17427,.T.);
#22960=ORIENTED_EDGE('',*,*,#17428,.T.);
#22961=ORIENTED_EDGE('',*,*,#17408,.F.);
#22962=ORIENTED_EDGE('',*,*,#17428,.F.);
#22963=ORIENTED_EDGE('',*,*,#17429,.T.);
#22964=ORIENTED_EDGE('',*,*,#17430,.T.);
#22965=ORIENTED_EDGE('',*,*,#17409,.F.);
#22966=ORIENTED_EDGE('',*,*,#17430,.F.);
#22967=ORIENTED_EDGE('',*,*,#17431,.T.);
#22968=ORIENTED_EDGE('',*,*,#17432,.T.);
#22969=ORIENTED_EDGE('',*,*,#17410,.F.);
#22970=ORIENTED_EDGE('',*,*,#17432,.F.);
#22971=ORIENTED_EDGE('',*,*,#17433,.T.);
#22972=ORIENTED_EDGE('',*,*,#17434,.T.);
#22973=ORIENTED_EDGE('',*,*,#17411,.F.);
#22974=ORIENTED_EDGE('',*,*,#17434,.F.);
#22975=ORIENTED_EDGE('',*,*,#17435,.T.);
#22976=ORIENTED_EDGE('',*,*,#17436,.T.);
#22977=ORIENTED_EDGE('',*,*,#17412,.F.);
#22978=ORIENTED_EDGE('',*,*,#17436,.F.);
#22979=ORIENTED_EDGE('',*,*,#17437,.T.);
#22980=ORIENTED_EDGE('',*,*,#17438,.T.);
#22981=ORIENTED_EDGE('',*,*,#17413,.F.);
#22982=ORIENTED_EDGE('',*,*,#17438,.F.);
#22983=ORIENTED_EDGE('',*,*,#17439,.T.);
#22984=ORIENTED_EDGE('',*,*,#17440,.T.);
#22985=ORIENTED_EDGE('',*,*,#17414,.F.);
#22986=ORIENTED_EDGE('',*,*,#17440,.F.);
#22987=ORIENTED_EDGE('',*,*,#17441,.T.);
#22988=ORIENTED_EDGE('',*,*,#17442,.T.);
#22989=ORIENTED_EDGE('',*,*,#17415,.F.);
#22990=ORIENTED_EDGE('',*,*,#17442,.F.);
#22991=ORIENTED_EDGE('',*,*,#17443,.T.);
#22992=ORIENTED_EDGE('',*,*,#17420,.T.);
#22993=ORIENTED_EDGE('',*,*,#17416,.F.);
#22994=ORIENTED_EDGE('',*,*,#17421,.F.);
#22995=ORIENTED_EDGE('',*,*,#17443,.F.);
#22996=ORIENTED_EDGE('',*,*,#17441,.F.);
#22997=ORIENTED_EDGE('',*,*,#17439,.F.);
#22998=ORIENTED_EDGE('',*,*,#17437,.F.);
#22999=ORIENTED_EDGE('',*,*,#17435,.F.);
#23000=ORIENTED_EDGE('',*,*,#17433,.F.);
#23001=ORIENTED_EDGE('',*,*,#17431,.F.);
#23002=ORIENTED_EDGE('',*,*,#17429,.F.);
#23003=ORIENTED_EDGE('',*,*,#17427,.F.);
#23004=ORIENTED_EDGE('',*,*,#17425,.F.);
#23005=ORIENTED_EDGE('',*,*,#17423,.F.);
#23006=ORIENTED_EDGE('',*,*,#17444,.F.);
#23007=ORIENTED_EDGE('',*,*,#17445,.T.);
#23008=ORIENTED_EDGE('',*,*,#17446,.T.);
#23009=ORIENTED_EDGE('',*,*,#17403,.F.);
#23010=ORIENTED_EDGE('',*,*,#17446,.F.);
#23011=ORIENTED_EDGE('',*,*,#17447,.T.);
#23012=ORIENTED_EDGE('',*,*,#17448,.T.);
#23013=ORIENTED_EDGE('',*,*,#17404,.F.);
#23014=ORIENTED_EDGE('',*,*,#17448,.F.);
#23015=ORIENTED_EDGE('',*,*,#17449,.T.);
#23016=ORIENTED_EDGE('',*,*,#17450,.T.);
#23017=ORIENTED_EDGE('',*,*,#17393,.F.);
#23018=ORIENTED_EDGE('',*,*,#17450,.F.);
#23019=ORIENTED_EDGE('',*,*,#17451,.T.);
#23020=ORIENTED_EDGE('',*,*,#17452,.T.);
#23021=ORIENTED_EDGE('',*,*,#17394,.F.);
#23022=ORIENTED_EDGE('',*,*,#17452,.F.);
#23023=ORIENTED_EDGE('',*,*,#17453,.T.);
#23024=ORIENTED_EDGE('',*,*,#17454,.T.);
#23025=ORIENTED_EDGE('',*,*,#17395,.F.);
#23026=ORIENTED_EDGE('',*,*,#17454,.F.);
#23027=ORIENTED_EDGE('',*,*,#17455,.T.);
#23028=ORIENTED_EDGE('',*,*,#17456,.T.);
#23029=ORIENTED_EDGE('',*,*,#17396,.F.);
#23030=ORIENTED_EDGE('',*,*,#17456,.F.);
#23031=ORIENTED_EDGE('',*,*,#17457,.T.);
#23032=ORIENTED_EDGE('',*,*,#17458,.T.);
#23033=ORIENTED_EDGE('',*,*,#17397,.F.);
#23034=ORIENTED_EDGE('',*,*,#17458,.F.);
#23035=ORIENTED_EDGE('',*,*,#17459,.T.);
#23036=ORIENTED_EDGE('',*,*,#17460,.T.);
#23037=ORIENTED_EDGE('',*,*,#17398,.F.);
#23038=ORIENTED_EDGE('',*,*,#17460,.F.);
#23039=ORIENTED_EDGE('',*,*,#17461,.T.);
#23040=ORIENTED_EDGE('',*,*,#17462,.T.);
#23041=ORIENTED_EDGE('',*,*,#17399,.F.);
#23042=ORIENTED_EDGE('',*,*,#17462,.F.);
#23043=ORIENTED_EDGE('',*,*,#17463,.T.);
#23044=ORIENTED_EDGE('',*,*,#17464,.T.);
#23045=ORIENTED_EDGE('',*,*,#17400,.F.);
#23046=ORIENTED_EDGE('',*,*,#17464,.F.);
#23047=ORIENTED_EDGE('',*,*,#17465,.T.);
#23048=ORIENTED_EDGE('',*,*,#17466,.T.);
#23049=ORIENTED_EDGE('',*,*,#17401,.F.);
#23050=ORIENTED_EDGE('',*,*,#17466,.F.);
#23051=ORIENTED_EDGE('',*,*,#17467,.T.);
#23052=ORIENTED_EDGE('',*,*,#17444,.T.);
#23053=ORIENTED_EDGE('',*,*,#17402,.F.);
#23054=ORIENTED_EDGE('',*,*,#17445,.F.);
#23055=ORIENTED_EDGE('',*,*,#17467,.F.);
#23056=ORIENTED_EDGE('',*,*,#17465,.F.);
#23057=ORIENTED_EDGE('',*,*,#17463,.F.);
#23058=ORIENTED_EDGE('',*,*,#17461,.F.);
#23059=ORIENTED_EDGE('',*,*,#17459,.F.);
#23060=ORIENTED_EDGE('',*,*,#17457,.F.);
#23061=ORIENTED_EDGE('',*,*,#17455,.F.);
#23062=ORIENTED_EDGE('',*,*,#17453,.F.);
#23063=ORIENTED_EDGE('',*,*,#17451,.F.);
#23064=ORIENTED_EDGE('',*,*,#17449,.F.);
#23065=ORIENTED_EDGE('',*,*,#17447,.F.);
#23066=ORIENTED_EDGE('',*,*,#17222,.T.);
#23067=ORIENTED_EDGE('',*,*,#17220,.T.);
#23068=ORIENTED_EDGE('',*,*,#17218,.T.);
#23069=ORIENTED_EDGE('',*,*,#17468,.T.);
#23070=ORIENTED_EDGE('',*,*,#17469,.T.);
#23071=ORIENTED_EDGE('',*,*,#17470,.T.);
#23072=ORIENTED_EDGE('',*,*,#17471,.T.);
#23073=ORIENTED_EDGE('',*,*,#17472,.T.);
#23074=ORIENTED_EDGE('',*,*,#17473,.T.);
#23075=ORIENTED_EDGE('',*,*,#17474,.T.);
#23076=ORIENTED_EDGE('',*,*,#17475,.T.);
#23077=ORIENTED_EDGE('',*,*,#17476,.T.);
#23078=ORIENTED_EDGE('',*,*,#17210,.F.);
#23079=ORIENTED_EDGE('',*,*,#17223,.F.);
#23080=ORIENTED_EDGE('',*,*,#17476,.F.);
#23081=ORIENTED_EDGE('',*,*,#17477,.T.);
#23082=ORIENTED_EDGE('',*,*,#17211,.F.);
#23083=ORIENTED_EDGE('',*,*,#17477,.F.);
#23084=ORIENTED_EDGE('',*,*,#17475,.F.);
#23085=ORIENTED_EDGE('',*,*,#17478,.T.);
#23086=ORIENTED_EDGE('',*,*,#17212,.F.);
#23087=ORIENTED_EDGE('',*,*,#17478,.F.);
#23088=ORIENTED_EDGE('',*,*,#17474,.F.);
#23089=ORIENTED_EDGE('',*,*,#17479,.T.);
#23090=ORIENTED_EDGE('',*,*,#17213,.F.);
#23091=ORIENTED_EDGE('',*,*,#17479,.F.);
#23092=ORIENTED_EDGE('',*,*,#17473,.F.);
#23093=ORIENTED_EDGE('',*,*,#17480,.T.);
#23094=ORIENTED_EDGE('',*,*,#17214,.F.);
#23095=ORIENTED_EDGE('',*,*,#17480,.F.);
#23096=ORIENTED_EDGE('',*,*,#17472,.F.);
#23097=ORIENTED_EDGE('',*,*,#17481,.T.);
#23098=ORIENTED_EDGE('',*,*,#17215,.F.);
#23099=ORIENTED_EDGE('',*,*,#17481,.F.);
#23100=ORIENTED_EDGE('',*,*,#17471,.F.);
#23101=ORIENTED_EDGE('',*,*,#17482,.T.);
#23102=ORIENTED_EDGE('',*,*,#17216,.F.);
#23103=ORIENTED_EDGE('',*,*,#17482,.F.);
#23104=ORIENTED_EDGE('',*,*,#17470,.F.);
#23105=ORIENTED_EDGE('',*,*,#17483,.T.);
#23106=ORIENTED_EDGE('',*,*,#17201,.F.);
#23107=ORIENTED_EDGE('',*,*,#17483,.F.);
#23108=ORIENTED_EDGE('',*,*,#17469,.F.);
#23109=ORIENTED_EDGE('',*,*,#17484,.T.);
#23110=ORIENTED_EDGE('',*,*,#17205,.F.);
#23111=ORIENTED_EDGE('',*,*,#17206,.F.);
#23112=ORIENTED_EDGE('',*,*,#17484,.F.);
#23113=ORIENTED_EDGE('',*,*,#17468,.F.);
#23114=ORIENTED_EDGE('',*,*,#17217,.T.);
#23115=ORIENTED_EDGE('',*,*,#17485,.F.);
#23116=ORIENTED_EDGE('',*,*,#17486,.F.);
#23117=ORIENTED_EDGE('',*,*,#17236,.F.);
#23118=ORIENTED_EDGE('',*,*,#17487,.F.);
#23119=ORIENTED_EDGE('',*,*,#17487,.T.);
#23120=ORIENTED_EDGE('',*,*,#17235,.F.);
#23121=ORIENTED_EDGE('',*,*,#17488,.F.);
#23122=ORIENTED_EDGE('',*,*,#17489,.F.);
#23123=ORIENTED_EDGE('',*,*,#17490,.F.);
#23124=ORIENTED_EDGE('',*,*,#17488,.T.);
#23125=ORIENTED_EDGE('',*,*,#17234,.F.);
#23126=ORIENTED_EDGE('',*,*,#17242,.F.);
#23127=ORIENTED_EDGE('',*,*,#17491,.F.);
#23128=ORIENTED_EDGE('',*,*,#17243,.T.);
#23129=ORIENTED_EDGE('',*,*,#17232,.F.);
#23130=ORIENTED_EDGE('',*,*,#17256,.F.);
#23131=ORIENTED_EDGE('',*,*,#17492,.F.);
#23132=ORIENTED_EDGE('',*,*,#17493,.F.);
#23133=ORIENTED_EDGE('',*,*,#17494,.F.);
#23134=ORIENTED_EDGE('',*,*,#17268,.F.);
#23135=ORIENTED_EDGE('',*,*,#17337,.F.);
#23136=ORIENTED_EDGE('',*,*,#17229,.T.);
#23137=ORIENTED_EDGE('',*,*,#17495,.T.);
#23138=ORIENTED_EDGE('',*,*,#17365,.T.);
#23139=ORIENTED_EDGE('',*,*,#17496,.T.);
#23140=ORIENTED_EDGE('',*,*,#17269,.T.);
#23141=ORIENTED_EDGE('',*,*,#17494,.T.);
#23142=ORIENTED_EDGE('',*,*,#17497,.F.);
#23143=ORIENTED_EDGE('',*,*,#17237,.F.);
#23144=ORIENTED_EDGE('',*,*,#17486,.T.);
#23145=ORIENTED_EDGE('',*,*,#17498,.F.);
#23146=ORIENTED_EDGE('',*,*,#17249,.F.);
#23147=ORIENTED_EDGE('',*,*,#17264,.F.);
#23148=ORIENTED_EDGE('',*,*,#17499,.F.);
#23149=ORIENTED_EDGE('',*,*,#17363,.F.);
#23150=ORIENTED_EDGE('',*,*,#17500,.F.);
#23151=ORIENTED_EDGE('',*,*,#17254,.F.);
#23152=ORIENTED_EDGE('',*,*,#17501,.F.);
#23153=ORIENTED_EDGE('',*,*,#17246,.T.);
#23154=ORIENTED_EDGE('',*,*,#17265,.F.);
#23155=ORIENTED_EDGE('',*,*,#17248,.F.);
#23156=ORIENTED_EDGE('',*,*,#17502,.F.);
#23157=ORIENTED_EDGE('',*,*,#17503,.T.);
#23158=ORIENTED_EDGE('',*,*,#17266,.F.);
#23159=ORIENTED_EDGE('',*,*,#17503,.F.);
#23160=ORIENTED_EDGE('',*,*,#17504,.F.);
#23161=ORIENTED_EDGE('',*,*,#17492,.T.);
#23162=ORIENTED_EDGE('',*,*,#17267,.F.);
#23163=ORIENTED_EDGE('',*,*,#17499,.T.);
#23164=ORIENTED_EDGE('',*,*,#17270,.F.);
#23165=ORIENTED_EDGE('',*,*,#17496,.F.);
#23166=ORIENTED_EDGE('',*,*,#17364,.T.);
#23167=ORIENTED_EDGE('',*,*,#17505,.T.);
#23168=ORIENTED_EDGE('',*,*,#17500,.T.);
#23169=ORIENTED_EDGE('',*,*,#17362,.F.);
#23170=ORIENTED_EDGE('',*,*,#17495,.F.);
#23171=ORIENTED_EDGE('',*,*,#17238,.T.);
#23172=ORIENTED_EDGE('',*,*,#17285,.F.);
#23173=ORIENTED_EDGE('',*,*,#17506,.F.);
#23174=ORIENTED_EDGE('',*,*,#17507,.F.);
#23175=ORIENTED_EDGE('',*,*,#17508,.T.);
#23176=ORIENTED_EDGE('',*,*,#17286,.F.);
#23177=ORIENTED_EDGE('',*,*,#17508,.F.);
#23178=ORIENTED_EDGE('',*,*,#17509,.F.);
#23179=ORIENTED_EDGE('',*,*,#17510,.T.);
#23180=ORIENTED_EDGE('',*,*,#17284,.F.);
#23181=ORIENTED_EDGE('',*,*,#17511,.F.);
#23182=ORIENTED_EDGE('',*,*,#17512,.F.);
#23183=ORIENTED_EDGE('',*,*,#17506,.T.);
#23184=ORIENTED_EDGE('',*,*,#17275,.F.);
#23185=ORIENTED_EDGE('',*,*,#17510,.F.);
#23186=ORIENTED_EDGE('',*,*,#17513,.F.);
#23187=ORIENTED_EDGE('',*,*,#17514,.T.);
#23188=ORIENTED_EDGE('',*,*,#17276,.F.);
#23189=ORIENTED_EDGE('',*,*,#17514,.F.);
#23190=ORIENTED_EDGE('',*,*,#17515,.F.);
#23191=ORIENTED_EDGE('',*,*,#17516,.T.);
#23192=ORIENTED_EDGE('',*,*,#17277,.F.);
#23193=ORIENTED_EDGE('',*,*,#17516,.F.);
#23194=ORIENTED_EDGE('',*,*,#17517,.F.);
#23195=ORIENTED_EDGE('',*,*,#17518,.T.);
#23196=ORIENTED_EDGE('',*,*,#17278,.F.);
#23197=ORIENTED_EDGE('',*,*,#17518,.F.);
#23198=ORIENTED_EDGE('',*,*,#17519,.F.);
#23199=ORIENTED_EDGE('',*,*,#17520,.T.);
#23200=ORIENTED_EDGE('',*,*,#17279,.F.);
#23201=ORIENTED_EDGE('',*,*,#17520,.F.);
#23202=ORIENTED_EDGE('',*,*,#17521,.F.);
#23203=ORIENTED_EDGE('',*,*,#17522,.T.);
#23204=ORIENTED_EDGE('',*,*,#17280,.F.);
#23205=ORIENTED_EDGE('',*,*,#17522,.F.);
#23206=ORIENTED_EDGE('',*,*,#17523,.F.);
#23207=ORIENTED_EDGE('',*,*,#17524,.T.);
#23208=ORIENTED_EDGE('',*,*,#17281,.F.);
#23209=ORIENTED_EDGE('',*,*,#17524,.F.);
#23210=ORIENTED_EDGE('',*,*,#17525,.F.);
#23211=ORIENTED_EDGE('',*,*,#17526,.T.);
#23212=ORIENTED_EDGE('',*,*,#17282,.F.);
#23213=ORIENTED_EDGE('',*,*,#17526,.F.);
#23214=ORIENTED_EDGE('',*,*,#17527,.F.);
#23215=ORIENTED_EDGE('',*,*,#17528,.T.);
#23216=ORIENTED_EDGE('',*,*,#17505,.F.);
#23217=ORIENTED_EDGE('',*,*,#17529,.T.);
#23218=ORIENTED_EDGE('',*,*,#17530,.T.);
#23219=ORIENTED_EDGE('',*,*,#17529,.F.);
#23220=ORIENTED_EDGE('',*,*,#17530,.F.);
#23221=ORIENTED_EDGE('',*,*,#17527,.T.);
#23222=ORIENTED_EDGE('',*,*,#17525,.T.);
#23223=ORIENTED_EDGE('',*,*,#17523,.T.);
#23224=ORIENTED_EDGE('',*,*,#17521,.T.);
#23225=ORIENTED_EDGE('',*,*,#17519,.T.);
#23226=ORIENTED_EDGE('',*,*,#17517,.T.);
#23227=ORIENTED_EDGE('',*,*,#17515,.T.);
#23228=ORIENTED_EDGE('',*,*,#17513,.T.);
#23229=ORIENTED_EDGE('',*,*,#17509,.T.);
#23230=ORIENTED_EDGE('',*,*,#17507,.T.);
#23231=ORIENTED_EDGE('',*,*,#17512,.T.);
#23232=ORIENTED_EDGE('',*,*,#17531,.T.);
#23233=ORIENTED_EDGE('',*,*,#17283,.F.);
#23234=ORIENTED_EDGE('',*,*,#17528,.F.);
#23235=ORIENTED_EDGE('',*,*,#17531,.F.);
#23236=ORIENTED_EDGE('',*,*,#17511,.T.);
#23237=ORIENTED_EDGE('',*,*,#17295,.F.);
#23238=ORIENTED_EDGE('',*,*,#17291,.T.);
#23239=ORIENTED_EDGE('',*,*,#17287,.T.);
#23240=ORIENTED_EDGE('',*,*,#17532,.T.);
#23241=ORIENTED_EDGE('',*,*,#17533,.T.);
#23242=ORIENTED_EDGE('',*,*,#17534,.T.);
#23243=ORIENTED_EDGE('',*,*,#17535,.T.);
#23244=ORIENTED_EDGE('',*,*,#17536,.T.);
#23245=ORIENTED_EDGE('',*,*,#17537,.T.);
#23246=ORIENTED_EDGE('',*,*,#17538,.T.);
#23247=ORIENTED_EDGE('',*,*,#17539,.T.);
#23248=ORIENTED_EDGE('',*,*,#17540,.T.);
#23249=ORIENTED_EDGE('',*,*,#17541,.T.);
#23250=ORIENTED_EDGE('',*,*,#17289,.T.);
#23251=ORIENTED_EDGE('',*,*,#17293,.T.);
#23252=ORIENTED_EDGE('',*,*,#17542,.T.);
#23253=ORIENTED_EDGE('',*,*,#17543,.T.);
#23254=ORIENTED_EDGE('',*,*,#17544,.T.);
#23255=ORIENTED_EDGE('',*,*,#17545,.T.);
#23256=ORIENTED_EDGE('',*,*,#17546,.T.);
#23257=ORIENTED_EDGE('',*,*,#17547,.T.);
#23258=ORIENTED_EDGE('',*,*,#17548,.T.);
#23259=ORIENTED_EDGE('',*,*,#17549,.T.);
#23260=ORIENTED_EDGE('',*,*,#17550,.T.);
#23261=ORIENTED_EDGE('',*,*,#17551,.T.);
#23262=ORIENTED_EDGE('',*,*,#17532,.F.);
#23263=ORIENTED_EDGE('',*,*,#17290,.F.);
#23264=ORIENTED_EDGE('',*,*,#17551,.F.);
#23265=ORIENTED_EDGE('',*,*,#17552,.T.);
#23266=ORIENTED_EDGE('',*,*,#17533,.F.);
#23267=ORIENTED_EDGE('',*,*,#17552,.F.);
#23268=ORIENTED_EDGE('',*,*,#17550,.F.);
#23269=ORIENTED_EDGE('',*,*,#17553,.T.);
#23270=ORIENTED_EDGE('',*,*,#17534,.F.);
#23271=ORIENTED_EDGE('',*,*,#17553,.F.);
#23272=ORIENTED_EDGE('',*,*,#17549,.F.);
#23273=ORIENTED_EDGE('',*,*,#17554,.T.);
#23274=ORIENTED_EDGE('',*,*,#17535,.F.);
#23275=ORIENTED_EDGE('',*,*,#17554,.F.);
#23276=ORIENTED_EDGE('',*,*,#17548,.F.);
#23277=ORIENTED_EDGE('',*,*,#17555,.T.);
#23278=ORIENTED_EDGE('',*,*,#17556,.T.);
#23279=ORIENTED_EDGE('',*,*,#17536,.F.);
#23280=ORIENTED_EDGE('',*,*,#17555,.F.);
#23281=ORIENTED_EDGE('',*,*,#17547,.F.);
#23282=ORIENTED_EDGE('',*,*,#17537,.F.);
#23283=ORIENTED_EDGE('',*,*,#17556,.F.);
#23284=ORIENTED_EDGE('',*,*,#17546,.F.);
#23285=ORIENTED_EDGE('',*,*,#17557,.T.);
#23286=ORIENTED_EDGE('',*,*,#17538,.F.);
#23287=ORIENTED_EDGE('',*,*,#17557,.F.);
#23288=ORIENTED_EDGE('',*,*,#17545,.F.);
#23289=ORIENTED_EDGE('',*,*,#17558,.T.);
#23290=ORIENTED_EDGE('',*,*,#17539,.F.);
#23291=ORIENTED_EDGE('',*,*,#17558,.F.);
#23292=ORIENTED_EDGE('',*,*,#17544,.F.);
#23293=ORIENTED_EDGE('',*,*,#17559,.T.);
#23294=ORIENTED_EDGE('',*,*,#17540,.F.);
#23295=ORIENTED_EDGE('',*,*,#17559,.F.);
#23296=ORIENTED_EDGE('',*,*,#17543,.F.);
#23297=ORIENTED_EDGE('',*,*,#17560,.T.);
#23298=ORIENTED_EDGE('',*,*,#17541,.F.);
#23299=ORIENTED_EDGE('',*,*,#17560,.F.);
#23300=ORIENTED_EDGE('',*,*,#17542,.F.);
#23301=ORIENTED_EDGE('',*,*,#17292,.T.);
#23302=ORIENTED_EDGE('',*,*,#17561,.T.);
#23303=ORIENTED_EDGE('',*,*,#17562,.F.);
#23304=ORIENTED_EDGE('',*,*,#17563,.T.);
#23305=ORIENTED_EDGE('',*,*,#17564,.T.);
#23306=ORIENTED_EDGE('',*,*,#17565,.F.);
#23307=ORIENTED_EDGE('',*,*,#17566,.F.);
#23308=ORIENTED_EDGE('',*,*,#17564,.F.);
#23309=ORIENTED_EDGE('',*,*,#17567,.T.);
#23310=ORIENTED_EDGE('',*,*,#17568,.F.);
#23311=ORIENTED_EDGE('',*,*,#17569,.F.);
#23312=ORIENTED_EDGE('',*,*,#17570,.T.);
#23313=ORIENTED_EDGE('',*,*,#17571,.T.);
#23314=ORIENTED_EDGE('',*,*,#17572,.F.);
#23315=ORIENTED_EDGE('',*,*,#17573,.F.);
#23316=ORIENTED_EDGE('',*,*,#17571,.F.);
#23317=ORIENTED_EDGE('',*,*,#17574,.T.);
#23318=ORIENTED_EDGE('',*,*,#17575,.F.);
#23319=ORIENTED_EDGE('',*,*,#17576,.F.);
#23320=ORIENTED_EDGE('',*,*,#17577,.F.);
#23321=ORIENTED_EDGE('',*,*,#17578,.T.);
#23322=ORIENTED_EDGE('',*,*,#17579,.T.);
#23323=ORIENTED_EDGE('',*,*,#17580,.F.);
#23324=ORIENTED_EDGE('',*,*,#17579,.F.);
#23325=ORIENTED_EDGE('',*,*,#17581,.T.);
#23326=ORIENTED_EDGE('',*,*,#17575,.T.);
#23327=ORIENTED_EDGE('',*,*,#17582,.T.);
#23328=ORIENTED_EDGE('',*,*,#17580,.T.);
#23329=ORIENTED_EDGE('',*,*,#17582,.F.);
#23330=ORIENTED_EDGE('',*,*,#17577,.T.);
#23331=ORIENTED_EDGE('',*,*,#17576,.T.);
#23332=ORIENTED_EDGE('',*,*,#17583,.F.);
#23333=ORIENTED_EDGE('',*,*,#17584,.F.);
#23334=ORIENTED_EDGE('',*,*,#17583,.T.);
#23335=ORIENTED_EDGE('',*,*,#17585,.T.);
#23336=ORIENTED_EDGE('',*,*,#17565,.T.);
#23337=ORIENTED_EDGE('',*,*,#17566,.T.);
#23338=ORIENTED_EDGE('',*,*,#17585,.F.);
#23339=ORIENTED_EDGE('',*,*,#17584,.T.);
#23340=ORIENTED_EDGE('',*,*,#17568,.T.);
#23341=ORIENTED_EDGE('',*,*,#17586,.T.);
#23342=ORIENTED_EDGE('',*,*,#17572,.T.);
#23343=ORIENTED_EDGE('',*,*,#17573,.T.);
#23344=ORIENTED_EDGE('',*,*,#17586,.F.);
#23345=ORIENTED_EDGE('',*,*,#17569,.T.);
#23346=ORIENTED_EDGE('',*,*,#17587,.F.);
#23347=ORIENTED_EDGE('',*,*,#17588,.F.);
#23348=ORIENTED_EDGE('',*,*,#17589,.T.);
#23349=ORIENTED_EDGE('',*,*,#17590,.T.);
#23350=ORIENTED_EDGE('',*,*,#17589,.F.);
#23351=ORIENTED_EDGE('',*,*,#17587,.T.);
#23352=ORIENTED_EDGE('',*,*,#17588,.T.);
#23353=ORIENTED_EDGE('',*,*,#17591,.T.);
#23354=ORIENTED_EDGE('',*,*,#17561,.F.);
#23355=ORIENTED_EDGE('',*,*,#17591,.F.);
#23356=ORIENTED_EDGE('',*,*,#17570,.F.);
#23357=ORIENTED_EDGE('',*,*,#17574,.F.);
#23358=ORIENTED_EDGE('',*,*,#17578,.F.);
#23359=ORIENTED_EDGE('',*,*,#17581,.F.);
#23360=ORIENTED_EDGE('',*,*,#17563,.F.);
#23361=ORIENTED_EDGE('',*,*,#17567,.F.);
#23362=ORIENTED_EDGE('',*,*,#17590,.F.);
#23363=ORIENTED_EDGE('',*,*,#17592,.T.);
#23364=ORIENTED_EDGE('',*,*,#17562,.T.);
#23365=ORIENTED_EDGE('',*,*,#17593,.T.);
#23366=ORIENTED_EDGE('',*,*,#17594,.F.);
#23367=ORIENTED_EDGE('',*,*,#17595,.F.);
#23368=ORIENTED_EDGE('',*,*,#17593,.F.);
#23369=ORIENTED_EDGE('',*,*,#17497,.T.);
#23370=ORIENTED_EDGE('',*,*,#17493,.T.);
#23371=ORIENTED_EDGE('',*,*,#17504,.T.);
#23372=ORIENTED_EDGE('',*,*,#17502,.T.);
#23373=ORIENTED_EDGE('',*,*,#17247,.T.);
#23374=ORIENTED_EDGE('',*,*,#17501,.T.);
#23375=ORIENTED_EDGE('',*,*,#17253,.T.);
#23376=ORIENTED_EDGE('',*,*,#17250,.T.);
#23377=ORIENTED_EDGE('',*,*,#17498,.T.);
#23378=ORIENTED_EDGE('',*,*,#17485,.T.);
#23379=ORIENTED_EDGE('',*,*,#17489,.T.);
#23380=ORIENTED_EDGE('',*,*,#17490,.T.);
#23381=ORIENTED_EDGE('',*,*,#17244,.T.);
#23382=ORIENTED_EDGE('',*,*,#17491,.T.);
#23383=ORIENTED_EDGE('',*,*,#17258,.T.);
#23384=ORIENTED_EDGE('',*,*,#17336,.T.);
#23385=ORIENTED_EDGE('',*,*,#17596,.T.);
#23386=ORIENTED_EDGE('',*,*,#17597,.F.);
#23387=ORIENTED_EDGE('',*,*,#17598,.F.);
#23388=ORIENTED_EDGE('',*,*,#17599,.T.);
#23389=ORIENTED_EDGE('',*,*,#17600,.T.);
#23390=ORIENTED_EDGE('',*,*,#17601,.T.);
#23391=ORIENTED_EDGE('',*,*,#17602,.T.);
#23392=ORIENTED_EDGE('',*,*,#17603,.T.);
#23393=ORIENTED_EDGE('',*,*,#17604,.T.);
#23394=ORIENTED_EDGE('',*,*,#17605,.T.);
#23395=ORIENTED_EDGE('',*,*,#17606,.T.);
#23396=ORIENTED_EDGE('',*,*,#17607,.T.);
#23397=ORIENTED_EDGE('',*,*,#17608,.T.);
#23398=ORIENTED_EDGE('',*,*,#17609,.T.);
#23399=ORIENTED_EDGE('',*,*,#17610,.T.);
#23400=ORIENTED_EDGE('',*,*,#17611,.T.);
#23401=ORIENTED_EDGE('',*,*,#17612,.T.);
#23402=ORIENTED_EDGE('',*,*,#17613,.T.);
#23403=ORIENTED_EDGE('',*,*,#17614,.T.);
#23404=ORIENTED_EDGE('',*,*,#17598,.T.);
#23405=ORIENTED_EDGE('',*,*,#17615,.T.);
#23406=ORIENTED_EDGE('',*,*,#17599,.F.);
#23407=ORIENTED_EDGE('',*,*,#17614,.F.);
#23408=ORIENTED_EDGE('',*,*,#17616,.T.);
#23409=ORIENTED_EDGE('',*,*,#17617,.F.);
#23410=ORIENTED_EDGE('',*,*,#17618,.T.);
#23411=ORIENTED_EDGE('',*,*,#17619,.T.);
#23412=ORIENTED_EDGE('',*,*,#17620,.F.);
#23413=ORIENTED_EDGE('',*,*,#17621,.T.);
#23414=ORIENTED_EDGE('',*,*,#17622,.F.);
#23415=ORIENTED_EDGE('',*,*,#17623,.T.);
#23416=ORIENTED_EDGE('',*,*,#17624,.T.);
#23417=ORIENTED_EDGE('',*,*,#17625,.T.);
#23418=ORIENTED_EDGE('',*,*,#17626,.F.);
#23419=ORIENTED_EDGE('',*,*,#17627,.F.);
#23420=ORIENTED_EDGE('',*,*,#17628,.F.);
#23421=ORIENTED_EDGE('',*,*,#17629,.T.);
#23422=ORIENTED_EDGE('',*,*,#17630,.T.);
#23423=ORIENTED_EDGE('',*,*,#17631,.T.);
#23424=ORIENTED_EDGE('',*,*,#17632,.T.);
#23425=ORIENTED_EDGE('',*,*,#17633,.F.);
#23426=ORIENTED_EDGE('',*,*,#17634,.T.);
#23427=ORIENTED_EDGE('',*,*,#17635,.T.);
#23428=ORIENTED_EDGE('',*,*,#17636,.T.);
#23429=ORIENTED_EDGE('',*,*,#17637,.F.);
#23430=ORIENTED_EDGE('',*,*,#17638,.F.);
#23431=ORIENTED_EDGE('',*,*,#17632,.F.);
#23432=ORIENTED_EDGE('',*,*,#17639,.T.);
#23433=ORIENTED_EDGE('',*,*,#17640,.F.);
#23434=ORIENTED_EDGE('',*,*,#17639,.F.);
#23435=ORIENTED_EDGE('',*,*,#17631,.F.);
#23436=ORIENTED_EDGE('',*,*,#17641,.T.);
#23437=ORIENTED_EDGE('',*,*,#17642,.F.);
#23438=ORIENTED_EDGE('',*,*,#17641,.F.);
#23439=ORIENTED_EDGE('',*,*,#17630,.F.);
#23440=ORIENTED_EDGE('',*,*,#17643,.T.);
#23441=ORIENTED_EDGE('',*,*,#17644,.F.);
#23442=ORIENTED_EDGE('',*,*,#17643,.F.);
#23443=ORIENTED_EDGE('',*,*,#17629,.F.);
#23444=ORIENTED_EDGE('',*,*,#17638,.T.);
#23445=ORIENTED_EDGE('',*,*,#17645,.T.);
#23446=ORIENTED_EDGE('',*,*,#17646,.T.);
#23447=ORIENTED_EDGE('',*,*,#17647,.T.);
#23448=ORIENTED_EDGE('',*,*,#17648,.T.);
#23449=ORIENTED_EDGE('',*,*,#17649,.F.);
#23450=ORIENTED_EDGE('',*,*,#17628,.T.);
#23451=ORIENTED_EDGE('',*,*,#17650,.T.);
#23452=ORIENTED_EDGE('',*,*,#17620,.T.);
#23453=ORIENTED_EDGE('',*,*,#17651,.F.);
#23454=ORIENTED_EDGE('',*,*,#17652,.F.);
#23455=ORIENTED_EDGE('',*,*,#17648,.F.);
#23456=ORIENTED_EDGE('',*,*,#17653,.T.);
#23457=ORIENTED_EDGE('',*,*,#17654,.F.);
#23458=ORIENTED_EDGE('',*,*,#17653,.F.);
#23459=ORIENTED_EDGE('',*,*,#17647,.F.);
#23460=ORIENTED_EDGE('',*,*,#17655,.T.);
#23461=ORIENTED_EDGE('',*,*,#17656,.F.);
#23462=ORIENTED_EDGE('',*,*,#17655,.F.);
#23463=ORIENTED_EDGE('',*,*,#17646,.F.);
#23464=ORIENTED_EDGE('',*,*,#17657,.T.);
#23465=ORIENTED_EDGE('',*,*,#17658,.F.);
#23466=ORIENTED_EDGE('',*,*,#17657,.F.);
#23467=ORIENTED_EDGE('',*,*,#17645,.F.);
#23468=ORIENTED_EDGE('',*,*,#17652,.T.);
#23469=ORIENTED_EDGE('',*,*,#17659,.F.);
#23470=ORIENTED_EDGE('',*,*,#17659,.T.);
#23471=ORIENTED_EDGE('',*,*,#17660,.T.);
#23472=ORIENTED_EDGE('',*,*,#17661,.F.);
#23473=ORIENTED_EDGE('',*,*,#17662,.F.);
#23474=ORIENTED_EDGE('',*,*,#17660,.F.);
#23475=ORIENTED_EDGE('',*,*,#17662,.T.);
#23476=ORIENTED_EDGE('',*,*,#17663,.T.);
#23477=ORIENTED_EDGE('',*,*,#17664,.F.);
#23478=ORIENTED_EDGE('',*,*,#17663,.F.);
#23479=ORIENTED_EDGE('',*,*,#17661,.T.);
#23480=ORIENTED_EDGE('',*,*,#17665,.F.);
#23481=ORIENTED_EDGE('',*,*,#17665,.T.);
#23482=ORIENTED_EDGE('',*,*,#17666,.T.);
#23483=ORIENTED_EDGE('',*,*,#17667,.F.);
#23484=ORIENTED_EDGE('',*,*,#17668,.F.);
#23485=ORIENTED_EDGE('',*,*,#17666,.F.);
#23486=ORIENTED_EDGE('',*,*,#17668,.T.);
#23487=ORIENTED_EDGE('',*,*,#17669,.T.);
#23488=ORIENTED_EDGE('',*,*,#17670,.F.);
#23489=ORIENTED_EDGE('',*,*,#17669,.F.);
#23490=ORIENTED_EDGE('',*,*,#17667,.T.);
#23491=ORIENTED_EDGE('',*,*,#17671,.F.);
#23492=ORIENTED_EDGE('',*,*,#17671,.T.);
#23493=ORIENTED_EDGE('',*,*,#17672,.T.);
#23494=ORIENTED_EDGE('',*,*,#17673,.F.);
#23495=ORIENTED_EDGE('',*,*,#17674,.F.);
#23496=ORIENTED_EDGE('',*,*,#17672,.F.);
#23497=ORIENTED_EDGE('',*,*,#17674,.T.);
#23498=ORIENTED_EDGE('',*,*,#17675,.T.);
#23499=ORIENTED_EDGE('',*,*,#17676,.F.);
#23500=ORIENTED_EDGE('',*,*,#17675,.F.);
#23501=ORIENTED_EDGE('',*,*,#17673,.T.);
#23502=ORIENTED_EDGE('',*,*,#17677,.F.);
#23503=ORIENTED_EDGE('',*,*,#17677,.T.);
#23504=ORIENTED_EDGE('',*,*,#17678,.T.);
#23505=ORIENTED_EDGE('',*,*,#17679,.F.);
#23506=ORIENTED_EDGE('',*,*,#17680,.F.);
#23507=ORIENTED_EDGE('',*,*,#17678,.F.);
#23508=ORIENTED_EDGE('',*,*,#17680,.T.);
#23509=ORIENTED_EDGE('',*,*,#17681,.T.);
#23510=ORIENTED_EDGE('',*,*,#17682,.F.);
#23511=ORIENTED_EDGE('',*,*,#17681,.F.);
#23512=ORIENTED_EDGE('',*,*,#17679,.T.);
#23513=ORIENTED_EDGE('',*,*,#17595,.T.);
#23514=ORIENTED_EDGE('',*,*,#17683,.T.);
#23515=ORIENTED_EDGE('',*,*,#17684,.F.);
#23516=ORIENTED_EDGE('',*,*,#17683,.F.);
#23517=ORIENTED_EDGE('',*,*,#17594,.T.);
#23518=ORIENTED_EDGE('',*,*,#17684,.T.);
#23519=ORIENTED_EDGE('',*,*,#17685,.T.);
#23520=ORIENTED_EDGE('',*,*,#17686,.T.);
#23521=ORIENTED_EDGE('',*,*,#17687,.F.);
#23522=ORIENTED_EDGE('',*,*,#17688,.T.);
#23523=ORIENTED_EDGE('',*,*,#17664,.T.);
#23524=ORIENTED_EDGE('',*,*,#17670,.T.);
#23525=ORIENTED_EDGE('',*,*,#17676,.T.);
#23526=ORIENTED_EDGE('',*,*,#17682,.T.);
#23527=ORIENTED_EDGE('',*,*,#17689,.F.);
#23528=ORIENTED_EDGE('',*,*,#17689,.T.);
#23529=ORIENTED_EDGE('',*,*,#17690,.T.);
#23530=ORIENTED_EDGE('',*,*,#17691,.F.);
#23531=ORIENTED_EDGE('',*,*,#17690,.F.);
#23532=ORIENTED_EDGE('',*,*,#17691,.T.);
#23533=ORIENTED_EDGE('',*,*,#17692,.F.);
#23534=ORIENTED_EDGE('',*,*,#17692,.T.);
#23535=ORIENTED_EDGE('',*,*,#17693,.T.);
#23536=ORIENTED_EDGE('',*,*,#17694,.F.);
#23537=ORIENTED_EDGE('',*,*,#17693,.F.);
#23538=ORIENTED_EDGE('',*,*,#17694,.T.);
#23539=ORIENTED_EDGE('',*,*,#17642,.T.);
#23540=ORIENTED_EDGE('',*,*,#17644,.T.);
#23541=ORIENTED_EDGE('',*,*,#17637,.T.);
#23542=ORIENTED_EDGE('',*,*,#17640,.T.);
#23543=ORIENTED_EDGE('',*,*,#17656,.T.);
#23544=ORIENTED_EDGE('',*,*,#17658,.T.);
#23545=ORIENTED_EDGE('',*,*,#17651,.T.);
#23546=ORIENTED_EDGE('',*,*,#17654,.T.);
#23547=ORIENTED_EDGE('',*,*,#17695,.F.);
#23548=ORIENTED_EDGE('',*,*,#17695,.T.);
#23549=ORIENTED_EDGE('',*,*,#17696,.T.);
#23550=ORIENTED_EDGE('',*,*,#17697,.F.);
#23551=ORIENTED_EDGE('',*,*,#17696,.F.);
#23552=ORIENTED_EDGE('',*,*,#17697,.T.);
#23553=ORIENTED_EDGE('',*,*,#17698,.F.);
#23554=ORIENTED_EDGE('',*,*,#17698,.T.);
#23555=ORIENTED_EDGE('',*,*,#17699,.T.);
#23556=ORIENTED_EDGE('',*,*,#17592,.F.);
#23557=ORIENTED_EDGE('',*,*,#17699,.F.);
#23558=ORIENTED_EDGE('',*,*,#17700,.T.);
#23559=ORIENTED_EDGE('',*,*,#17701,.F.);
#23560=ORIENTED_EDGE('',*,*,#17685,.F.);
#23561=ORIENTED_EDGE('',*,*,#17702,.T.);
#23562=ORIENTED_EDGE('',*,*,#17700,.F.);
#23563=ORIENTED_EDGE('',*,*,#17702,.F.);
#23564=ORIENTED_EDGE('',*,*,#17701,.T.);
#23565=ORIENTED_EDGE('',*,*,#17703,.T.);
#23566=ORIENTED_EDGE('',*,*,#17704,.F.);
#23567=ORIENTED_EDGE('',*,*,#17703,.F.);
#23568=ORIENTED_EDGE('',*,*,#17704,.T.);
#23569=ORIENTED_EDGE('',*,*,#17705,.T.);
#23570=ORIENTED_EDGE('',*,*,#17706,.T.);
#23571=ORIENTED_EDGE('',*,*,#17688,.F.);
#23572=ORIENTED_EDGE('',*,*,#17706,.F.);
#23573=ORIENTED_EDGE('',*,*,#17705,.F.);
#23574=ORIENTED_EDGE('',*,*,#17707,.T.);
#23575=ORIENTED_EDGE('',*,*,#17708,.T.);
#23576=ORIENTED_EDGE('',*,*,#17709,.T.);
#23577=ORIENTED_EDGE('',*,*,#17707,.F.);
#23578=ORIENTED_EDGE('',*,*,#17709,.F.);
#23579=ORIENTED_EDGE('',*,*,#17708,.F.);
#23580=ORIENTED_EDGE('',*,*,#17710,.T.);
#23581=ORIENTED_EDGE('',*,*,#17711,.T.);
#23582=ORIENTED_EDGE('',*,*,#17712,.T.);
#23583=ORIENTED_EDGE('',*,*,#17710,.F.);
#23584=ORIENTED_EDGE('',*,*,#17712,.F.);
#23585=ORIENTED_EDGE('',*,*,#17713,.T.);
#23586=ORIENTED_EDGE('',*,*,#17711,.F.);
#23587=ORIENTED_EDGE('',*,*,#17687,.T.);
#23588=ORIENTED_EDGE('',*,*,#17714,.T.);
#23589=ORIENTED_EDGE('',*,*,#17713,.F.);
#23590=ORIENTED_EDGE('',*,*,#17714,.F.);
#23591=ORIENTED_EDGE('',*,*,#17715,.T.);
#23592=ORIENTED_EDGE('',*,*,#17716,.T.);
#23593=ORIENTED_EDGE('',*,*,#17686,.F.);
#23594=ORIENTED_EDGE('',*,*,#17716,.F.);
#23595=ORIENTED_EDGE('',*,*,#17715,.F.);
#23596=ORIENTED_EDGE('',*,*,#17717,.T.);
#23597=ORIENTED_EDGE('',*,*,#17718,.T.);
#23598=ORIENTED_EDGE('',*,*,#17719,.T.);
#23599=ORIENTED_EDGE('',*,*,#17717,.F.);
#23600=ORIENTED_EDGE('',*,*,#17719,.F.);
#23601=ORIENTED_EDGE('',*,*,#17718,.F.);
#23602=ORIENTED_EDGE('',*,*,#17720,.F.);
#23603=ORIENTED_EDGE('',*,*,#17721,.T.);
#23604=ORIENTED_EDGE('',*,*,#17722,.T.);
#23605=ORIENTED_EDGE('',*,*,#17636,.F.);
#23606=ORIENTED_EDGE('',*,*,#17723,.T.);
#23607=ORIENTED_EDGE('',*,*,#17724,.F.);
#23608=ORIENTED_EDGE('',*,*,#17725,.F.);
#23609=ORIENTED_EDGE('',*,*,#17726,.T.);
#23610=ORIENTED_EDGE('',*,*,#17720,.T.);
#23611=ORIENTED_EDGE('',*,*,#17727,.F.);
#23612=ORIENTED_EDGE('',*,*,#17728,.T.);
#23613=ORIENTED_EDGE('',*,*,#17729,.T.);
#23614=ORIENTED_EDGE('',*,*,#17725,.T.);
#23615=ORIENTED_EDGE('',*,*,#17730,.F.);
#23616=ORIENTED_EDGE('',*,*,#17731,.F.);
#23617=ORIENTED_EDGE('',*,*,#17634,.F.);
#23618=ORIENTED_EDGE('',*,*,#17622,.T.);
#23619=ORIENTED_EDGE('',*,*,#17732,.T.);
#23620=ORIENTED_EDGE('',*,*,#17626,.T.);
#23621=ORIENTED_EDGE('',*,*,#17733,.T.);
#23622=ORIENTED_EDGE('',*,*,#17734,.T.);
#23623=ORIENTED_EDGE('',*,*,#17735,.T.);
#23624=ORIENTED_EDGE('',*,*,#17617,.T.);
#23625=ORIENTED_EDGE('',*,*,#17733,.F.);
#23626=ORIENTED_EDGE('',*,*,#17625,.F.);
#23627=ORIENTED_EDGE('',*,*,#17627,.T.);
#23628=ORIENTED_EDGE('',*,*,#17732,.F.);
#23629=ORIENTED_EDGE('',*,*,#17621,.F.);
#23630=ORIENTED_EDGE('',*,*,#17650,.F.);
#23631=ORIENTED_EDGE('',*,*,#17731,.T.);
#23632=ORIENTED_EDGE('',*,*,#17736,.F.);
#23633=ORIENTED_EDGE('',*,*,#17723,.F.);
#23634=ORIENTED_EDGE('',*,*,#17635,.F.);
#23635=ORIENTED_EDGE('',*,*,#17730,.T.);
#23636=ORIENTED_EDGE('',*,*,#17727,.T.);
#23637=ORIENTED_EDGE('',*,*,#17724,.T.);
#23638=ORIENTED_EDGE('',*,*,#17736,.T.);
#23639=ORIENTED_EDGE('',*,*,#17737,.T.);
#23640=ORIENTED_EDGE('',*,*,#17728,.F.);
#23641=ORIENTED_EDGE('',*,*,#17738,.F.);
#23642=ORIENTED_EDGE('',*,*,#17722,.F.);
#23643=ORIENTED_EDGE('',*,*,#17739,.T.);
#23644=ORIENTED_EDGE('',*,*,#17737,.F.);
#23645=ORIENTED_EDGE('',*,*,#17740,.T.);
#23646=ORIENTED_EDGE('',*,*,#17741,.F.);
#23647=ORIENTED_EDGE('',*,*,#17740,.F.);
#23648=ORIENTED_EDGE('',*,*,#17739,.F.);
#23649=ORIENTED_EDGE('',*,*,#17721,.F.);
#23650=ORIENTED_EDGE('',*,*,#17726,.F.);
#23651=ORIENTED_EDGE('',*,*,#17729,.F.);
#23652=ORIENTED_EDGE('',*,*,#17741,.T.);
#23653=ORIENTED_EDGE('',*,*,#17738,.T.);
#23654=ORIENTED_EDGE('',*,*,#17633,.T.);
#23655=ORIENTED_EDGE('',*,*,#17742,.F.);
#23656=ORIENTED_EDGE('',*,*,#17743,.F.);
#23657=ORIENTED_EDGE('',*,*,#17744,.F.);
#23658=ORIENTED_EDGE('',*,*,#17745,.F.);
#23659=ORIENTED_EDGE('',*,*,#17746,.F.);
#23660=ORIENTED_EDGE('',*,*,#17747,.F.);
#23661=ORIENTED_EDGE('',*,*,#17748,.F.);
#23662=ORIENTED_EDGE('',*,*,#17749,.F.);
#23663=ORIENTED_EDGE('',*,*,#17750,.F.);
#23664=ORIENTED_EDGE('',*,*,#17596,.F.);
#23665=ORIENTED_EDGE('',*,*,#17615,.F.);
#23666=ORIENTED_EDGE('',*,*,#17751,.F.);
#23667=ORIENTED_EDGE('',*,*,#17752,.F.);
#23668=ORIENTED_EDGE('',*,*,#17753,.F.);
#23669=ORIENTED_EDGE('',*,*,#17754,.F.);
#23670=ORIENTED_EDGE('',*,*,#17755,.F.);
#23671=ORIENTED_EDGE('',*,*,#17618,.F.);
#23672=ORIENTED_EDGE('',*,*,#17735,.F.);
#23673=ORIENTED_EDGE('',*,*,#17624,.F.);
#23674=ORIENTED_EDGE('',*,*,#17756,.F.);
#23675=ORIENTED_EDGE('',*,*,#17757,.T.);
#23676=ORIENTED_EDGE('',*,*,#17734,.F.);
#23677=ORIENTED_EDGE('',*,*,#17758,.T.);
#23678=ORIENTED_EDGE('',*,*,#17757,.F.);
#23679=ORIENTED_EDGE('',*,*,#17758,.F.);
#23680=ORIENTED_EDGE('',*,*,#17619,.F.);
#23681=ORIENTED_EDGE('',*,*,#17756,.T.);
#23682=ORIENTED_EDGE('',*,*,#17623,.F.);
#23683=ORIENTED_EDGE('',*,*,#17759,.F.);
#23684=ORIENTED_EDGE('',*,*,#17649,.T.);
#23685=ORIENTED_EDGE('',*,*,#17759,.T.);
#23686=ORIENTED_EDGE('',*,*,#17760,.F.);
#23687=ORIENTED_EDGE('',*,*,#17761,.F.);
#23688=ORIENTED_EDGE('',*,*,#17762,.F.);
#23689=ORIENTED_EDGE('',*,*,#17763,.F.);
#23690=ORIENTED_EDGE('',*,*,#17764,.F.);
#23691=ORIENTED_EDGE('',*,*,#17765,.F.);
#23692=ORIENTED_EDGE('',*,*,#17766,.F.);
#23693=ORIENTED_EDGE('',*,*,#17767,.F.);
#23694=ORIENTED_EDGE('',*,*,#17768,.F.);
#23695=ORIENTED_EDGE('',*,*,#17769,.F.);
#23696=ORIENTED_EDGE('',*,*,#17770,.F.);
#23697=ORIENTED_EDGE('',*,*,#17771,.F.);
#23698=ORIENTED_EDGE('',*,*,#17772,.F.);
#23699=ORIENTED_EDGE('',*,*,#17773,.F.);
#23700=ORIENTED_EDGE('',*,*,#17774,.F.);
#23701=ORIENTED_EDGE('',*,*,#17775,.F.);
#23702=ORIENTED_EDGE('',*,*,#17769,.T.);
#23703=ORIENTED_EDGE('',*,*,#17776,.F.);
#23704=ORIENTED_EDGE('',*,*,#17777,.F.);
#23705=ORIENTED_EDGE('',*,*,#17778,.T.);
#23706=ORIENTED_EDGE('',*,*,#17768,.T.);
#23707=ORIENTED_EDGE('',*,*,#17779,.F.);
#23708=ORIENTED_EDGE('',*,*,#17780,.F.);
#23709=ORIENTED_EDGE('',*,*,#17776,.T.);
#23710=ORIENTED_EDGE('',*,*,#17767,.T.);
#23711=ORIENTED_EDGE('',*,*,#17781,.F.);
#23712=ORIENTED_EDGE('',*,*,#17782,.F.);
#23713=ORIENTED_EDGE('',*,*,#17779,.T.);
#23714=ORIENTED_EDGE('',*,*,#17766,.T.);
#23715=ORIENTED_EDGE('',*,*,#17783,.F.);
#23716=ORIENTED_EDGE('',*,*,#17784,.F.);
#23717=ORIENTED_EDGE('',*,*,#17781,.T.);
#23718=ORIENTED_EDGE('',*,*,#17765,.T.);
#23719=ORIENTED_EDGE('',*,*,#17785,.F.);
#23720=ORIENTED_EDGE('',*,*,#17786,.F.);
#23721=ORIENTED_EDGE('',*,*,#17783,.T.);
#23722=ORIENTED_EDGE('',*,*,#17764,.T.);
#23723=ORIENTED_EDGE('',*,*,#17787,.F.);
#23724=ORIENTED_EDGE('',*,*,#17788,.F.);
#23725=ORIENTED_EDGE('',*,*,#17785,.T.);
#23726=ORIENTED_EDGE('',*,*,#17763,.T.);
#23727=ORIENTED_EDGE('',*,*,#17789,.F.);
#23728=ORIENTED_EDGE('',*,*,#17790,.F.);
#23729=ORIENTED_EDGE('',*,*,#17787,.T.);
#23730=ORIENTED_EDGE('',*,*,#17762,.T.);
#23731=ORIENTED_EDGE('',*,*,#17791,.F.);
#23732=ORIENTED_EDGE('',*,*,#17792,.F.);
#23733=ORIENTED_EDGE('',*,*,#17789,.T.);
#23734=ORIENTED_EDGE('',*,*,#17761,.T.);
#23735=ORIENTED_EDGE('',*,*,#17793,.F.);
#23736=ORIENTED_EDGE('',*,*,#17794,.F.);
#23737=ORIENTED_EDGE('',*,*,#17791,.T.);
#23738=ORIENTED_EDGE('',*,*,#17793,.T.);
#23739=ORIENTED_EDGE('',*,*,#17760,.T.);
#23740=ORIENTED_EDGE('',*,*,#17795,.F.);
#23741=ORIENTED_EDGE('',*,*,#17796,.F.);
#23742=ORIENTED_EDGE('',*,*,#17775,.T.);
#23743=ORIENTED_EDGE('',*,*,#17797,.F.);
#23744=ORIENTED_EDGE('',*,*,#17798,.F.);
#23745=ORIENTED_EDGE('',*,*,#17795,.T.);
#23746=ORIENTED_EDGE('',*,*,#17774,.T.);
#23747=ORIENTED_EDGE('',*,*,#17799,.F.);
#23748=ORIENTED_EDGE('',*,*,#17800,.F.);
#23749=ORIENTED_EDGE('',*,*,#17797,.T.);
#23750=ORIENTED_EDGE('',*,*,#17773,.T.);
#23751=ORIENTED_EDGE('',*,*,#17801,.F.);
#23752=ORIENTED_EDGE('',*,*,#17802,.F.);
#23753=ORIENTED_EDGE('',*,*,#17799,.T.);
#23754=ORIENTED_EDGE('',*,*,#17772,.T.);
#23755=ORIENTED_EDGE('',*,*,#17803,.F.);
#23756=ORIENTED_EDGE('',*,*,#17804,.F.);
#23757=ORIENTED_EDGE('',*,*,#17801,.T.);
#23758=ORIENTED_EDGE('',*,*,#17771,.T.);
#23759=ORIENTED_EDGE('',*,*,#17805,.F.);
#23760=ORIENTED_EDGE('',*,*,#17806,.F.);
#23761=ORIENTED_EDGE('',*,*,#17803,.T.);
#23762=ORIENTED_EDGE('',*,*,#17770,.T.);
#23763=ORIENTED_EDGE('',*,*,#17778,.F.);
#23764=ORIENTED_EDGE('',*,*,#17807,.F.);
#23765=ORIENTED_EDGE('',*,*,#17805,.T.);
#23766=ORIENTED_EDGE('',*,*,#17777,.T.);
#23767=ORIENTED_EDGE('',*,*,#17780,.T.);
#23768=ORIENTED_EDGE('',*,*,#17782,.T.);
#23769=ORIENTED_EDGE('',*,*,#17784,.T.);
#23770=ORIENTED_EDGE('',*,*,#17786,.T.);
#23771=ORIENTED_EDGE('',*,*,#17788,.T.);
#23772=ORIENTED_EDGE('',*,*,#17790,.T.);
#23773=ORIENTED_EDGE('',*,*,#17792,.T.);
#23774=ORIENTED_EDGE('',*,*,#17794,.T.);
#23775=ORIENTED_EDGE('',*,*,#17796,.T.);
#23776=ORIENTED_EDGE('',*,*,#17798,.T.);
#23777=ORIENTED_EDGE('',*,*,#17800,.T.);
#23778=ORIENTED_EDGE('',*,*,#17802,.T.);
#23779=ORIENTED_EDGE('',*,*,#17804,.T.);
#23780=ORIENTED_EDGE('',*,*,#17806,.T.);
#23781=ORIENTED_EDGE('',*,*,#17807,.T.);
#23782=ORIENTED_EDGE('',*,*,#17750,.T.);
#23783=ORIENTED_EDGE('',*,*,#17808,.F.);
#23784=ORIENTED_EDGE('',*,*,#17600,.F.);
#23785=ORIENTED_EDGE('',*,*,#17597,.T.);
#23786=ORIENTED_EDGE('',*,*,#17749,.T.);
#23787=ORIENTED_EDGE('',*,*,#17809,.F.);
#23788=ORIENTED_EDGE('',*,*,#17601,.F.);
#23789=ORIENTED_EDGE('',*,*,#17808,.T.);
#23790=ORIENTED_EDGE('',*,*,#17748,.T.);
#23791=ORIENTED_EDGE('',*,*,#17810,.F.);
#23792=ORIENTED_EDGE('',*,*,#17602,.F.);
#23793=ORIENTED_EDGE('',*,*,#17809,.T.);
#23794=ORIENTED_EDGE('',*,*,#17747,.T.);
#23795=ORIENTED_EDGE('',*,*,#17811,.F.);
#23796=ORIENTED_EDGE('',*,*,#17603,.F.);
#23797=ORIENTED_EDGE('',*,*,#17810,.T.);
#23798=ORIENTED_EDGE('',*,*,#17746,.T.);
#23799=ORIENTED_EDGE('',*,*,#17812,.F.);
#23800=ORIENTED_EDGE('',*,*,#17604,.F.);
#23801=ORIENTED_EDGE('',*,*,#17811,.T.);
#23802=ORIENTED_EDGE('',*,*,#17745,.T.);
#23803=ORIENTED_EDGE('',*,*,#17813,.F.);
#23804=ORIENTED_EDGE('',*,*,#17605,.F.);
#23805=ORIENTED_EDGE('',*,*,#17812,.T.);
#23806=ORIENTED_EDGE('',*,*,#17744,.T.);
#23807=ORIENTED_EDGE('',*,*,#17814,.F.);
#23808=ORIENTED_EDGE('',*,*,#17606,.F.);
#23809=ORIENTED_EDGE('',*,*,#17813,.T.);
#23810=ORIENTED_EDGE('',*,*,#17743,.T.);
#23811=ORIENTED_EDGE('',*,*,#17815,.F.);
#23812=ORIENTED_EDGE('',*,*,#17607,.F.);
#23813=ORIENTED_EDGE('',*,*,#17814,.T.);
#23814=ORIENTED_EDGE('',*,*,#17815,.T.);
#23815=ORIENTED_EDGE('',*,*,#17742,.T.);
#23816=ORIENTED_EDGE('',*,*,#17816,.F.);
#23817=ORIENTED_EDGE('',*,*,#17608,.F.);
#23818=ORIENTED_EDGE('',*,*,#17755,.T.);
#23819=ORIENTED_EDGE('',*,*,#17817,.F.);
#23820=ORIENTED_EDGE('',*,*,#17609,.F.);
#23821=ORIENTED_EDGE('',*,*,#17816,.T.);
#23822=ORIENTED_EDGE('',*,*,#17754,.T.);
#23823=ORIENTED_EDGE('',*,*,#17818,.F.);
#23824=ORIENTED_EDGE('',*,*,#17610,.F.);
#23825=ORIENTED_EDGE('',*,*,#17817,.T.);
#23826=ORIENTED_EDGE('',*,*,#17753,.T.);
#23827=ORIENTED_EDGE('',*,*,#17819,.F.);
#23828=ORIENTED_EDGE('',*,*,#17611,.F.);
#23829=ORIENTED_EDGE('',*,*,#17818,.T.);
#23830=ORIENTED_EDGE('',*,*,#17752,.T.);
#23831=ORIENTED_EDGE('',*,*,#17820,.F.);
#23832=ORIENTED_EDGE('',*,*,#17612,.F.);
#23833=ORIENTED_EDGE('',*,*,#17819,.T.);
#23834=ORIENTED_EDGE('',*,*,#17751,.T.);
#23835=ORIENTED_EDGE('',*,*,#17616,.F.);
#23836=ORIENTED_EDGE('',*,*,#17613,.F.);
#23837=ORIENTED_EDGE('',*,*,#17820,.T.);
#23838=ORIENTED_EDGE('',*,*,#17821,.T.);
#23839=ORIENTED_EDGE('',*,*,#17822,.T.);
#23840=ORIENTED_EDGE('',*,*,#17823,.T.);
#23841=ORIENTED_EDGE('',*,*,#17824,.T.);
#23842=ORIENTED_EDGE('',*,*,#17822,.F.);
#23843=ORIENTED_EDGE('',*,*,#17825,.T.);
#23844=ORIENTED_EDGE('',*,*,#17826,.T.);
#23845=ORIENTED_EDGE('',*,*,#17827,.F.);
#23846=ORIENTED_EDGE('',*,*,#17828,.T.);
#23847=ORIENTED_EDGE('',*,*,#17829,.T.);
#23848=ORIENTED_EDGE('',*,*,#17830,.F.);
#23849=ORIENTED_EDGE('',*,*,#17831,.T.);
#23850=ORIENTED_EDGE('',*,*,#17832,.T.);
#23851=ORIENTED_EDGE('',*,*,#17833,.F.);
#23852=ORIENTED_EDGE('',*,*,#17834,.T.);
#23853=ORIENTED_EDGE('',*,*,#17835,.T.);
#23854=ORIENTED_EDGE('',*,*,#17836,.F.);
#23855=ORIENTED_EDGE('',*,*,#17837,.F.);
#23856=ORIENTED_EDGE('',*,*,#17838,.T.);
#23857=ORIENTED_EDGE('',*,*,#17839,.T.);
#23858=ORIENTED_EDGE('',*,*,#17840,.T.);
#23859=ORIENTED_EDGE('',*,*,#17841,.T.);
#23860=ORIENTED_EDGE('',*,*,#17842,.F.);
#23861=ORIENTED_EDGE('',*,*,#17843,.F.);
#23862=ORIENTED_EDGE('',*,*,#17844,.T.);
#23863=ORIENTED_EDGE('',*,*,#17845,.T.);
#23864=ORIENTED_EDGE('',*,*,#17846,.T.);
#23865=ORIENTED_EDGE('',*,*,#17833,.T.);
#23866=ORIENTED_EDGE('',*,*,#17847,.F.);
#23867=ORIENTED_EDGE('',*,*,#17845,.F.);
#23868=ORIENTED_EDGE('',*,*,#17848,.T.);
#23869=ORIENTED_EDGE('',*,*,#17849,.T.);
#23870=ORIENTED_EDGE('',*,*,#17850,.F.);
#23871=ORIENTED_EDGE('',*,*,#17851,.F.);
#23872=ORIENTED_EDGE('',*,*,#17852,.F.);
#23873=ORIENTED_EDGE('',*,*,#17853,.F.);
#23874=ORIENTED_EDGE('',*,*,#17854,.F.);
#23875=ORIENTED_EDGE('',*,*,#17855,.F.);
#23876=ORIENTED_EDGE('',*,*,#17856,.F.);
#23877=ORIENTED_EDGE('',*,*,#17857,.F.);
#23878=ORIENTED_EDGE('',*,*,#17858,.F.);
#23879=ORIENTED_EDGE('',*,*,#17859,.T.);
#23880=ORIENTED_EDGE('',*,*,#17860,.F.);
#23881=ORIENTED_EDGE('',*,*,#17830,.T.);
#23882=ORIENTED_EDGE('',*,*,#17861,.F.);
#23883=ORIENTED_EDGE('',*,*,#17862,.T.);
#23884=ORIENTED_EDGE('',*,*,#17863,.T.);
#23885=ORIENTED_EDGE('',*,*,#17864,.T.);
#23886=ORIENTED_EDGE('',*,*,#17865,.F.);
#23887=ORIENTED_EDGE('',*,*,#17866,.T.);
#23888=ORIENTED_EDGE('',*,*,#17862,.F.);
#23889=ORIENTED_EDGE('',*,*,#17867,.F.);
#23890=ORIENTED_EDGE('',*,*,#17864,.F.);
#23891=ORIENTED_EDGE('',*,*,#17868,.T.);
#23892=ORIENTED_EDGE('',*,*,#17860,.T.);
#23893=ORIENTED_EDGE('',*,*,#17869,.T.);
#23894=ORIENTED_EDGE('',*,*,#17870,.T.);
#23895=ORIENTED_EDGE('',*,*,#17871,.F.);
#23896=ORIENTED_EDGE('',*,*,#17831,.F.);
#23897=ORIENTED_EDGE('',*,*,#17867,.T.);
#23898=ORIENTED_EDGE('',*,*,#17872,.T.);
#23899=ORIENTED_EDGE('',*,*,#17873,.F.);
#23900=ORIENTED_EDGE('',*,*,#17850,.T.);
#23901=ORIENTED_EDGE('',*,*,#17874,.T.);
#23902=ORIENTED_EDGE('',*,*,#17869,.F.);
#23903=ORIENTED_EDGE('',*,*,#17868,.F.);
#23904=ORIENTED_EDGE('',*,*,#17863,.F.);
#23905=ORIENTED_EDGE('',*,*,#17866,.F.);
#23906=ORIENTED_EDGE('',*,*,#17875,.F.);
#23907=ORIENTED_EDGE('',*,*,#17876,.F.);
#23908=ORIENTED_EDGE('',*,*,#17877,.F.);
#23909=ORIENTED_EDGE('',*,*,#17878,.F.);
#23910=ORIENTED_EDGE('',*,*,#17872,.F.);
#23911=ORIENTED_EDGE('',*,*,#17879,.T.);
#23912=ORIENTED_EDGE('',*,*,#17827,.T.);
#23913=ORIENTED_EDGE('',*,*,#17880,.T.);
#23914=ORIENTED_EDGE('',*,*,#17881,.T.);
#23915=ORIENTED_EDGE('',*,*,#17882,.F.);
#23916=ORIENTED_EDGE('',*,*,#17883,.F.);
#23917=ORIENTED_EDGE('',*,*,#17884,.F.);
#23918=ORIENTED_EDGE('',*,*,#17885,.F.);
#23919=ORIENTED_EDGE('',*,*,#17886,.F.);
#23920=ORIENTED_EDGE('',*,*,#17887,.F.);
#23921=ORIENTED_EDGE('',*,*,#17888,.F.);
#23922=ORIENTED_EDGE('',*,*,#17889,.F.);
#23923=ORIENTED_EDGE('',*,*,#17890,.F.);
#23924=ORIENTED_EDGE('',*,*,#17891,.F.);
#23925=ORIENTED_EDGE('',*,*,#17892,.F.);
#23926=ORIENTED_EDGE('',*,*,#17893,.F.);
#23927=ORIENTED_EDGE('',*,*,#17894,.F.);
#23928=ORIENTED_EDGE('',*,*,#17895,.F.);
#23929=ORIENTED_EDGE('',*,*,#17896,.F.);
#23930=ORIENTED_EDGE('',*,*,#17897,.F.);
#23931=ORIENTED_EDGE('',*,*,#17898,.F.);
#23932=ORIENTED_EDGE('',*,*,#17899,.F.);
#23933=ORIENTED_EDGE('',*,*,#17900,.T.);
#23934=ORIENTED_EDGE('',*,*,#17901,.F.);
#23935=ORIENTED_EDGE('',*,*,#17902,.F.);
#23936=ORIENTED_EDGE('',*,*,#17903,.F.);
#23937=ORIENTED_EDGE('',*,*,#17904,.F.);
#23938=ORIENTED_EDGE('',*,*,#17905,.F.);
#23939=ORIENTED_EDGE('',*,*,#17855,.T.);
#23940=ORIENTED_EDGE('',*,*,#17906,.F.);
#23941=ORIENTED_EDGE('',*,*,#17907,.F.);
#23942=ORIENTED_EDGE('',*,*,#17908,.F.);
#23943=ORIENTED_EDGE('',*,*,#17909,.F.);
#23944=ORIENTED_EDGE('',*,*,#17910,.F.);
#23945=ORIENTED_EDGE('',*,*,#17911,.F.);
#23946=ORIENTED_EDGE('',*,*,#17912,.F.);
#23947=ORIENTED_EDGE('',*,*,#17908,.T.);
#23948=ORIENTED_EDGE('',*,*,#17913,.T.);
#23949=ORIENTED_EDGE('',*,*,#17911,.T.);
#23950=ORIENTED_EDGE('',*,*,#17914,.T.);
#23951=ORIENTED_EDGE('',*,*,#17915,.T.);
#23952=ORIENTED_EDGE('',*,*,#17916,.T.);
#23953=ORIENTED_EDGE('',*,*,#17912,.T.);
#23954=ORIENTED_EDGE('',*,*,#17917,.T.);
#23955=ORIENTED_EDGE('',*,*,#17918,.F.);
#23956=ORIENTED_EDGE('',*,*,#17919,.F.);
#23957=ORIENTED_EDGE('',*,*,#17920,.F.);
#23958=ORIENTED_EDGE('',*,*,#17905,.T.);
#23959=ORIENTED_EDGE('',*,*,#17921,.T.);
#23960=ORIENTED_EDGE('',*,*,#17919,.T.);
#23961=ORIENTED_EDGE('',*,*,#17856,.T.);
#23962=ORIENTED_EDGE('',*,*,#17920,.T.);
#23963=ORIENTED_EDGE('',*,*,#17922,.T.);
#23964=ORIENTED_EDGE('',*,*,#17909,.T.);
#23965=ORIENTED_EDGE('',*,*,#17923,.T.);
#23966=ORIENTED_EDGE('',*,*,#17924,.F.);
#23967=ORIENTED_EDGE('',*,*,#17925,.F.);
#23968=ORIENTED_EDGE('',*,*,#17926,.F.);
#23969=ORIENTED_EDGE('',*,*,#17927,.T.);
#23970=ORIENTED_EDGE('',*,*,#17858,.T.);
#23971=ORIENTED_EDGE('',*,*,#17925,.T.);
#23972=ORIENTED_EDGE('',*,*,#17928,.T.);
#23973=ORIENTED_EDGE('',*,*,#17918,.T.);
#23974=ORIENTED_EDGE('',*,*,#17929,.T.);
#23975=ORIENTED_EDGE('',*,*,#17926,.T.);
#23976=ORIENTED_EDGE('',*,*,#17857,.T.);
#23977=ORIENTED_EDGE('',*,*,#17924,.T.);
#23978=ORIENTED_EDGE('',*,*,#17930,.T.);
#23979=ORIENTED_EDGE('',*,*,#17910,.T.);
#23980=ORIENTED_EDGE('',*,*,#17931,.T.);
#23981=ORIENTED_EDGE('',*,*,#17901,.T.);
#23982=ORIENTED_EDGE('',*,*,#17932,.T.);
#23983=ORIENTED_EDGE('',*,*,#17907,.T.);
#23984=ORIENTED_EDGE('',*,*,#17933,.T.);
#23985=ORIENTED_EDGE('',*,*,#17898,.T.);
#23986=ORIENTED_EDGE('',*,*,#17934,.T.);
#23987=ORIENTED_EDGE('',*,*,#17906,.T.);
#23988=ORIENTED_EDGE('',*,*,#17854,.T.);
#23989=ORIENTED_EDGE('',*,*,#17904,.T.);
#23990=ORIENTED_EDGE('',*,*,#17935,.T.);
#23991=ORIENTED_EDGE('',*,*,#17902,.T.);
#23992=ORIENTED_EDGE('',*,*,#17936,.T.);
#23993=ORIENTED_EDGE('',*,*,#17895,.T.);
#23994=ORIENTED_EDGE('',*,*,#17937,.T.);
#23995=ORIENTED_EDGE('',*,*,#17903,.T.);
#23996=ORIENTED_EDGE('',*,*,#17938,.T.);
#23997=ORIENTED_EDGE('',*,*,#17892,.T.);
#23998=ORIENTED_EDGE('',*,*,#17939,.T.);
#23999=ORIENTED_EDGE('',*,*,#17899,.T.);
#24000=ORIENTED_EDGE('',*,*,#17853,.T.);
#24001=ORIENTED_EDGE('',*,*,#17897,.T.);
#24002=ORIENTED_EDGE('',*,*,#17940,.T.);
#24003=ORIENTED_EDGE('',*,*,#17896,.T.);
#24004=ORIENTED_EDGE('',*,*,#17941,.T.);
#24005=ORIENTED_EDGE('',*,*,#17889,.T.);
#24006=ORIENTED_EDGE('',*,*,#17942,.T.);
#24007=ORIENTED_EDGE('',*,*,#17894,.T.);
#24008=ORIENTED_EDGE('',*,*,#17943,.T.);
#24009=ORIENTED_EDGE('',*,*,#17886,.T.);
#24010=ORIENTED_EDGE('',*,*,#17944,.T.);
#24011=ORIENTED_EDGE('',*,*,#17893,.T.);
#24012=ORIENTED_EDGE('',*,*,#17852,.T.);
#24013=ORIENTED_EDGE('',*,*,#17891,.T.);
#24014=ORIENTED_EDGE('',*,*,#17945,.T.);
#24015=ORIENTED_EDGE('',*,*,#17890,.T.);
#24016=ORIENTED_EDGE('',*,*,#17946,.T.);
#24017=ORIENTED_EDGE('',*,*,#17883,.T.);
#24018=ORIENTED_EDGE('',*,*,#17947,.T.);
#24019=ORIENTED_EDGE('',*,*,#17888,.T.);
#24020=ORIENTED_EDGE('',*,*,#17948,.T.);
#24021=ORIENTED_EDGE('',*,*,#17873,.T.);
#24022=ORIENTED_EDGE('',*,*,#17878,.T.);
#24023=ORIENTED_EDGE('',*,*,#17887,.T.);
#24024=ORIENTED_EDGE('',*,*,#17851,.T.);
#24025=ORIENTED_EDGE('',*,*,#17885,.T.);
#24026=ORIENTED_EDGE('',*,*,#17877,.T.);
#24027=ORIENTED_EDGE('',*,*,#17884,.T.);
#24028=ORIENTED_EDGE('',*,*,#17949,.T.);
#24029=ORIENTED_EDGE('',*,*,#17950,.T.);
#24030=ORIENTED_EDGE('',*,*,#17951,.T.);
#24031=ORIENTED_EDGE('',*,*,#17882,.T.);
#24032=ORIENTED_EDGE('',*,*,#17876,.T.);
#24033=ORIENTED_EDGE('',*,*,#17952,.T.);
#24034=ORIENTED_EDGE('',*,*,#17953,.T.);
#24035=ORIENTED_EDGE('',*,*,#17928,.F.);
#24036=ORIENTED_EDGE('',*,*,#17931,.F.);
#24037=ORIENTED_EDGE('',*,*,#17916,.F.);
#24038=ORIENTED_EDGE('',*,*,#17954,.T.);
#24039=ORIENTED_EDGE('',*,*,#17955,.F.);
#24040=ORIENTED_EDGE('',*,*,#17824,.F.);
#24041=ORIENTED_EDGE('',*,*,#17915,.F.);
#24042=ORIENTED_EDGE('',*,*,#17956,.F.);
#24043=ORIENTED_EDGE('',*,*,#17957,.F.);
#24044=ORIENTED_EDGE('',*,*,#17958,.F.);
#24045=ORIENTED_EDGE('',*,*,#17954,.F.);
#24046=ORIENTED_EDGE('',*,*,#17959,.T.);
#24047=ORIENTED_EDGE('',*,*,#17956,.T.);
#24048=ORIENTED_EDGE('',*,*,#17917,.F.);
#24049=ORIENTED_EDGE('',*,*,#17913,.F.);
#24050=ORIENTED_EDGE('',*,*,#17932,.F.);
#24051=ORIENTED_EDGE('',*,*,#17900,.F.);
#24052=ORIENTED_EDGE('',*,*,#17937,.F.);
#24053=ORIENTED_EDGE('',*,*,#17942,.F.);
#24054=ORIENTED_EDGE('',*,*,#17947,.F.);
#24055=ORIENTED_EDGE('',*,*,#17951,.F.);
#24056=ORIENTED_EDGE('',*,*,#17960,.T.);
#24057=ORIENTED_EDGE('',*,*,#17961,.T.);
#24058=ORIENTED_EDGE('',*,*,#17962,.F.);
#24059=ORIENTED_EDGE('',*,*,#17881,.F.);
#24060=ORIENTED_EDGE('',*,*,#17914,.F.);
#24061=ORIENTED_EDGE('',*,*,#17930,.F.);
#24062=ORIENTED_EDGE('',*,*,#17929,.F.);
#24063=ORIENTED_EDGE('',*,*,#17923,.F.);
#24064=ORIENTED_EDGE('',*,*,#17963,.F.);
#24065=ORIENTED_EDGE('',*,*,#17964,.F.);
#24066=ORIENTED_EDGE('',*,*,#17965,.T.);
#24067=ORIENTED_EDGE('',*,*,#17966,.T.);
#24068=ORIENTED_EDGE('',*,*,#17967,.T.);
#24069=ORIENTED_EDGE('',*,*,#17968,.T.);
#24070=ORIENTED_EDGE('',*,*,#17969,.F.);
#24071=ORIENTED_EDGE('',*,*,#17970,.F.);
#24072=ORIENTED_EDGE('',*,*,#17921,.F.);
#24073=ORIENTED_EDGE('',*,*,#17936,.F.);
#24074=ORIENTED_EDGE('',*,*,#17933,.F.);
#24075=ORIENTED_EDGE('',*,*,#17922,.F.);
#24076=ORIENTED_EDGE('',*,*,#17934,.F.);
#24077=ORIENTED_EDGE('',*,*,#17941,.F.);
#24078=ORIENTED_EDGE('',*,*,#17938,.F.);
#24079=ORIENTED_EDGE('',*,*,#17935,.F.);
#24080=ORIENTED_EDGE('',*,*,#17939,.F.);
#24081=ORIENTED_EDGE('',*,*,#17946,.F.);
#24082=ORIENTED_EDGE('',*,*,#17943,.F.);
#24083=ORIENTED_EDGE('',*,*,#17940,.F.);
#24084=ORIENTED_EDGE('',*,*,#17944,.F.);
#24085=ORIENTED_EDGE('',*,*,#17949,.F.);
#24086=ORIENTED_EDGE('',*,*,#17948,.F.);
#24087=ORIENTED_EDGE('',*,*,#17945,.F.);
#24088=ORIENTED_EDGE('',*,*,#17971,.T.);
#24089=ORIENTED_EDGE('',*,*,#17972,.T.);
#24090=ORIENTED_EDGE('',*,*,#17963,.T.);
#24091=ORIENTED_EDGE('',*,*,#17972,.F.);
#24092=ORIENTED_EDGE('',*,*,#17971,.F.);
#24093=ORIENTED_EDGE('',*,*,#17973,.T.);
#24094=ORIENTED_EDGE('',*,*,#17974,.F.);
#24095=ORIENTED_EDGE('',*,*,#17975,.F.);
#24096=ORIENTED_EDGE('',*,*,#17973,.F.);
#24097=ORIENTED_EDGE('',*,*,#17976,.T.);
#24098=ORIENTED_EDGE('',*,*,#17977,.T.);
#24099=ORIENTED_EDGE('',*,*,#17970,.T.);
#24100=ORIENTED_EDGE('',*,*,#17977,.F.);
#24101=ORIENTED_EDGE('',*,*,#17976,.F.);
#24102=ORIENTED_EDGE('',*,*,#17978,.T.);
#24103=ORIENTED_EDGE('',*,*,#17979,.F.);
#24104=ORIENTED_EDGE('',*,*,#17980,.F.);
#24105=ORIENTED_EDGE('',*,*,#17978,.F.);
#24106=ORIENTED_EDGE('',*,*,#17981,.T.);
#24107=ORIENTED_EDGE('',*,*,#17982,.T.);
#24108=ORIENTED_EDGE('',*,*,#17964,.T.);
#24109=ORIENTED_EDGE('',*,*,#17982,.F.);
#24110=ORIENTED_EDGE('',*,*,#17981,.F.);
#24111=ORIENTED_EDGE('',*,*,#17983,.T.);
#24112=ORIENTED_EDGE('',*,*,#17984,.F.);
#24113=ORIENTED_EDGE('',*,*,#17985,.F.);
#24114=ORIENTED_EDGE('',*,*,#17983,.F.);
#24115=ORIENTED_EDGE('',*,*,#17986,.T.);
#24116=ORIENTED_EDGE('',*,*,#17987,.T.);
#24117=ORIENTED_EDGE('',*,*,#17969,.T.);
#24118=ORIENTED_EDGE('',*,*,#17987,.F.);
#24119=ORIENTED_EDGE('',*,*,#17986,.F.);
#24120=ORIENTED_EDGE('',*,*,#17988,.T.);
#24121=ORIENTED_EDGE('',*,*,#17989,.F.);
#24122=ORIENTED_EDGE('',*,*,#17990,.F.);
#24123=ORIENTED_EDGE('',*,*,#17988,.F.);
#24124=ORIENTED_EDGE('',*,*,#17974,.T.);
#24125=ORIENTED_EDGE('',*,*,#17975,.T.);
#24126=ORIENTED_EDGE('',*,*,#17991,.T.);
#24127=ORIENTED_EDGE('',*,*,#17843,.T.);
#24128=ORIENTED_EDGE('',*,*,#17991,.F.);
#24129=ORIENTED_EDGE('',*,*,#17979,.T.);
#24130=ORIENTED_EDGE('',*,*,#17980,.T.);
#24131=ORIENTED_EDGE('',*,*,#17992,.T.);
#24132=ORIENTED_EDGE('',*,*,#17836,.T.);
#24133=ORIENTED_EDGE('',*,*,#17992,.F.);
#24134=ORIENTED_EDGE('',*,*,#17984,.T.);
#24135=ORIENTED_EDGE('',*,*,#17985,.T.);
#24136=ORIENTED_EDGE('',*,*,#17993,.T.);
#24137=ORIENTED_EDGE('',*,*,#17842,.T.);
#24138=ORIENTED_EDGE('',*,*,#17993,.F.);
#24139=ORIENTED_EDGE('',*,*,#17989,.T.);
#24140=ORIENTED_EDGE('',*,*,#17990,.T.);
#24141=ORIENTED_EDGE('',*,*,#17994,.T.);
#24142=ORIENTED_EDGE('',*,*,#17837,.T.);
#24143=ORIENTED_EDGE('',*,*,#17994,.F.);
#24144=ORIENTED_EDGE('',*,*,#17957,.T.);
#24145=ORIENTED_EDGE('',*,*,#17959,.F.);
#24146=ORIENTED_EDGE('',*,*,#17880,.F.);
#24147=ORIENTED_EDGE('',*,*,#17826,.F.);
#24148=ORIENTED_EDGE('',*,*,#17995,.T.);
#24149=ORIENTED_EDGE('',*,*,#17958,.T.);
#24150=ORIENTED_EDGE('',*,*,#17995,.F.);
#24151=ORIENTED_EDGE('',*,*,#17825,.F.);
#24152=ORIENTED_EDGE('',*,*,#17821,.F.);
#24153=ORIENTED_EDGE('',*,*,#17955,.T.);
#24154=ORIENTED_EDGE('',*,*,#17961,.F.);
#24155=ORIENTED_EDGE('',*,*,#17996,.F.);
#24156=ORIENTED_EDGE('',*,*,#17997,.F.);
#24157=ORIENTED_EDGE('',*,*,#17998,.F.);
#24158=ORIENTED_EDGE('',*,*,#17998,.T.);
#24159=ORIENTED_EDGE('',*,*,#17999,.F.);
#24160=ORIENTED_EDGE('',*,*,#17828,.F.);
#24161=ORIENTED_EDGE('',*,*,#17879,.F.);
#24162=ORIENTED_EDGE('',*,*,#17962,.T.);
#24163=ORIENTED_EDGE('',*,*,#17865,.T.);
#24164=ORIENTED_EDGE('',*,*,#18000,.T.);
#24165=ORIENTED_EDGE('',*,*,#17996,.T.);
#24166=ORIENTED_EDGE('',*,*,#17960,.F.);
#24167=ORIENTED_EDGE('',*,*,#17950,.F.);
#24168=ORIENTED_EDGE('',*,*,#17875,.T.);
#24169=ORIENTED_EDGE('',*,*,#17861,.T.);
#24170=ORIENTED_EDGE('',*,*,#17829,.F.);
#24171=ORIENTED_EDGE('',*,*,#17999,.T.);
#24172=ORIENTED_EDGE('',*,*,#17997,.T.);
#24173=ORIENTED_EDGE('',*,*,#18000,.F.);
#24174=ORIENTED_EDGE('',*,*,#18001,.T.);
#24175=ORIENTED_EDGE('',*,*,#17952,.F.);
#24176=ORIENTED_EDGE('',*,*,#17823,.F.);
#24177=ORIENTED_EDGE('',*,*,#17835,.F.);
#24178=ORIENTED_EDGE('',*,*,#18002,.T.);
#24179=ORIENTED_EDGE('',*,*,#18003,.T.);
#24180=ORIENTED_EDGE('',*,*,#18002,.F.);
#24181=ORIENTED_EDGE('',*,*,#17834,.F.);
#24182=ORIENTED_EDGE('',*,*,#17846,.F.);
#24183=ORIENTED_EDGE('',*,*,#17847,.T.);
#24184=ORIENTED_EDGE('',*,*,#17927,.F.);
#24185=ORIENTED_EDGE('',*,*,#17953,.F.);
#24186=ORIENTED_EDGE('',*,*,#18001,.F.);
#24187=ORIENTED_EDGE('',*,*,#18003,.F.);
#24188=ORIENTED_EDGE('',*,*,#17859,.F.);
#24189=ORIENTED_EDGE('',*,*,#17849,.F.);
#24190=ORIENTED_EDGE('',*,*,#18004,.F.);
#24191=ORIENTED_EDGE('',*,*,#17870,.F.);
#24192=ORIENTED_EDGE('',*,*,#17874,.F.);
#24193=ORIENTED_EDGE('',*,*,#18004,.T.);
#24194=ORIENTED_EDGE('',*,*,#17848,.F.);
#24195=ORIENTED_EDGE('',*,*,#17844,.F.);
#24196=ORIENTED_EDGE('',*,*,#17832,.F.);
#24197=ORIENTED_EDGE('',*,*,#17871,.T.);
#24198=ORIENTED_EDGE('',*,*,#17840,.F.);
#24199=ORIENTED_EDGE('',*,*,#18005,.T.);
#24200=ORIENTED_EDGE('',*,*,#17967,.F.);
#24201=ORIENTED_EDGE('',*,*,#18006,.T.);
#24202=ORIENTED_EDGE('',*,*,#17841,.F.);
#24203=ORIENTED_EDGE('',*,*,#18006,.F.);
#24204=ORIENTED_EDGE('',*,*,#17966,.F.);
#24205=ORIENTED_EDGE('',*,*,#18007,.F.);
#24206=ORIENTED_EDGE('',*,*,#17838,.F.);
#24207=ORIENTED_EDGE('',*,*,#18007,.T.);
#24208=ORIENTED_EDGE('',*,*,#17965,.F.);
#24209=ORIENTED_EDGE('',*,*,#18008,.F.);
#24210=ORIENTED_EDGE('',*,*,#17839,.F.);
#24211=ORIENTED_EDGE('',*,*,#18008,.T.);
#24212=ORIENTED_EDGE('',*,*,#17968,.F.);
#24213=ORIENTED_EDGE('',*,*,#18005,.F.);
#24214=ORIENTED_EDGE('',*,*,#18009,.T.);
#24215=ORIENTED_EDGE('',*,*,#18010,.F.);
#24216=ORIENTED_EDGE('',*,*,#18011,.F.);
#24217=ORIENTED_EDGE('',*,*,#18012,.T.);
#24218=ORIENTED_EDGE('',*,*,#18013,.T.);
#24219=ORIENTED_EDGE('',*,*,#18014,.F.);
#24220=ORIENTED_EDGE('',*,*,#18015,.F.);
#24221=ORIENTED_EDGE('',*,*,#18010,.T.);
#24222=ORIENTED_EDGE('',*,*,#18016,.T.);
#24223=ORIENTED_EDGE('',*,*,#18017,.F.);
#24224=ORIENTED_EDGE('',*,*,#18018,.F.);
#24225=ORIENTED_EDGE('',*,*,#18014,.T.);
#24226=ORIENTED_EDGE('',*,*,#18019,.T.);
#24227=ORIENTED_EDGE('',*,*,#18020,.F.);
#24228=ORIENTED_EDGE('',*,*,#18021,.F.);
#24229=ORIENTED_EDGE('',*,*,#18017,.T.);
#24230=ORIENTED_EDGE('',*,*,#18022,.T.);
#24231=ORIENTED_EDGE('',*,*,#18023,.F.);
#24232=ORIENTED_EDGE('',*,*,#18024,.F.);
#24233=ORIENTED_EDGE('',*,*,#18025,.T.);
#24234=ORIENTED_EDGE('',*,*,#18026,.T.);
#24235=ORIENTED_EDGE('',*,*,#18027,.F.);
#24236=ORIENTED_EDGE('',*,*,#18028,.F.);
#24237=ORIENTED_EDGE('',*,*,#18023,.T.);
#24238=ORIENTED_EDGE('',*,*,#18029,.T.);
#24239=ORIENTED_EDGE('',*,*,#18030,.F.);
#24240=ORIENTED_EDGE('',*,*,#18031,.F.);
#24241=ORIENTED_EDGE('',*,*,#18027,.T.);
#24242=ORIENTED_EDGE('',*,*,#18032,.T.);
#24243=ORIENTED_EDGE('',*,*,#18033,.F.);
#24244=ORIENTED_EDGE('',*,*,#18034,.F.);
#24245=ORIENTED_EDGE('',*,*,#18030,.T.);
#24246=ORIENTED_EDGE('',*,*,#18035,.T.);
#24247=ORIENTED_EDGE('',*,*,#18036,.F.);
#24248=ORIENTED_EDGE('',*,*,#18037,.F.);
#24249=ORIENTED_EDGE('',*,*,#18020,.T.);
#24250=ORIENTED_EDGE('',*,*,#18038,.T.);
#24251=ORIENTED_EDGE('',*,*,#18012,.F.);
#24252=ORIENTED_EDGE('',*,*,#18039,.F.);
#24253=ORIENTED_EDGE('',*,*,#18040,.T.);
#24254=ORIENTED_EDGE('',*,*,#18041,.T.);
#24255=ORIENTED_EDGE('',*,*,#18040,.F.);
#24256=ORIENTED_EDGE('',*,*,#18042,.F.);
#24257=ORIENTED_EDGE('',*,*,#18043,.T.);
#24258=ORIENTED_EDGE('',*,*,#18044,.T.);
#24259=ORIENTED_EDGE('',*,*,#18043,.F.);
#24260=ORIENTED_EDGE('',*,*,#18045,.F.);
#24261=ORIENTED_EDGE('',*,*,#18036,.T.);
#24262=ORIENTED_EDGE('',*,*,#18046,.T.);
#24263=ORIENTED_EDGE('',*,*,#18047,.F.);
#24264=ORIENTED_EDGE('',*,*,#18048,.F.);
#24265=ORIENTED_EDGE('',*,*,#18033,.T.);
#24266=ORIENTED_EDGE('',*,*,#18049,.T.);
#24267=ORIENTED_EDGE('',*,*,#18050,.F.);
#24268=ORIENTED_EDGE('',*,*,#18051,.F.);
#24269=ORIENTED_EDGE('',*,*,#18047,.T.);
#24270=ORIENTED_EDGE('',*,*,#18052,.T.);
#24271=ORIENTED_EDGE('',*,*,#18053,.F.);
#24272=ORIENTED_EDGE('',*,*,#18054,.F.);
#24273=ORIENTED_EDGE('',*,*,#18050,.T.);
#24274=ORIENTED_EDGE('',*,*,#18055,.T.);
#24275=ORIENTED_EDGE('',*,*,#18025,.F.);
#24276=ORIENTED_EDGE('',*,*,#18056,.F.);
#24277=ORIENTED_EDGE('',*,*,#18053,.T.);
#24278=ORIENTED_EDGE('',*,*,#18048,.T.);
#24279=ORIENTED_EDGE('',*,*,#18051,.T.);
#24280=ORIENTED_EDGE('',*,*,#18054,.T.);
#24281=ORIENTED_EDGE('',*,*,#18056,.T.);
#24282=ORIENTED_EDGE('',*,*,#18024,.T.);
#24283=ORIENTED_EDGE('',*,*,#18028,.T.);
#24284=ORIENTED_EDGE('',*,*,#18031,.T.);
#24285=ORIENTED_EDGE('',*,*,#18034,.T.);
#24286=ORIENTED_EDGE('',*,*,#18037,.T.);
#24287=ORIENTED_EDGE('',*,*,#18045,.T.);
#24288=ORIENTED_EDGE('',*,*,#18042,.T.);
#24289=ORIENTED_EDGE('',*,*,#18039,.T.);
#24290=ORIENTED_EDGE('',*,*,#18011,.T.);
#24291=ORIENTED_EDGE('',*,*,#18015,.T.);
#24292=ORIENTED_EDGE('',*,*,#18018,.T.);
#24293=ORIENTED_EDGE('',*,*,#18021,.T.);
#24294=ORIENTED_EDGE('',*,*,#18046,.F.);
#24295=ORIENTED_EDGE('',*,*,#18032,.F.);
#24296=ORIENTED_EDGE('',*,*,#18029,.F.);
#24297=ORIENTED_EDGE('',*,*,#18026,.F.);
#24298=ORIENTED_EDGE('',*,*,#18022,.F.);
#24299=ORIENTED_EDGE('',*,*,#18055,.F.);
#24300=ORIENTED_EDGE('',*,*,#18052,.F.);
#24301=ORIENTED_EDGE('',*,*,#18049,.F.);
#24302=ORIENTED_EDGE('',*,*,#18035,.F.);
#24303=ORIENTED_EDGE('',*,*,#18019,.F.);
#24304=ORIENTED_EDGE('',*,*,#18016,.F.);
#24305=ORIENTED_EDGE('',*,*,#18013,.F.);
#24306=ORIENTED_EDGE('',*,*,#18009,.F.);
#24307=ORIENTED_EDGE('',*,*,#18038,.F.);
#24308=ORIENTED_EDGE('',*,*,#18041,.F.);
#24309=ORIENTED_EDGE('',*,*,#18044,.F.);
#24310=ORIENTED_EDGE('',*,*,#18057,.T.);
#24311=ORIENTED_EDGE('',*,*,#18058,.F.);
#24312=ORIENTED_EDGE('',*,*,#18059,.F.);
#24313=ORIENTED_EDGE('',*,*,#18060,.T.);
#24314=ORIENTED_EDGE('',*,*,#18061,.T.);
#24315=ORIENTED_EDGE('',*,*,#18062,.F.);
#24316=ORIENTED_EDGE('',*,*,#18063,.F.);
#24317=ORIENTED_EDGE('',*,*,#18058,.T.);
#24318=ORIENTED_EDGE('',*,*,#18064,.T.);
#24319=ORIENTED_EDGE('',*,*,#18065,.F.);
#24320=ORIENTED_EDGE('',*,*,#18066,.F.);
#24321=ORIENTED_EDGE('',*,*,#18062,.T.);
#24322=ORIENTED_EDGE('',*,*,#18067,.T.);
#24323=ORIENTED_EDGE('',*,*,#18068,.F.);
#24324=ORIENTED_EDGE('',*,*,#18069,.F.);
#24325=ORIENTED_EDGE('',*,*,#18065,.T.);
#24326=ORIENTED_EDGE('',*,*,#18070,.T.);
#24327=ORIENTED_EDGE('',*,*,#18071,.F.);
#24328=ORIENTED_EDGE('',*,*,#18072,.F.);
#24329=ORIENTED_EDGE('',*,*,#18073,.T.);
#24330=ORIENTED_EDGE('',*,*,#18074,.T.);
#24331=ORIENTED_EDGE('',*,*,#18075,.F.);
#24332=ORIENTED_EDGE('',*,*,#18076,.F.);
#24333=ORIENTED_EDGE('',*,*,#18071,.T.);
#24334=ORIENTED_EDGE('',*,*,#18077,.T.);
#24335=ORIENTED_EDGE('',*,*,#18078,.F.);
#24336=ORIENTED_EDGE('',*,*,#18079,.F.);
#24337=ORIENTED_EDGE('',*,*,#18075,.T.);
#24338=ORIENTED_EDGE('',*,*,#18080,.T.);
#24339=ORIENTED_EDGE('',*,*,#18081,.F.);
#24340=ORIENTED_EDGE('',*,*,#18082,.F.);
#24341=ORIENTED_EDGE('',*,*,#18078,.T.);
#24342=ORIENTED_EDGE('',*,*,#18083,.T.);
#24343=ORIENTED_EDGE('',*,*,#18084,.F.);
#24344=ORIENTED_EDGE('',*,*,#18085,.F.);
#24345=ORIENTED_EDGE('',*,*,#18068,.T.);
#24346=ORIENTED_EDGE('',*,*,#18086,.T.);
#24347=ORIENTED_EDGE('',*,*,#18060,.F.);
#24348=ORIENTED_EDGE('',*,*,#18087,.F.);
#24349=ORIENTED_EDGE('',*,*,#18088,.T.);
#24350=ORIENTED_EDGE('',*,*,#18089,.T.);
#24351=ORIENTED_EDGE('',*,*,#18088,.F.);
#24352=ORIENTED_EDGE('',*,*,#18090,.F.);
#24353=ORIENTED_EDGE('',*,*,#18091,.T.);
#24354=ORIENTED_EDGE('',*,*,#18092,.T.);
#24355=ORIENTED_EDGE('',*,*,#18091,.F.);
#24356=ORIENTED_EDGE('',*,*,#18093,.F.);
#24357=ORIENTED_EDGE('',*,*,#18084,.T.);
#24358=ORIENTED_EDGE('',*,*,#18094,.T.);
#24359=ORIENTED_EDGE('',*,*,#18095,.F.);
#24360=ORIENTED_EDGE('',*,*,#18096,.F.);
#24361=ORIENTED_EDGE('',*,*,#18081,.T.);
#24362=ORIENTED_EDGE('',*,*,#18097,.T.);
#24363=ORIENTED_EDGE('',*,*,#18098,.F.);
#24364=ORIENTED_EDGE('',*,*,#18099,.F.);
#24365=ORIENTED_EDGE('',*,*,#18095,.T.);
#24366=ORIENTED_EDGE('',*,*,#18100,.T.);
#24367=ORIENTED_EDGE('',*,*,#18101,.F.);
#24368=ORIENTED_EDGE('',*,*,#18102,.F.);
#24369=ORIENTED_EDGE('',*,*,#18098,.T.);
#24370=ORIENTED_EDGE('',*,*,#18103,.T.);
#24371=ORIENTED_EDGE('',*,*,#18073,.F.);
#24372=ORIENTED_EDGE('',*,*,#18104,.F.);
#24373=ORIENTED_EDGE('',*,*,#18101,.T.);
#24374=ORIENTED_EDGE('',*,*,#18096,.T.);
#24375=ORIENTED_EDGE('',*,*,#18099,.T.);
#24376=ORIENTED_EDGE('',*,*,#18102,.T.);
#24377=ORIENTED_EDGE('',*,*,#18104,.T.);
#24378=ORIENTED_EDGE('',*,*,#18072,.T.);
#24379=ORIENTED_EDGE('',*,*,#18076,.T.);
#24380=ORIENTED_EDGE('',*,*,#18079,.T.);
#24381=ORIENTED_EDGE('',*,*,#18082,.T.);
#24382=ORIENTED_EDGE('',*,*,#18085,.T.);
#24383=ORIENTED_EDGE('',*,*,#18093,.T.);
#24384=ORIENTED_EDGE('',*,*,#18090,.T.);
#24385=ORIENTED_EDGE('',*,*,#18087,.T.);
#24386=ORIENTED_EDGE('',*,*,#18059,.T.);
#24387=ORIENTED_EDGE('',*,*,#18063,.T.);
#24388=ORIENTED_EDGE('',*,*,#18066,.T.);
#24389=ORIENTED_EDGE('',*,*,#18069,.T.);
#24390=ORIENTED_EDGE('',*,*,#18094,.F.);
#24391=ORIENTED_EDGE('',*,*,#18080,.F.);
#24392=ORIENTED_EDGE('',*,*,#18077,.F.);
#24393=ORIENTED_EDGE('',*,*,#18074,.F.);
#24394=ORIENTED_EDGE('',*,*,#18070,.F.);
#24395=ORIENTED_EDGE('',*,*,#18103,.F.);
#24396=ORIENTED_EDGE('',*,*,#18100,.F.);
#24397=ORIENTED_EDGE('',*,*,#18097,.F.);
#24398=ORIENTED_EDGE('',*,*,#18083,.F.);
#24399=ORIENTED_EDGE('',*,*,#18067,.F.);
#24400=ORIENTED_EDGE('',*,*,#18064,.F.);
#24401=ORIENTED_EDGE('',*,*,#18061,.F.);
#24402=ORIENTED_EDGE('',*,*,#18057,.F.);
#24403=ORIENTED_EDGE('',*,*,#18086,.F.);
#24404=ORIENTED_EDGE('',*,*,#18089,.F.);
#24405=ORIENTED_EDGE('',*,*,#18092,.F.);
#24406=ORIENTED_EDGE('',*,*,#18105,.T.);
#24407=ORIENTED_EDGE('',*,*,#18106,.F.);
#24408=ORIENTED_EDGE('',*,*,#18107,.F.);
#24409=ORIENTED_EDGE('',*,*,#18108,.T.);
#24410=ORIENTED_EDGE('',*,*,#18109,.T.);
#24411=ORIENTED_EDGE('',*,*,#18110,.F.);
#24412=ORIENTED_EDGE('',*,*,#18111,.F.);
#24413=ORIENTED_EDGE('',*,*,#18106,.T.);
#24414=ORIENTED_EDGE('',*,*,#18112,.T.);
#24415=ORIENTED_EDGE('',*,*,#18113,.F.);
#24416=ORIENTED_EDGE('',*,*,#18114,.F.);
#24417=ORIENTED_EDGE('',*,*,#18110,.T.);
#24418=ORIENTED_EDGE('',*,*,#18115,.T.);
#24419=ORIENTED_EDGE('',*,*,#18116,.F.);
#24420=ORIENTED_EDGE('',*,*,#18117,.F.);
#24421=ORIENTED_EDGE('',*,*,#18113,.T.);
#24422=ORIENTED_EDGE('',*,*,#18118,.T.);
#24423=ORIENTED_EDGE('',*,*,#18119,.F.);
#24424=ORIENTED_EDGE('',*,*,#18120,.F.);
#24425=ORIENTED_EDGE('',*,*,#18121,.T.);
#24426=ORIENTED_EDGE('',*,*,#18122,.T.);
#24427=ORIENTED_EDGE('',*,*,#18123,.F.);
#24428=ORIENTED_EDGE('',*,*,#18124,.F.);
#24429=ORIENTED_EDGE('',*,*,#18119,.T.);
#24430=ORIENTED_EDGE('',*,*,#18125,.T.);
#24431=ORIENTED_EDGE('',*,*,#18126,.F.);
#24432=ORIENTED_EDGE('',*,*,#18127,.F.);
#24433=ORIENTED_EDGE('',*,*,#18123,.T.);
#24434=ORIENTED_EDGE('',*,*,#18128,.T.);
#24435=ORIENTED_EDGE('',*,*,#18129,.F.);
#24436=ORIENTED_EDGE('',*,*,#18130,.F.);
#24437=ORIENTED_EDGE('',*,*,#18126,.T.);
#24438=ORIENTED_EDGE('',*,*,#18131,.T.);
#24439=ORIENTED_EDGE('',*,*,#18132,.F.);
#24440=ORIENTED_EDGE('',*,*,#18133,.F.);
#24441=ORIENTED_EDGE('',*,*,#18116,.T.);
#24442=ORIENTED_EDGE('',*,*,#18134,.T.);
#24443=ORIENTED_EDGE('',*,*,#18108,.F.);
#24444=ORIENTED_EDGE('',*,*,#18135,.F.);
#24445=ORIENTED_EDGE('',*,*,#18136,.T.);
#24446=ORIENTED_EDGE('',*,*,#18137,.T.);
#24447=ORIENTED_EDGE('',*,*,#18136,.F.);
#24448=ORIENTED_EDGE('',*,*,#18138,.F.);
#24449=ORIENTED_EDGE('',*,*,#18139,.T.);
#24450=ORIENTED_EDGE('',*,*,#18140,.T.);
#24451=ORIENTED_EDGE('',*,*,#18139,.F.);
#24452=ORIENTED_EDGE('',*,*,#18141,.F.);
#24453=ORIENTED_EDGE('',*,*,#18132,.T.);
#24454=ORIENTED_EDGE('',*,*,#18142,.T.);
#24455=ORIENTED_EDGE('',*,*,#18143,.F.);
#24456=ORIENTED_EDGE('',*,*,#18144,.F.);
#24457=ORIENTED_EDGE('',*,*,#18129,.T.);
#24458=ORIENTED_EDGE('',*,*,#18145,.T.);
#24459=ORIENTED_EDGE('',*,*,#18146,.F.);
#24460=ORIENTED_EDGE('',*,*,#18147,.F.);
#24461=ORIENTED_EDGE('',*,*,#18143,.T.);
#24462=ORIENTED_EDGE('',*,*,#18148,.T.);
#24463=ORIENTED_EDGE('',*,*,#18149,.F.);
#24464=ORIENTED_EDGE('',*,*,#18150,.F.);
#24465=ORIENTED_EDGE('',*,*,#18146,.T.);
#24466=ORIENTED_EDGE('',*,*,#18151,.T.);
#24467=ORIENTED_EDGE('',*,*,#18121,.F.);
#24468=ORIENTED_EDGE('',*,*,#18152,.F.);
#24469=ORIENTED_EDGE('',*,*,#18149,.T.);
#24470=ORIENTED_EDGE('',*,*,#18144,.T.);
#24471=ORIENTED_EDGE('',*,*,#18147,.T.);
#24472=ORIENTED_EDGE('',*,*,#18150,.T.);
#24473=ORIENTED_EDGE('',*,*,#18152,.T.);
#24474=ORIENTED_EDGE('',*,*,#18120,.T.);
#24475=ORIENTED_EDGE('',*,*,#18124,.T.);
#24476=ORIENTED_EDGE('',*,*,#18127,.T.);
#24477=ORIENTED_EDGE('',*,*,#18130,.T.);
#24478=ORIENTED_EDGE('',*,*,#18133,.T.);
#24479=ORIENTED_EDGE('',*,*,#18141,.T.);
#24480=ORIENTED_EDGE('',*,*,#18138,.T.);
#24481=ORIENTED_EDGE('',*,*,#18135,.T.);
#24482=ORIENTED_EDGE('',*,*,#18107,.T.);
#24483=ORIENTED_EDGE('',*,*,#18111,.T.);
#24484=ORIENTED_EDGE('',*,*,#18114,.T.);
#24485=ORIENTED_EDGE('',*,*,#18117,.T.);
#24486=ORIENTED_EDGE('',*,*,#18142,.F.);
#24487=ORIENTED_EDGE('',*,*,#18128,.F.);
#24488=ORIENTED_EDGE('',*,*,#18125,.F.);
#24489=ORIENTED_EDGE('',*,*,#18122,.F.);
#24490=ORIENTED_EDGE('',*,*,#18118,.F.);
#24491=ORIENTED_EDGE('',*,*,#18151,.F.);
#24492=ORIENTED_EDGE('',*,*,#18148,.F.);
#24493=ORIENTED_EDGE('',*,*,#18145,.F.);
#24494=ORIENTED_EDGE('',*,*,#18131,.F.);
#24495=ORIENTED_EDGE('',*,*,#18115,.F.);
#24496=ORIENTED_EDGE('',*,*,#18112,.F.);
#24497=ORIENTED_EDGE('',*,*,#18109,.F.);
#24498=ORIENTED_EDGE('',*,*,#18105,.F.);
#24499=ORIENTED_EDGE('',*,*,#18134,.F.);
#24500=ORIENTED_EDGE('',*,*,#18137,.F.);
#24501=ORIENTED_EDGE('',*,*,#18140,.F.);
#24502=ORIENTED_EDGE('',*,*,#18153,.T.);
#24503=ORIENTED_EDGE('',*,*,#18154,.F.);
#24504=ORIENTED_EDGE('',*,*,#18155,.F.);
#24505=ORIENTED_EDGE('',*,*,#18156,.T.);
#24506=ORIENTED_EDGE('',*,*,#18157,.T.);
#24507=ORIENTED_EDGE('',*,*,#18158,.F.);
#24508=ORIENTED_EDGE('',*,*,#18159,.F.);
#24509=ORIENTED_EDGE('',*,*,#18154,.T.);
#24510=ORIENTED_EDGE('',*,*,#18160,.T.);
#24511=ORIENTED_EDGE('',*,*,#18161,.F.);
#24512=ORIENTED_EDGE('',*,*,#18162,.F.);
#24513=ORIENTED_EDGE('',*,*,#18158,.T.);
#24514=ORIENTED_EDGE('',*,*,#18163,.T.);
#24515=ORIENTED_EDGE('',*,*,#18164,.F.);
#24516=ORIENTED_EDGE('',*,*,#18165,.F.);
#24517=ORIENTED_EDGE('',*,*,#18161,.T.);
#24518=ORIENTED_EDGE('',*,*,#18166,.T.);
#24519=ORIENTED_EDGE('',*,*,#18167,.F.);
#24520=ORIENTED_EDGE('',*,*,#18168,.F.);
#24521=ORIENTED_EDGE('',*,*,#18169,.T.);
#24522=ORIENTED_EDGE('',*,*,#18170,.T.);
#24523=ORIENTED_EDGE('',*,*,#18171,.F.);
#24524=ORIENTED_EDGE('',*,*,#18172,.F.);
#24525=ORIENTED_EDGE('',*,*,#18167,.T.);
#24526=ORIENTED_EDGE('',*,*,#18173,.T.);
#24527=ORIENTED_EDGE('',*,*,#18174,.F.);
#24528=ORIENTED_EDGE('',*,*,#18175,.F.);
#24529=ORIENTED_EDGE('',*,*,#18171,.T.);
#24530=ORIENTED_EDGE('',*,*,#18176,.T.);
#24531=ORIENTED_EDGE('',*,*,#18177,.F.);
#24532=ORIENTED_EDGE('',*,*,#18178,.F.);
#24533=ORIENTED_EDGE('',*,*,#18174,.T.);
#24534=ORIENTED_EDGE('',*,*,#18179,.T.);
#24535=ORIENTED_EDGE('',*,*,#18180,.F.);
#24536=ORIENTED_EDGE('',*,*,#18181,.F.);
#24537=ORIENTED_EDGE('',*,*,#18164,.T.);
#24538=ORIENTED_EDGE('',*,*,#18182,.T.);
#24539=ORIENTED_EDGE('',*,*,#18156,.F.);
#24540=ORIENTED_EDGE('',*,*,#18183,.F.);
#24541=ORIENTED_EDGE('',*,*,#18184,.T.);
#24542=ORIENTED_EDGE('',*,*,#18185,.T.);
#24543=ORIENTED_EDGE('',*,*,#18184,.F.);
#24544=ORIENTED_EDGE('',*,*,#18186,.F.);
#24545=ORIENTED_EDGE('',*,*,#18187,.T.);
#24546=ORIENTED_EDGE('',*,*,#18188,.T.);
#24547=ORIENTED_EDGE('',*,*,#18187,.F.);
#24548=ORIENTED_EDGE('',*,*,#18189,.F.);
#24549=ORIENTED_EDGE('',*,*,#18180,.T.);
#24550=ORIENTED_EDGE('',*,*,#18190,.T.);
#24551=ORIENTED_EDGE('',*,*,#18191,.F.);
#24552=ORIENTED_EDGE('',*,*,#18192,.F.);
#24553=ORIENTED_EDGE('',*,*,#18177,.T.);
#24554=ORIENTED_EDGE('',*,*,#18193,.T.);
#24555=ORIENTED_EDGE('',*,*,#18194,.F.);
#24556=ORIENTED_EDGE('',*,*,#18195,.F.);
#24557=ORIENTED_EDGE('',*,*,#18191,.T.);
#24558=ORIENTED_EDGE('',*,*,#18196,.T.);
#24559=ORIENTED_EDGE('',*,*,#18197,.F.);
#24560=ORIENTED_EDGE('',*,*,#18198,.F.);
#24561=ORIENTED_EDGE('',*,*,#18194,.T.);
#24562=ORIENTED_EDGE('',*,*,#18199,.T.);
#24563=ORIENTED_EDGE('',*,*,#18169,.F.);
#24564=ORIENTED_EDGE('',*,*,#18200,.F.);
#24565=ORIENTED_EDGE('',*,*,#18197,.T.);
#24566=ORIENTED_EDGE('',*,*,#18192,.T.);
#24567=ORIENTED_EDGE('',*,*,#18195,.T.);
#24568=ORIENTED_EDGE('',*,*,#18198,.T.);
#24569=ORIENTED_EDGE('',*,*,#18200,.T.);
#24570=ORIENTED_EDGE('',*,*,#18168,.T.);
#24571=ORIENTED_EDGE('',*,*,#18172,.T.);
#24572=ORIENTED_EDGE('',*,*,#18175,.T.);
#24573=ORIENTED_EDGE('',*,*,#18178,.T.);
#24574=ORIENTED_EDGE('',*,*,#18181,.T.);
#24575=ORIENTED_EDGE('',*,*,#18189,.T.);
#24576=ORIENTED_EDGE('',*,*,#18186,.T.);
#24577=ORIENTED_EDGE('',*,*,#18183,.T.);
#24578=ORIENTED_EDGE('',*,*,#18155,.T.);
#24579=ORIENTED_EDGE('',*,*,#18159,.T.);
#24580=ORIENTED_EDGE('',*,*,#18162,.T.);
#24581=ORIENTED_EDGE('',*,*,#18165,.T.);
#24582=ORIENTED_EDGE('',*,*,#18190,.F.);
#24583=ORIENTED_EDGE('',*,*,#18176,.F.);
#24584=ORIENTED_EDGE('',*,*,#18173,.F.);
#24585=ORIENTED_EDGE('',*,*,#18170,.F.);
#24586=ORIENTED_EDGE('',*,*,#18166,.F.);
#24587=ORIENTED_EDGE('',*,*,#18199,.F.);
#24588=ORIENTED_EDGE('',*,*,#18196,.F.);
#24589=ORIENTED_EDGE('',*,*,#18193,.F.);
#24590=ORIENTED_EDGE('',*,*,#18179,.F.);
#24591=ORIENTED_EDGE('',*,*,#18163,.F.);
#24592=ORIENTED_EDGE('',*,*,#18160,.F.);
#24593=ORIENTED_EDGE('',*,*,#18157,.F.);
#24594=ORIENTED_EDGE('',*,*,#18153,.F.);
#24595=ORIENTED_EDGE('',*,*,#18182,.F.);
#24596=ORIENTED_EDGE('',*,*,#18185,.F.);
#24597=ORIENTED_EDGE('',*,*,#18188,.F.);
#24598=ORIENTED_EDGE('',*,*,#18201,.F.);
#24599=ORIENTED_EDGE('',*,*,#18202,.F.);
#24600=ORIENTED_EDGE('',*,*,#18203,.F.);
#24601=ORIENTED_EDGE('',*,*,#18204,.T.);
#24602=ORIENTED_EDGE('',*,*,#18205,.F.);
#24603=ORIENTED_EDGE('',*,*,#18206,.F.);
#24604=ORIENTED_EDGE('',*,*,#18207,.F.);
#24605=ORIENTED_EDGE('',*,*,#18208,.F.);
#24606=ORIENTED_EDGE('',*,*,#18209,.F.);
#24607=ORIENTED_EDGE('',*,*,#18210,.F.);
#24608=ORIENTED_EDGE('',*,*,#18211,.F.);
#24609=ORIENTED_EDGE('',*,*,#18212,.F.);
#24610=ORIENTED_EDGE('',*,*,#18213,.F.);
#24611=ORIENTED_EDGE('',*,*,#18214,.F.);
#24612=ORIENTED_EDGE('',*,*,#18215,.F.);
#24613=ORIENTED_EDGE('',*,*,#18216,.F.);
#24614=ORIENTED_EDGE('',*,*,#18213,.T.);
#24615=ORIENTED_EDGE('',*,*,#18217,.T.);
#24616=ORIENTED_EDGE('',*,*,#18218,.T.);
#24617=ORIENTED_EDGE('',*,*,#18219,.F.);
#24618=ORIENTED_EDGE('',*,*,#18212,.T.);
#24619=ORIENTED_EDGE('',*,*,#18220,.T.);
#24620=ORIENTED_EDGE('',*,*,#18221,.T.);
#24621=ORIENTED_EDGE('',*,*,#18217,.F.);
#24622=ORIENTED_EDGE('',*,*,#18211,.T.);
#24623=ORIENTED_EDGE('',*,*,#18222,.T.);
#24624=ORIENTED_EDGE('',*,*,#18223,.T.);
#24625=ORIENTED_EDGE('',*,*,#18220,.F.);
#24626=ORIENTED_EDGE('',*,*,#18210,.T.);
#24627=ORIENTED_EDGE('',*,*,#18224,.T.);
#24628=ORIENTED_EDGE('',*,*,#18225,.T.);
#24629=ORIENTED_EDGE('',*,*,#18222,.F.);
#24630=ORIENTED_EDGE('',*,*,#18205,.T.);
#24631=ORIENTED_EDGE('',*,*,#18226,.T.);
#24632=ORIENTED_EDGE('',*,*,#18227,.T.);
#24633=ORIENTED_EDGE('',*,*,#18228,.F.);
#24634=ORIENTED_EDGE('',*,*,#18203,.T.);
#24635=ORIENTED_EDGE('',*,*,#18229,.T.);
#24636=ORIENTED_EDGE('',*,*,#18230,.T.);
#24637=ORIENTED_EDGE('',*,*,#18231,.F.);
#24638=ORIENTED_EDGE('',*,*,#18202,.T.);
#24639=ORIENTED_EDGE('',*,*,#18232,.T.);
#24640=ORIENTED_EDGE('',*,*,#18233,.T.);
#24641=ORIENTED_EDGE('',*,*,#18229,.F.);
#24642=ORIENTED_EDGE('',*,*,#18234,.F.);
#24643=ORIENTED_EDGE('',*,*,#18230,.F.);
#24644=ORIENTED_EDGE('',*,*,#18233,.F.);
#24645=ORIENTED_EDGE('',*,*,#18235,.F.);
#24646=ORIENTED_EDGE('',*,*,#18236,.F.);
#24647=ORIENTED_EDGE('',*,*,#18237,.F.);
#24648=ORIENTED_EDGE('',*,*,#18238,.F.);
#24649=ORIENTED_EDGE('',*,*,#18227,.F.);
#24650=ORIENTED_EDGE('',*,*,#18218,.F.);
#24651=ORIENTED_EDGE('',*,*,#18221,.F.);
#24652=ORIENTED_EDGE('',*,*,#18223,.F.);
#24653=ORIENTED_EDGE('',*,*,#18225,.F.);
#24654=ORIENTED_EDGE('',*,*,#18239,.F.);
#24655=ORIENTED_EDGE('',*,*,#18240,.F.);
#24656=ORIENTED_EDGE('',*,*,#18241,.F.);
#24657=ORIENTED_EDGE('',*,*,#18242,.F.);
#24658=ORIENTED_EDGE('',*,*,#18209,.T.);
#24659=ORIENTED_EDGE('',*,*,#18243,.T.);
#24660=ORIENTED_EDGE('',*,*,#18239,.T.);
#24661=ORIENTED_EDGE('',*,*,#18224,.F.);
#24662=ORIENTED_EDGE('',*,*,#18201,.T.);
#24663=ORIENTED_EDGE('',*,*,#18244,.T.);
#24664=ORIENTED_EDGE('',*,*,#18235,.T.);
#24665=ORIENTED_EDGE('',*,*,#18232,.F.);
#24666=ORIENTED_EDGE('',*,*,#18214,.T.);
#24667=ORIENTED_EDGE('',*,*,#18219,.T.);
#24668=ORIENTED_EDGE('',*,*,#18242,.T.);
#24669=ORIENTED_EDGE('',*,*,#18245,.F.);
#24670=ORIENTED_EDGE('',*,*,#18215,.T.);
#24671=ORIENTED_EDGE('',*,*,#18245,.T.);
#24672=ORIENTED_EDGE('',*,*,#18241,.T.);
#24673=ORIENTED_EDGE('',*,*,#18246,.F.);
#24674=ORIENTED_EDGE('',*,*,#18216,.T.);
#24675=ORIENTED_EDGE('',*,*,#18246,.T.);
#24676=ORIENTED_EDGE('',*,*,#18240,.T.);
#24677=ORIENTED_EDGE('',*,*,#18243,.F.);
#24678=ORIENTED_EDGE('',*,*,#18234,.T.);
#24679=ORIENTED_EDGE('',*,*,#18226,.F.);
#24680=ORIENTED_EDGE('',*,*,#18204,.F.);
#24681=ORIENTED_EDGE('',*,*,#18231,.T.);
#24682=ORIENTED_EDGE('',*,*,#18206,.T.);
#24683=ORIENTED_EDGE('',*,*,#18228,.T.);
#24684=ORIENTED_EDGE('',*,*,#18238,.T.);
#24685=ORIENTED_EDGE('',*,*,#18247,.F.);
#24686=ORIENTED_EDGE('',*,*,#18207,.T.);
#24687=ORIENTED_EDGE('',*,*,#18247,.T.);
#24688=ORIENTED_EDGE('',*,*,#18237,.T.);
#24689=ORIENTED_EDGE('',*,*,#18248,.F.);
#24690=ORIENTED_EDGE('',*,*,#18208,.T.);
#24691=ORIENTED_EDGE('',*,*,#18248,.T.);
#24692=ORIENTED_EDGE('',*,*,#18236,.T.);
#24693=ORIENTED_EDGE('',*,*,#18244,.F.);
#24694=ORIENTED_EDGE('',*,*,#18249,.F.);
#24695=ORIENTED_EDGE('',*,*,#18250,.F.);
#24696=ORIENTED_EDGE('',*,*,#18251,.F.);
#24697=ORIENTED_EDGE('',*,*,#18252,.F.);
#24698=ORIENTED_EDGE('',*,*,#18253,.F.);
#24699=ORIENTED_EDGE('',*,*,#18254,.F.);
#24700=ORIENTED_EDGE('',*,*,#18255,.F.);
#24701=ORIENTED_EDGE('',*,*,#18256,.T.);
#24702=ORIENTED_EDGE('',*,*,#18257,.F.);
#24703=ORIENTED_EDGE('',*,*,#18258,.F.);
#24704=ORIENTED_EDGE('',*,*,#18259,.F.);
#24705=ORIENTED_EDGE('',*,*,#18260,.F.);
#24706=ORIENTED_EDGE('',*,*,#18261,.F.);
#24707=ORIENTED_EDGE('',*,*,#18262,.F.);
#24708=ORIENTED_EDGE('',*,*,#18263,.F.);
#24709=ORIENTED_EDGE('',*,*,#18264,.F.);
#24710=ORIENTED_EDGE('',*,*,#18261,.T.);
#24711=ORIENTED_EDGE('',*,*,#18265,.T.);
#24712=ORIENTED_EDGE('',*,*,#18266,.T.);
#24713=ORIENTED_EDGE('',*,*,#18267,.F.);
#24714=ORIENTED_EDGE('',*,*,#18260,.T.);
#24715=ORIENTED_EDGE('',*,*,#18268,.T.);
#24716=ORIENTED_EDGE('',*,*,#18269,.T.);
#24717=ORIENTED_EDGE('',*,*,#18265,.F.);
#24718=ORIENTED_EDGE('',*,*,#18259,.T.);
#24719=ORIENTED_EDGE('',*,*,#18270,.T.);
#24720=ORIENTED_EDGE('',*,*,#18271,.T.);
#24721=ORIENTED_EDGE('',*,*,#18268,.F.);
#24722=ORIENTED_EDGE('',*,*,#18258,.T.);
#24723=ORIENTED_EDGE('',*,*,#18272,.T.);
#24724=ORIENTED_EDGE('',*,*,#18273,.T.);
#24725=ORIENTED_EDGE('',*,*,#18270,.F.);
#24726=ORIENTED_EDGE('',*,*,#18253,.T.);
#24727=ORIENTED_EDGE('',*,*,#18274,.T.);
#24728=ORIENTED_EDGE('',*,*,#18275,.T.);
#24729=ORIENTED_EDGE('',*,*,#18276,.F.);
#24730=ORIENTED_EDGE('',*,*,#18252,.T.);
#24731=ORIENTED_EDGE('',*,*,#18277,.T.);
#24732=ORIENTED_EDGE('',*,*,#18278,.T.);
#24733=ORIENTED_EDGE('',*,*,#18274,.F.);
#24734=ORIENTED_EDGE('',*,*,#18251,.T.);
#24735=ORIENTED_EDGE('',*,*,#18279,.T.);
#24736=ORIENTED_EDGE('',*,*,#18280,.T.);
#24737=ORIENTED_EDGE('',*,*,#18277,.F.);
#24738=ORIENTED_EDGE('',*,*,#18250,.T.);
#24739=ORIENTED_EDGE('',*,*,#18281,.T.);
#24740=ORIENTED_EDGE('',*,*,#18282,.T.);
#24741=ORIENTED_EDGE('',*,*,#18279,.F.);
#24742=ORIENTED_EDGE('',*,*,#18278,.F.);
#24743=ORIENTED_EDGE('',*,*,#18280,.F.);
#24744=ORIENTED_EDGE('',*,*,#18282,.F.);
#24745=ORIENTED_EDGE('',*,*,#18283,.F.);
#24746=ORIENTED_EDGE('',*,*,#18284,.F.);
#24747=ORIENTED_EDGE('',*,*,#18285,.F.);
#24748=ORIENTED_EDGE('',*,*,#18286,.F.);
#24749=ORIENTED_EDGE('',*,*,#18275,.F.);
#24750=ORIENTED_EDGE('',*,*,#18266,.F.);
#24751=ORIENTED_EDGE('',*,*,#18269,.F.);
#24752=ORIENTED_EDGE('',*,*,#18271,.F.);
#24753=ORIENTED_EDGE('',*,*,#18273,.F.);
#24754=ORIENTED_EDGE('',*,*,#18287,.F.);
#24755=ORIENTED_EDGE('',*,*,#18288,.F.);
#24756=ORIENTED_EDGE('',*,*,#18289,.F.);
#24757=ORIENTED_EDGE('',*,*,#18290,.F.);
#24758=ORIENTED_EDGE('',*,*,#18257,.T.);
#24759=ORIENTED_EDGE('',*,*,#18291,.T.);
#24760=ORIENTED_EDGE('',*,*,#18287,.T.);
#24761=ORIENTED_EDGE('',*,*,#18272,.F.);
#24762=ORIENTED_EDGE('',*,*,#18249,.T.);
#24763=ORIENTED_EDGE('',*,*,#18292,.T.);
#24764=ORIENTED_EDGE('',*,*,#18283,.T.);
#24765=ORIENTED_EDGE('',*,*,#18281,.F.);
#24766=ORIENTED_EDGE('',*,*,#18262,.T.);
#24767=ORIENTED_EDGE('',*,*,#18267,.T.);
#24768=ORIENTED_EDGE('',*,*,#18290,.T.);
#24769=ORIENTED_EDGE('',*,*,#18293,.F.);
#24770=ORIENTED_EDGE('',*,*,#18263,.T.);
#24771=ORIENTED_EDGE('',*,*,#18293,.T.);
#24772=ORIENTED_EDGE('',*,*,#18289,.T.);
#24773=ORIENTED_EDGE('',*,*,#18294,.F.);
#24774=ORIENTED_EDGE('',*,*,#18264,.T.);
#24775=ORIENTED_EDGE('',*,*,#18294,.T.);
#24776=ORIENTED_EDGE('',*,*,#18288,.T.);
#24777=ORIENTED_EDGE('',*,*,#18291,.F.);
#24778=ORIENTED_EDGE('',*,*,#18254,.T.);
#24779=ORIENTED_EDGE('',*,*,#18276,.T.);
#24780=ORIENTED_EDGE('',*,*,#18286,.T.);
#24781=ORIENTED_EDGE('',*,*,#18295,.F.);
#24782=ORIENTED_EDGE('',*,*,#18255,.T.);
#24783=ORIENTED_EDGE('',*,*,#18295,.T.);
#24784=ORIENTED_EDGE('',*,*,#18285,.T.);
#24785=ORIENTED_EDGE('',*,*,#18296,.F.);
#24786=ORIENTED_EDGE('',*,*,#18284,.T.);
#24787=ORIENTED_EDGE('',*,*,#18292,.F.);
#24788=ORIENTED_EDGE('',*,*,#18256,.F.);
#24789=ORIENTED_EDGE('',*,*,#18296,.T.);
#24790=ORIENTED_EDGE('',*,*,#18297,.F.);
#24791=ORIENTED_EDGE('',*,*,#18298,.F.);
#24792=ORIENTED_EDGE('',*,*,#18299,.F.);
#24793=ORIENTED_EDGE('',*,*,#18300,.F.);
#24794=ORIENTED_EDGE('',*,*,#18301,.F.);
#24795=ORIENTED_EDGE('',*,*,#18302,.F.);
#24796=ORIENTED_EDGE('',*,*,#18303,.F.);
#24797=ORIENTED_EDGE('',*,*,#18304,.F.);
#24798=ORIENTED_EDGE('',*,*,#18305,.F.);
#24799=ORIENTED_EDGE('',*,*,#18306,.F.);
#24800=ORIENTED_EDGE('',*,*,#18307,.F.);
#24801=ORIENTED_EDGE('',*,*,#18308,.F.);
#24802=ORIENTED_EDGE('',*,*,#18309,.F.);
#24803=ORIENTED_EDGE('',*,*,#18310,.F.);
#24804=ORIENTED_EDGE('',*,*,#18311,.F.);
#24805=ORIENTED_EDGE('',*,*,#18312,.F.);
#24806=ORIENTED_EDGE('',*,*,#18309,.T.);
#24807=ORIENTED_EDGE('',*,*,#18313,.T.);
#24808=ORIENTED_EDGE('',*,*,#18314,.T.);
#24809=ORIENTED_EDGE('',*,*,#18315,.F.);
#24810=ORIENTED_EDGE('',*,*,#18308,.T.);
#24811=ORIENTED_EDGE('',*,*,#18316,.T.);
#24812=ORIENTED_EDGE('',*,*,#18317,.T.);
#24813=ORIENTED_EDGE('',*,*,#18313,.F.);
#24814=ORIENTED_EDGE('',*,*,#18307,.T.);
#24815=ORIENTED_EDGE('',*,*,#18318,.T.);
#24816=ORIENTED_EDGE('',*,*,#18319,.T.);
#24817=ORIENTED_EDGE('',*,*,#18316,.F.);
#24818=ORIENTED_EDGE('',*,*,#18306,.T.);
#24819=ORIENTED_EDGE('',*,*,#18320,.T.);
#24820=ORIENTED_EDGE('',*,*,#18321,.T.);
#24821=ORIENTED_EDGE('',*,*,#18318,.F.);
#24822=ORIENTED_EDGE('',*,*,#18301,.T.);
#24823=ORIENTED_EDGE('',*,*,#18322,.T.);
#24824=ORIENTED_EDGE('',*,*,#18323,.T.);
#24825=ORIENTED_EDGE('',*,*,#18324,.F.);
#24826=ORIENTED_EDGE('',*,*,#18300,.T.);
#24827=ORIENTED_EDGE('',*,*,#18325,.T.);
#24828=ORIENTED_EDGE('',*,*,#18326,.T.);
#24829=ORIENTED_EDGE('',*,*,#18322,.F.);
#24830=ORIENTED_EDGE('',*,*,#18299,.T.);
#24831=ORIENTED_EDGE('',*,*,#18327,.F.);
#24832=ORIENTED_EDGE('',*,*,#18328,.T.);
#24833=ORIENTED_EDGE('',*,*,#18325,.F.);
#24834=ORIENTED_EDGE('',*,*,#18298,.T.);
#24835=ORIENTED_EDGE('',*,*,#18329,.T.);
#24836=ORIENTED_EDGE('',*,*,#18330,.T.);
#24837=ORIENTED_EDGE('',*,*,#18327,.T.);
#24838=ORIENTED_EDGE('',*,*,#18323,.F.);
#24839=ORIENTED_EDGE('',*,*,#18326,.F.);
#24840=ORIENTED_EDGE('',*,*,#18328,.F.);
#24841=ORIENTED_EDGE('',*,*,#18330,.F.);
#24842=ORIENTED_EDGE('',*,*,#18331,.F.);
#24843=ORIENTED_EDGE('',*,*,#18332,.F.);
#24844=ORIENTED_EDGE('',*,*,#18333,.T.);
#24845=ORIENTED_EDGE('',*,*,#18334,.F.);
#24846=ORIENTED_EDGE('',*,*,#18314,.F.);
#24847=ORIENTED_EDGE('',*,*,#18317,.F.);
#24848=ORIENTED_EDGE('',*,*,#18319,.F.);
#24849=ORIENTED_EDGE('',*,*,#18321,.F.);
#24850=ORIENTED_EDGE('',*,*,#18335,.F.);
#24851=ORIENTED_EDGE('',*,*,#18336,.F.);
#24852=ORIENTED_EDGE('',*,*,#18337,.F.);
#24853=ORIENTED_EDGE('',*,*,#18338,.F.);
#24854=ORIENTED_EDGE('',*,*,#18305,.T.);
#24855=ORIENTED_EDGE('',*,*,#18339,.T.);
#24856=ORIENTED_EDGE('',*,*,#18335,.T.);
#24857=ORIENTED_EDGE('',*,*,#18320,.F.);
#24858=ORIENTED_EDGE('',*,*,#18297,.T.);
#24859=ORIENTED_EDGE('',*,*,#18340,.T.);
#24860=ORIENTED_EDGE('',*,*,#18331,.T.);
#24861=ORIENTED_EDGE('',*,*,#18329,.F.);
#24862=ORIENTED_EDGE('',*,*,#18310,.T.);
#24863=ORIENTED_EDGE('',*,*,#18315,.T.);
#24864=ORIENTED_EDGE('',*,*,#18338,.T.);
#24865=ORIENTED_EDGE('',*,*,#18341,.F.);
#24866=ORIENTED_EDGE('',*,*,#18311,.T.);
#24867=ORIENTED_EDGE('',*,*,#18341,.T.);
#24868=ORIENTED_EDGE('',*,*,#18337,.T.);
#24869=ORIENTED_EDGE('',*,*,#18342,.T.);
#24870=ORIENTED_EDGE('',*,*,#18312,.T.);
#24871=ORIENTED_EDGE('',*,*,#18342,.F.);
#24872=ORIENTED_EDGE('',*,*,#18336,.T.);
#24873=ORIENTED_EDGE('',*,*,#18339,.F.);
#24874=ORIENTED_EDGE('',*,*,#18304,.T.);
#24875=ORIENTED_EDGE('',*,*,#18343,.T.);
#24876=ORIENTED_EDGE('',*,*,#18332,.T.);
#24877=ORIENTED_EDGE('',*,*,#18340,.F.);
#24878=ORIENTED_EDGE('',*,*,#18303,.T.);
#24879=ORIENTED_EDGE('',*,*,#18344,.T.);
#24880=ORIENTED_EDGE('',*,*,#18333,.F.);
#24881=ORIENTED_EDGE('',*,*,#18343,.F.);
#24882=ORIENTED_EDGE('',*,*,#18302,.T.);
#24883=ORIENTED_EDGE('',*,*,#18324,.T.);
#24884=ORIENTED_EDGE('',*,*,#18334,.T.);
#24885=ORIENTED_EDGE('',*,*,#18344,.F.);
#24886=ORIENTED_EDGE('',*,*,#18345,.F.);
#24887=ORIENTED_EDGE('',*,*,#18346,.F.);
#24888=ORIENTED_EDGE('',*,*,#18347,.F.);
#24889=ORIENTED_EDGE('',*,*,#18348,.F.);
#24890=ORIENTED_EDGE('',*,*,#18349,.F.);
#24891=ORIENTED_EDGE('',*,*,#18350,.F.);
#24892=ORIENTED_EDGE('',*,*,#18351,.T.);
#24893=ORIENTED_EDGE('',*,*,#18352,.F.);
#24894=ORIENTED_EDGE('',*,*,#18353,.F.);
#24895=ORIENTED_EDGE('',*,*,#18354,.F.);
#24896=ORIENTED_EDGE('',*,*,#18355,.F.);
#24897=ORIENTED_EDGE('',*,*,#18356,.F.);
#24898=ORIENTED_EDGE('',*,*,#18357,.F.);
#24899=ORIENTED_EDGE('',*,*,#18358,.F.);
#24900=ORIENTED_EDGE('',*,*,#18359,.F.);
#24901=ORIENTED_EDGE('',*,*,#18360,.F.);
#24902=ORIENTED_EDGE('',*,*,#18357,.T.);
#24903=ORIENTED_EDGE('',*,*,#18361,.T.);
#24904=ORIENTED_EDGE('',*,*,#18362,.T.);
#24905=ORIENTED_EDGE('',*,*,#18363,.F.);
#24906=ORIENTED_EDGE('',*,*,#18356,.T.);
#24907=ORIENTED_EDGE('',*,*,#18364,.T.);
#24908=ORIENTED_EDGE('',*,*,#18365,.T.);
#24909=ORIENTED_EDGE('',*,*,#18361,.F.);
#24910=ORIENTED_EDGE('',*,*,#18355,.T.);
#24911=ORIENTED_EDGE('',*,*,#18366,.T.);
#24912=ORIENTED_EDGE('',*,*,#18367,.T.);
#24913=ORIENTED_EDGE('',*,*,#18364,.F.);
#24914=ORIENTED_EDGE('',*,*,#18354,.T.);
#24915=ORIENTED_EDGE('',*,*,#18368,.T.);
#24916=ORIENTED_EDGE('',*,*,#18369,.T.);
#24917=ORIENTED_EDGE('',*,*,#18366,.F.);
#24918=ORIENTED_EDGE('',*,*,#18349,.T.);
#24919=ORIENTED_EDGE('',*,*,#18370,.T.);
#24920=ORIENTED_EDGE('',*,*,#18371,.T.);
#24921=ORIENTED_EDGE('',*,*,#18372,.F.);
#24922=ORIENTED_EDGE('',*,*,#18348,.T.);
#24923=ORIENTED_EDGE('',*,*,#18373,.T.);
#24924=ORIENTED_EDGE('',*,*,#18374,.T.);
#24925=ORIENTED_EDGE('',*,*,#18370,.F.);
#24926=ORIENTED_EDGE('',*,*,#18347,.T.);
#24927=ORIENTED_EDGE('',*,*,#18375,.T.);
#24928=ORIENTED_EDGE('',*,*,#18376,.T.);
#24929=ORIENTED_EDGE('',*,*,#18373,.F.);
#24930=ORIENTED_EDGE('',*,*,#18346,.T.);
#24931=ORIENTED_EDGE('',*,*,#18377,.T.);
#24932=ORIENTED_EDGE('',*,*,#18378,.T.);
#24933=ORIENTED_EDGE('',*,*,#18375,.F.);
#24934=ORIENTED_EDGE('',*,*,#18371,.F.);
#24935=ORIENTED_EDGE('',*,*,#18374,.F.);
#24936=ORIENTED_EDGE('',*,*,#18376,.F.);
#24937=ORIENTED_EDGE('',*,*,#18378,.F.);
#24938=ORIENTED_EDGE('',*,*,#18379,.F.);
#24939=ORIENTED_EDGE('',*,*,#18380,.F.);
#24940=ORIENTED_EDGE('',*,*,#18381,.F.);
#24941=ORIENTED_EDGE('',*,*,#18382,.F.);
#24942=ORIENTED_EDGE('',*,*,#18362,.F.);
#24943=ORIENTED_EDGE('',*,*,#18365,.F.);
#24944=ORIENTED_EDGE('',*,*,#18367,.F.);
#24945=ORIENTED_EDGE('',*,*,#18369,.F.);
#24946=ORIENTED_EDGE('',*,*,#18383,.F.);
#24947=ORIENTED_EDGE('',*,*,#18384,.F.);
#24948=ORIENTED_EDGE('',*,*,#18385,.F.);
#24949=ORIENTED_EDGE('',*,*,#18386,.F.);
#24950=ORIENTED_EDGE('',*,*,#18353,.T.);
#24951=ORIENTED_EDGE('',*,*,#18387,.T.);
#24952=ORIENTED_EDGE('',*,*,#18383,.T.);
#24953=ORIENTED_EDGE('',*,*,#18368,.F.);
#24954=ORIENTED_EDGE('',*,*,#18345,.T.);
#24955=ORIENTED_EDGE('',*,*,#18388,.T.);
#24956=ORIENTED_EDGE('',*,*,#18379,.T.);
#24957=ORIENTED_EDGE('',*,*,#18377,.F.);
#24958=ORIENTED_EDGE('',*,*,#18358,.T.);
#24959=ORIENTED_EDGE('',*,*,#18363,.T.);
#24960=ORIENTED_EDGE('',*,*,#18386,.T.);
#24961=ORIENTED_EDGE('',*,*,#18389,.F.);
#24962=ORIENTED_EDGE('',*,*,#18359,.T.);
#24963=ORIENTED_EDGE('',*,*,#18389,.T.);
#24964=ORIENTED_EDGE('',*,*,#18385,.T.);
#24965=ORIENTED_EDGE('',*,*,#18390,.F.);
#24966=ORIENTED_EDGE('',*,*,#18360,.T.);
#24967=ORIENTED_EDGE('',*,*,#18390,.T.);
#24968=ORIENTED_EDGE('',*,*,#18384,.T.);
#24969=ORIENTED_EDGE('',*,*,#18387,.F.);
#24970=ORIENTED_EDGE('',*,*,#18350,.T.);
#24971=ORIENTED_EDGE('',*,*,#18372,.T.);
#24972=ORIENTED_EDGE('',*,*,#18382,.T.);
#24973=ORIENTED_EDGE('',*,*,#18391,.F.);
#24974=ORIENTED_EDGE('',*,*,#18381,.T.);
#24975=ORIENTED_EDGE('',*,*,#18392,.F.);
#24976=ORIENTED_EDGE('',*,*,#18351,.F.);
#24977=ORIENTED_EDGE('',*,*,#18391,.T.);
#24978=ORIENTED_EDGE('',*,*,#18352,.T.);
#24979=ORIENTED_EDGE('',*,*,#18392,.T.);
#24980=ORIENTED_EDGE('',*,*,#18380,.T.);
#24981=ORIENTED_EDGE('',*,*,#18388,.F.);
#24982=ORIENTED_EDGE('',*,*,#18393,.T.);
#24983=ORIENTED_EDGE('',*,*,#18394,.F.);
#24984=ORIENTED_EDGE('',*,*,#18395,.F.);
#24985=ORIENTED_EDGE('',*,*,#18396,.T.);
#24986=ORIENTED_EDGE('',*,*,#18397,.T.);
#24987=ORIENTED_EDGE('',*,*,#18398,.F.);
#24988=ORIENTED_EDGE('',*,*,#18399,.F.);
#24989=ORIENTED_EDGE('',*,*,#18394,.T.);
#24990=ORIENTED_EDGE('',*,*,#18400,.T.);
#24991=ORIENTED_EDGE('',*,*,#18401,.F.);
#24992=ORIENTED_EDGE('',*,*,#18402,.F.);
#24993=ORIENTED_EDGE('',*,*,#18398,.T.);
#24994=ORIENTED_EDGE('',*,*,#18403,.T.);
#24995=ORIENTED_EDGE('',*,*,#18404,.F.);
#24996=ORIENTED_EDGE('',*,*,#18405,.F.);
#24997=ORIENTED_EDGE('',*,*,#18401,.T.);
#24998=ORIENTED_EDGE('',*,*,#18406,.T.);
#24999=ORIENTED_EDGE('',*,*,#18407,.F.);
#25000=ORIENTED_EDGE('',*,*,#18408,.F.);
#25001=ORIENTED_EDGE('',*,*,#18409,.T.);
#25002=ORIENTED_EDGE('',*,*,#18410,.T.);
#25003=ORIENTED_EDGE('',*,*,#18411,.F.);
#25004=ORIENTED_EDGE('',*,*,#18412,.F.);
#25005=ORIENTED_EDGE('',*,*,#18407,.T.);
#25006=ORIENTED_EDGE('',*,*,#18413,.T.);
#25007=ORIENTED_EDGE('',*,*,#18414,.F.);
#25008=ORIENTED_EDGE('',*,*,#18415,.F.);
#25009=ORIENTED_EDGE('',*,*,#18411,.T.);
#25010=ORIENTED_EDGE('',*,*,#18416,.T.);
#25011=ORIENTED_EDGE('',*,*,#18417,.F.);
#25012=ORIENTED_EDGE('',*,*,#18418,.F.);
#25013=ORIENTED_EDGE('',*,*,#18414,.T.);
#25014=ORIENTED_EDGE('',*,*,#18419,.T.);
#25015=ORIENTED_EDGE('',*,*,#18420,.F.);
#25016=ORIENTED_EDGE('',*,*,#18421,.F.);
#25017=ORIENTED_EDGE('',*,*,#18404,.T.);
#25018=ORIENTED_EDGE('',*,*,#18422,.T.);
#25019=ORIENTED_EDGE('',*,*,#18396,.F.);
#25020=ORIENTED_EDGE('',*,*,#18423,.F.);
#25021=ORIENTED_EDGE('',*,*,#18424,.T.);
#25022=ORIENTED_EDGE('',*,*,#18425,.T.);
#25023=ORIENTED_EDGE('',*,*,#18424,.F.);
#25024=ORIENTED_EDGE('',*,*,#18426,.F.);
#25025=ORIENTED_EDGE('',*,*,#18427,.T.);
#25026=ORIENTED_EDGE('',*,*,#18428,.T.);
#25027=ORIENTED_EDGE('',*,*,#18427,.F.);
#25028=ORIENTED_EDGE('',*,*,#18429,.F.);
#25029=ORIENTED_EDGE('',*,*,#18420,.T.);
#25030=ORIENTED_EDGE('',*,*,#18430,.T.);
#25031=ORIENTED_EDGE('',*,*,#18431,.F.);
#25032=ORIENTED_EDGE('',*,*,#18432,.F.);
#25033=ORIENTED_EDGE('',*,*,#18417,.T.);
#25034=ORIENTED_EDGE('',*,*,#18433,.T.);
#25035=ORIENTED_EDGE('',*,*,#18434,.F.);
#25036=ORIENTED_EDGE('',*,*,#18435,.F.);
#25037=ORIENTED_EDGE('',*,*,#18431,.T.);
#25038=ORIENTED_EDGE('',*,*,#18436,.T.);
#25039=ORIENTED_EDGE('',*,*,#18437,.F.);
#25040=ORIENTED_EDGE('',*,*,#18438,.F.);
#25041=ORIENTED_EDGE('',*,*,#18434,.T.);
#25042=ORIENTED_EDGE('',*,*,#18439,.T.);
#25043=ORIENTED_EDGE('',*,*,#18409,.F.);
#25044=ORIENTED_EDGE('',*,*,#18440,.F.);
#25045=ORIENTED_EDGE('',*,*,#18437,.T.);
#25046=ORIENTED_EDGE('',*,*,#18432,.T.);
#25047=ORIENTED_EDGE('',*,*,#18435,.T.);
#25048=ORIENTED_EDGE('',*,*,#18438,.T.);
#25049=ORIENTED_EDGE('',*,*,#18440,.T.);
#25050=ORIENTED_EDGE('',*,*,#18408,.T.);
#25051=ORIENTED_EDGE('',*,*,#18412,.T.);
#25052=ORIENTED_EDGE('',*,*,#18415,.T.);
#25053=ORIENTED_EDGE('',*,*,#18418,.T.);
#25054=ORIENTED_EDGE('',*,*,#18421,.T.);
#25055=ORIENTED_EDGE('',*,*,#18429,.T.);
#25056=ORIENTED_EDGE('',*,*,#18426,.T.);
#25057=ORIENTED_EDGE('',*,*,#18423,.T.);
#25058=ORIENTED_EDGE('',*,*,#18395,.T.);
#25059=ORIENTED_EDGE('',*,*,#18399,.T.);
#25060=ORIENTED_EDGE('',*,*,#18402,.T.);
#25061=ORIENTED_EDGE('',*,*,#18405,.T.);
#25062=ORIENTED_EDGE('',*,*,#18430,.F.);
#25063=ORIENTED_EDGE('',*,*,#18416,.F.);
#25064=ORIENTED_EDGE('',*,*,#18413,.F.);
#25065=ORIENTED_EDGE('',*,*,#18410,.F.);
#25066=ORIENTED_EDGE('',*,*,#18406,.F.);
#25067=ORIENTED_EDGE('',*,*,#18439,.F.);
#25068=ORIENTED_EDGE('',*,*,#18436,.F.);
#25069=ORIENTED_EDGE('',*,*,#18433,.F.);
#25070=ORIENTED_EDGE('',*,*,#18419,.F.);
#25071=ORIENTED_EDGE('',*,*,#18403,.F.);
#25072=ORIENTED_EDGE('',*,*,#18400,.F.);
#25073=ORIENTED_EDGE('',*,*,#18397,.F.);
#25074=ORIENTED_EDGE('',*,*,#18393,.F.);
#25075=ORIENTED_EDGE('',*,*,#18422,.F.);
#25076=ORIENTED_EDGE('',*,*,#18425,.F.);
#25077=ORIENTED_EDGE('',*,*,#18428,.F.);
#25078=ORIENTED_EDGE('',*,*,#18441,.T.);
#25079=ORIENTED_EDGE('',*,*,#18442,.F.);
#25080=ORIENTED_EDGE('',*,*,#18443,.F.);
#25081=ORIENTED_EDGE('',*,*,#18444,.T.);
#25082=ORIENTED_EDGE('',*,*,#18445,.T.);
#25083=ORIENTED_EDGE('',*,*,#18446,.F.);
#25084=ORIENTED_EDGE('',*,*,#18447,.F.);
#25085=ORIENTED_EDGE('',*,*,#18442,.T.);
#25086=ORIENTED_EDGE('',*,*,#18448,.T.);
#25087=ORIENTED_EDGE('',*,*,#18449,.F.);
#25088=ORIENTED_EDGE('',*,*,#18450,.F.);
#25089=ORIENTED_EDGE('',*,*,#18446,.T.);
#25090=ORIENTED_EDGE('',*,*,#18451,.T.);
#25091=ORIENTED_EDGE('',*,*,#18452,.F.);
#25092=ORIENTED_EDGE('',*,*,#18453,.F.);
#25093=ORIENTED_EDGE('',*,*,#18449,.T.);
#25094=ORIENTED_EDGE('',*,*,#18454,.T.);
#25095=ORIENTED_EDGE('',*,*,#18455,.F.);
#25096=ORIENTED_EDGE('',*,*,#18456,.F.);
#25097=ORIENTED_EDGE('',*,*,#18457,.T.);
#25098=ORIENTED_EDGE('',*,*,#18458,.T.);
#25099=ORIENTED_EDGE('',*,*,#18459,.F.);
#25100=ORIENTED_EDGE('',*,*,#18460,.F.);
#25101=ORIENTED_EDGE('',*,*,#18455,.T.);
#25102=ORIENTED_EDGE('',*,*,#18461,.T.);
#25103=ORIENTED_EDGE('',*,*,#18462,.F.);
#25104=ORIENTED_EDGE('',*,*,#18463,.F.);
#25105=ORIENTED_EDGE('',*,*,#18459,.T.);
#25106=ORIENTED_EDGE('',*,*,#18464,.T.);
#25107=ORIENTED_EDGE('',*,*,#18465,.F.);
#25108=ORIENTED_EDGE('',*,*,#18466,.F.);
#25109=ORIENTED_EDGE('',*,*,#18462,.T.);
#25110=ORIENTED_EDGE('',*,*,#18467,.T.);
#25111=ORIENTED_EDGE('',*,*,#18468,.F.);
#25112=ORIENTED_EDGE('',*,*,#18469,.F.);
#25113=ORIENTED_EDGE('',*,*,#18452,.T.);
#25114=ORIENTED_EDGE('',*,*,#18470,.T.);
#25115=ORIENTED_EDGE('',*,*,#18444,.F.);
#25116=ORIENTED_EDGE('',*,*,#18471,.F.);
#25117=ORIENTED_EDGE('',*,*,#18472,.T.);
#25118=ORIENTED_EDGE('',*,*,#18473,.T.);
#25119=ORIENTED_EDGE('',*,*,#18472,.F.);
#25120=ORIENTED_EDGE('',*,*,#18474,.F.);
#25121=ORIENTED_EDGE('',*,*,#18475,.T.);
#25122=ORIENTED_EDGE('',*,*,#18476,.T.);
#25123=ORIENTED_EDGE('',*,*,#18475,.F.);
#25124=ORIENTED_EDGE('',*,*,#18477,.F.);
#25125=ORIENTED_EDGE('',*,*,#18468,.T.);
#25126=ORIENTED_EDGE('',*,*,#18478,.T.);
#25127=ORIENTED_EDGE('',*,*,#18479,.F.);
#25128=ORIENTED_EDGE('',*,*,#18480,.F.);
#25129=ORIENTED_EDGE('',*,*,#18465,.T.);
#25130=ORIENTED_EDGE('',*,*,#18481,.T.);
#25131=ORIENTED_EDGE('',*,*,#18482,.F.);
#25132=ORIENTED_EDGE('',*,*,#18483,.F.);
#25133=ORIENTED_EDGE('',*,*,#18479,.T.);
#25134=ORIENTED_EDGE('',*,*,#18484,.T.);
#25135=ORIENTED_EDGE('',*,*,#18485,.F.);
#25136=ORIENTED_EDGE('',*,*,#18486,.F.);
#25137=ORIENTED_EDGE('',*,*,#18482,.T.);
#25138=ORIENTED_EDGE('',*,*,#18487,.T.);
#25139=ORIENTED_EDGE('',*,*,#18457,.F.);
#25140=ORIENTED_EDGE('',*,*,#18488,.F.);
#25141=ORIENTED_EDGE('',*,*,#18485,.T.);
#25142=ORIENTED_EDGE('',*,*,#18480,.T.);
#25143=ORIENTED_EDGE('',*,*,#18483,.T.);
#25144=ORIENTED_EDGE('',*,*,#18486,.T.);
#25145=ORIENTED_EDGE('',*,*,#18488,.T.);
#25146=ORIENTED_EDGE('',*,*,#18456,.T.);
#25147=ORIENTED_EDGE('',*,*,#18460,.T.);
#25148=ORIENTED_EDGE('',*,*,#18463,.T.);
#25149=ORIENTED_EDGE('',*,*,#18466,.T.);
#25150=ORIENTED_EDGE('',*,*,#18469,.T.);
#25151=ORIENTED_EDGE('',*,*,#18477,.T.);
#25152=ORIENTED_EDGE('',*,*,#18474,.T.);
#25153=ORIENTED_EDGE('',*,*,#18471,.T.);
#25154=ORIENTED_EDGE('',*,*,#18443,.T.);
#25155=ORIENTED_EDGE('',*,*,#18447,.T.);
#25156=ORIENTED_EDGE('',*,*,#18450,.T.);
#25157=ORIENTED_EDGE('',*,*,#18453,.T.);
#25158=ORIENTED_EDGE('',*,*,#18478,.F.);
#25159=ORIENTED_EDGE('',*,*,#18464,.F.);
#25160=ORIENTED_EDGE('',*,*,#18461,.F.);
#25161=ORIENTED_EDGE('',*,*,#18458,.F.);
#25162=ORIENTED_EDGE('',*,*,#18454,.F.);
#25163=ORIENTED_EDGE('',*,*,#18487,.F.);
#25164=ORIENTED_EDGE('',*,*,#18484,.F.);
#25165=ORIENTED_EDGE('',*,*,#18481,.F.);
#25166=ORIENTED_EDGE('',*,*,#18467,.F.);
#25167=ORIENTED_EDGE('',*,*,#18451,.F.);
#25168=ORIENTED_EDGE('',*,*,#18448,.F.);
#25169=ORIENTED_EDGE('',*,*,#18445,.F.);
#25170=ORIENTED_EDGE('',*,*,#18441,.F.);
#25171=ORIENTED_EDGE('',*,*,#18470,.F.);
#25172=ORIENTED_EDGE('',*,*,#18473,.F.);
#25173=ORIENTED_EDGE('',*,*,#18476,.F.);
#25174=ORIENTED_EDGE('',*,*,#18489,.T.);
#25175=ORIENTED_EDGE('',*,*,#18490,.F.);
#25176=ORIENTED_EDGE('',*,*,#18491,.F.);
#25177=ORIENTED_EDGE('',*,*,#18492,.T.);
#25178=ORIENTED_EDGE('',*,*,#18493,.T.);
#25179=ORIENTED_EDGE('',*,*,#18494,.F.);
#25180=ORIENTED_EDGE('',*,*,#18495,.F.);
#25181=ORIENTED_EDGE('',*,*,#18490,.T.);
#25182=ORIENTED_EDGE('',*,*,#18496,.T.);
#25183=ORIENTED_EDGE('',*,*,#18497,.F.);
#25184=ORIENTED_EDGE('',*,*,#18498,.F.);
#25185=ORIENTED_EDGE('',*,*,#18494,.T.);
#25186=ORIENTED_EDGE('',*,*,#18499,.T.);
#25187=ORIENTED_EDGE('',*,*,#18500,.F.);
#25188=ORIENTED_EDGE('',*,*,#18501,.F.);
#25189=ORIENTED_EDGE('',*,*,#18497,.T.);
#25190=ORIENTED_EDGE('',*,*,#18502,.T.);
#25191=ORIENTED_EDGE('',*,*,#18503,.F.);
#25192=ORIENTED_EDGE('',*,*,#18504,.F.);
#25193=ORIENTED_EDGE('',*,*,#18505,.T.);
#25194=ORIENTED_EDGE('',*,*,#18506,.T.);
#25195=ORIENTED_EDGE('',*,*,#18507,.F.);
#25196=ORIENTED_EDGE('',*,*,#18508,.F.);
#25197=ORIENTED_EDGE('',*,*,#18503,.T.);
#25198=ORIENTED_EDGE('',*,*,#18509,.T.);
#25199=ORIENTED_EDGE('',*,*,#18510,.F.);
#25200=ORIENTED_EDGE('',*,*,#18511,.F.);
#25201=ORIENTED_EDGE('',*,*,#18507,.T.);
#25202=ORIENTED_EDGE('',*,*,#18512,.T.);
#25203=ORIENTED_EDGE('',*,*,#18513,.F.);
#25204=ORIENTED_EDGE('',*,*,#18514,.F.);
#25205=ORIENTED_EDGE('',*,*,#18510,.T.);
#25206=ORIENTED_EDGE('',*,*,#18515,.T.);
#25207=ORIENTED_EDGE('',*,*,#18516,.F.);
#25208=ORIENTED_EDGE('',*,*,#18517,.F.);
#25209=ORIENTED_EDGE('',*,*,#18500,.T.);
#25210=ORIENTED_EDGE('',*,*,#18518,.T.);
#25211=ORIENTED_EDGE('',*,*,#18492,.F.);
#25212=ORIENTED_EDGE('',*,*,#18519,.F.);
#25213=ORIENTED_EDGE('',*,*,#18520,.T.);
#25214=ORIENTED_EDGE('',*,*,#18521,.T.);
#25215=ORIENTED_EDGE('',*,*,#18520,.F.);
#25216=ORIENTED_EDGE('',*,*,#18522,.F.);
#25217=ORIENTED_EDGE('',*,*,#18523,.T.);
#25218=ORIENTED_EDGE('',*,*,#18524,.T.);
#25219=ORIENTED_EDGE('',*,*,#18523,.F.);
#25220=ORIENTED_EDGE('',*,*,#18525,.F.);
#25221=ORIENTED_EDGE('',*,*,#18516,.T.);
#25222=ORIENTED_EDGE('',*,*,#18526,.T.);
#25223=ORIENTED_EDGE('',*,*,#18527,.F.);
#25224=ORIENTED_EDGE('',*,*,#18528,.F.);
#25225=ORIENTED_EDGE('',*,*,#18513,.T.);
#25226=ORIENTED_EDGE('',*,*,#18529,.T.);
#25227=ORIENTED_EDGE('',*,*,#18530,.F.);
#25228=ORIENTED_EDGE('',*,*,#18531,.F.);
#25229=ORIENTED_EDGE('',*,*,#18527,.T.);
#25230=ORIENTED_EDGE('',*,*,#18532,.T.);
#25231=ORIENTED_EDGE('',*,*,#18533,.F.);
#25232=ORIENTED_EDGE('',*,*,#18534,.F.);
#25233=ORIENTED_EDGE('',*,*,#18530,.T.);
#25234=ORIENTED_EDGE('',*,*,#18535,.T.);
#25235=ORIENTED_EDGE('',*,*,#18505,.F.);
#25236=ORIENTED_EDGE('',*,*,#18536,.F.);
#25237=ORIENTED_EDGE('',*,*,#18533,.T.);
#25238=ORIENTED_EDGE('',*,*,#18528,.T.);
#25239=ORIENTED_EDGE('',*,*,#18531,.T.);
#25240=ORIENTED_EDGE('',*,*,#18534,.T.);
#25241=ORIENTED_EDGE('',*,*,#18536,.T.);
#25242=ORIENTED_EDGE('',*,*,#18504,.T.);
#25243=ORIENTED_EDGE('',*,*,#18508,.T.);
#25244=ORIENTED_EDGE('',*,*,#18511,.T.);
#25245=ORIENTED_EDGE('',*,*,#18514,.T.);
#25246=ORIENTED_EDGE('',*,*,#18517,.T.);
#25247=ORIENTED_EDGE('',*,*,#18525,.T.);
#25248=ORIENTED_EDGE('',*,*,#18522,.T.);
#25249=ORIENTED_EDGE('',*,*,#18519,.T.);
#25250=ORIENTED_EDGE('',*,*,#18491,.T.);
#25251=ORIENTED_EDGE('',*,*,#18495,.T.);
#25252=ORIENTED_EDGE('',*,*,#18498,.T.);
#25253=ORIENTED_EDGE('',*,*,#18501,.T.);
#25254=ORIENTED_EDGE('',*,*,#18526,.F.);
#25255=ORIENTED_EDGE('',*,*,#18512,.F.);
#25256=ORIENTED_EDGE('',*,*,#18509,.F.);
#25257=ORIENTED_EDGE('',*,*,#18506,.F.);
#25258=ORIENTED_EDGE('',*,*,#18502,.F.);
#25259=ORIENTED_EDGE('',*,*,#18535,.F.);
#25260=ORIENTED_EDGE('',*,*,#18532,.F.);
#25261=ORIENTED_EDGE('',*,*,#18529,.F.);
#25262=ORIENTED_EDGE('',*,*,#18515,.F.);
#25263=ORIENTED_EDGE('',*,*,#18499,.F.);
#25264=ORIENTED_EDGE('',*,*,#18496,.F.);
#25265=ORIENTED_EDGE('',*,*,#18493,.F.);
#25266=ORIENTED_EDGE('',*,*,#18489,.F.);
#25267=ORIENTED_EDGE('',*,*,#18518,.F.);
#25268=ORIENTED_EDGE('',*,*,#18521,.F.);
#25269=ORIENTED_EDGE('',*,*,#18524,.F.);
#25270=ORIENTED_EDGE('',*,*,#18537,.F.);
#25271=ORIENTED_EDGE('',*,*,#18538,.T.);
#25272=ORIENTED_EDGE('',*,*,#18539,.F.);
#25273=ORIENTED_EDGE('',*,*,#18540,.F.);
#25274=ORIENTED_EDGE('',*,*,#18541,.F.);
#25275=ORIENTED_EDGE('',*,*,#18542,.T.);
#25276=ORIENTED_EDGE('',*,*,#18543,.F.);
#25277=ORIENTED_EDGE('',*,*,#18538,.F.);
#25278=ORIENTED_EDGE('',*,*,#18544,.F.);
#25279=ORIENTED_EDGE('',*,*,#18545,.T.);
#25280=ORIENTED_EDGE('',*,*,#18546,.F.);
#25281=ORIENTED_EDGE('',*,*,#18542,.F.);
#25282=ORIENTED_EDGE('',*,*,#18547,.F.);
#25283=ORIENTED_EDGE('',*,*,#18548,.T.);
#25284=ORIENTED_EDGE('',*,*,#18549,.F.);
#25285=ORIENTED_EDGE('',*,*,#18545,.F.);
#25286=ORIENTED_EDGE('',*,*,#18550,.F.);
#25287=ORIENTED_EDGE('',*,*,#18551,.T.);
#25288=ORIENTED_EDGE('',*,*,#18552,.F.);
#25289=ORIENTED_EDGE('',*,*,#18548,.F.);
#25290=ORIENTED_EDGE('',*,*,#18553,.F.);
#25291=ORIENTED_EDGE('',*,*,#18554,.T.);
#25292=ORIENTED_EDGE('',*,*,#18555,.F.);
#25293=ORIENTED_EDGE('',*,*,#18551,.F.);
#25294=ORIENTED_EDGE('',*,*,#18556,.F.);
#25295=ORIENTED_EDGE('',*,*,#18557,.T.);
#25296=ORIENTED_EDGE('',*,*,#18558,.F.);
#25297=ORIENTED_EDGE('',*,*,#18554,.F.);
#25298=ORIENTED_EDGE('',*,*,#18559,.F.);
#25299=ORIENTED_EDGE('',*,*,#18540,.T.);
#25300=ORIENTED_EDGE('',*,*,#18560,.F.);
#25301=ORIENTED_EDGE('',*,*,#18557,.F.);
#25302=ORIENTED_EDGE('',*,*,#18561,.F.);
#25303=ORIENTED_EDGE('',*,*,#18562,.T.);
#25304=ORIENTED_EDGE('',*,*,#18563,.F.);
#25305=ORIENTED_EDGE('',*,*,#18564,.F.);
#25306=ORIENTED_EDGE('',*,*,#18565,.F.);
#25307=ORIENTED_EDGE('',*,*,#18564,.T.);
#25308=ORIENTED_EDGE('',*,*,#18566,.F.);
#25309=ORIENTED_EDGE('',*,*,#18567,.F.);
#25310=ORIENTED_EDGE('',*,*,#18568,.F.);
#25311=ORIENTED_EDGE('',*,*,#18567,.T.);
#25312=ORIENTED_EDGE('',*,*,#18569,.F.);
#25313=ORIENTED_EDGE('',*,*,#18570,.F.);
#25314=ORIENTED_EDGE('',*,*,#18571,.F.);
#25315=ORIENTED_EDGE('',*,*,#18570,.T.);
#25316=ORIENTED_EDGE('',*,*,#18572,.F.);
#25317=ORIENTED_EDGE('',*,*,#18573,.F.);
#25318=ORIENTED_EDGE('',*,*,#18574,.F.);
#25319=ORIENTED_EDGE('',*,*,#18573,.T.);
#25320=ORIENTED_EDGE('',*,*,#18575,.F.);
#25321=ORIENTED_EDGE('',*,*,#18576,.F.);
#25322=ORIENTED_EDGE('',*,*,#18577,.F.);
#25323=ORIENTED_EDGE('',*,*,#18576,.T.);
#25324=ORIENTED_EDGE('',*,*,#18578,.F.);
#25325=ORIENTED_EDGE('',*,*,#18579,.F.);
#25326=ORIENTED_EDGE('',*,*,#18580,.F.);
#25327=ORIENTED_EDGE('',*,*,#18579,.T.);
#25328=ORIENTED_EDGE('',*,*,#18581,.F.);
#25329=ORIENTED_EDGE('',*,*,#18582,.F.);
#25330=ORIENTED_EDGE('',*,*,#18583,.F.);
#25331=ORIENTED_EDGE('',*,*,#18582,.T.);
#25332=ORIENTED_EDGE('',*,*,#18584,.F.);
#25333=ORIENTED_EDGE('',*,*,#18562,.F.);
#25334=ORIENTED_EDGE('',*,*,#18583,.T.);
#25335=ORIENTED_EDGE('',*,*,#18561,.T.);
#25336=ORIENTED_EDGE('',*,*,#18565,.T.);
#25337=ORIENTED_EDGE('',*,*,#18568,.T.);
#25338=ORIENTED_EDGE('',*,*,#18571,.T.);
#25339=ORIENTED_EDGE('',*,*,#18574,.T.);
#25340=ORIENTED_EDGE('',*,*,#18577,.T.);
#25341=ORIENTED_EDGE('',*,*,#18580,.T.);
#25342=ORIENTED_EDGE('',*,*,#18537,.T.);
#25343=ORIENTED_EDGE('',*,*,#18559,.T.);
#25344=ORIENTED_EDGE('',*,*,#18556,.T.);
#25345=ORIENTED_EDGE('',*,*,#18553,.T.);
#25346=ORIENTED_EDGE('',*,*,#18550,.T.);
#25347=ORIENTED_EDGE('',*,*,#18547,.T.);
#25348=ORIENTED_EDGE('',*,*,#18544,.T.);
#25349=ORIENTED_EDGE('',*,*,#18541,.T.);
#25350=ORIENTED_EDGE('',*,*,#18584,.T.);
#25351=ORIENTED_EDGE('',*,*,#18581,.T.);
#25352=ORIENTED_EDGE('',*,*,#18578,.T.);
#25353=ORIENTED_EDGE('',*,*,#18575,.T.);
#25354=ORIENTED_EDGE('',*,*,#18572,.T.);
#25355=ORIENTED_EDGE('',*,*,#18569,.T.);
#25356=ORIENTED_EDGE('',*,*,#18566,.T.);
#25357=ORIENTED_EDGE('',*,*,#18563,.T.);
#25358=ORIENTED_EDGE('',*,*,#18539,.T.);
#25359=ORIENTED_EDGE('',*,*,#18543,.T.);
#25360=ORIENTED_EDGE('',*,*,#18546,.T.);
#25361=ORIENTED_EDGE('',*,*,#18549,.T.);
#25362=ORIENTED_EDGE('',*,*,#18552,.T.);
#25363=ORIENTED_EDGE('',*,*,#18555,.T.);
#25364=ORIENTED_EDGE('',*,*,#18558,.T.);
#25365=ORIENTED_EDGE('',*,*,#18560,.T.);
#25366=ORIENTED_EDGE('',*,*,#18585,.F.);
#25367=ORIENTED_EDGE('',*,*,#18586,.T.);
#25368=ORIENTED_EDGE('',*,*,#18587,.F.);
#25369=ORIENTED_EDGE('',*,*,#18588,.F.);
#25370=ORIENTED_EDGE('',*,*,#18589,.F.);
#25371=ORIENTED_EDGE('',*,*,#18590,.T.);
#25372=ORIENTED_EDGE('',*,*,#18591,.F.);
#25373=ORIENTED_EDGE('',*,*,#18586,.F.);
#25374=ORIENTED_EDGE('',*,*,#18592,.F.);
#25375=ORIENTED_EDGE('',*,*,#18593,.T.);
#25376=ORIENTED_EDGE('',*,*,#18594,.F.);
#25377=ORIENTED_EDGE('',*,*,#18590,.F.);
#25378=ORIENTED_EDGE('',*,*,#18595,.F.);
#25379=ORIENTED_EDGE('',*,*,#18596,.T.);
#25380=ORIENTED_EDGE('',*,*,#18597,.F.);
#25381=ORIENTED_EDGE('',*,*,#18593,.F.);
#25382=ORIENTED_EDGE('',*,*,#18598,.F.);
#25383=ORIENTED_EDGE('',*,*,#18599,.T.);
#25384=ORIENTED_EDGE('',*,*,#18600,.F.);
#25385=ORIENTED_EDGE('',*,*,#18596,.F.);
#25386=ORIENTED_EDGE('',*,*,#18601,.F.);
#25387=ORIENTED_EDGE('',*,*,#18602,.T.);
#25388=ORIENTED_EDGE('',*,*,#18603,.F.);
#25389=ORIENTED_EDGE('',*,*,#18599,.F.);
#25390=ORIENTED_EDGE('',*,*,#18604,.F.);
#25391=ORIENTED_EDGE('',*,*,#18605,.T.);
#25392=ORIENTED_EDGE('',*,*,#18606,.F.);
#25393=ORIENTED_EDGE('',*,*,#18602,.F.);
#25394=ORIENTED_EDGE('',*,*,#18607,.F.);
#25395=ORIENTED_EDGE('',*,*,#18588,.T.);
#25396=ORIENTED_EDGE('',*,*,#18608,.F.);
#25397=ORIENTED_EDGE('',*,*,#18605,.F.);
#25398=ORIENTED_EDGE('',*,*,#18609,.F.);
#25399=ORIENTED_EDGE('',*,*,#18610,.T.);
#25400=ORIENTED_EDGE('',*,*,#18611,.F.);
#25401=ORIENTED_EDGE('',*,*,#18612,.F.);
#25402=ORIENTED_EDGE('',*,*,#18613,.F.);
#25403=ORIENTED_EDGE('',*,*,#18612,.T.);
#25404=ORIENTED_EDGE('',*,*,#18614,.F.);
#25405=ORIENTED_EDGE('',*,*,#18615,.F.);
#25406=ORIENTED_EDGE('',*,*,#18616,.F.);
#25407=ORIENTED_EDGE('',*,*,#18615,.T.);
#25408=ORIENTED_EDGE('',*,*,#18617,.F.);
#25409=ORIENTED_EDGE('',*,*,#18618,.F.);
#25410=ORIENTED_EDGE('',*,*,#18619,.F.);
#25411=ORIENTED_EDGE('',*,*,#18618,.T.);
#25412=ORIENTED_EDGE('',*,*,#18620,.F.);
#25413=ORIENTED_EDGE('',*,*,#18621,.F.);
#25414=ORIENTED_EDGE('',*,*,#18622,.F.);
#25415=ORIENTED_EDGE('',*,*,#18621,.T.);
#25416=ORIENTED_EDGE('',*,*,#18623,.F.);
#25417=ORIENTED_EDGE('',*,*,#18624,.F.);
#25418=ORIENTED_EDGE('',*,*,#18625,.F.);
#25419=ORIENTED_EDGE('',*,*,#18624,.T.);
#25420=ORIENTED_EDGE('',*,*,#18626,.F.);
#25421=ORIENTED_EDGE('',*,*,#18627,.F.);
#25422=ORIENTED_EDGE('',*,*,#18628,.F.);
#25423=ORIENTED_EDGE('',*,*,#18627,.T.);
#25424=ORIENTED_EDGE('',*,*,#18629,.F.);
#25425=ORIENTED_EDGE('',*,*,#18630,.F.);
#25426=ORIENTED_EDGE('',*,*,#18631,.F.);
#25427=ORIENTED_EDGE('',*,*,#18630,.T.);
#25428=ORIENTED_EDGE('',*,*,#18632,.F.);
#25429=ORIENTED_EDGE('',*,*,#18610,.F.);
#25430=ORIENTED_EDGE('',*,*,#18631,.T.);
#25431=ORIENTED_EDGE('',*,*,#18609,.T.);
#25432=ORIENTED_EDGE('',*,*,#18613,.T.);
#25433=ORIENTED_EDGE('',*,*,#18616,.T.);
#25434=ORIENTED_EDGE('',*,*,#18619,.T.);
#25435=ORIENTED_EDGE('',*,*,#18622,.T.);
#25436=ORIENTED_EDGE('',*,*,#18625,.T.);
#25437=ORIENTED_EDGE('',*,*,#18628,.T.);
#25438=ORIENTED_EDGE('',*,*,#18585,.T.);
#25439=ORIENTED_EDGE('',*,*,#18607,.T.);
#25440=ORIENTED_EDGE('',*,*,#18604,.T.);
#25441=ORIENTED_EDGE('',*,*,#18601,.T.);
#25442=ORIENTED_EDGE('',*,*,#18598,.T.);
#25443=ORIENTED_EDGE('',*,*,#18595,.T.);
#25444=ORIENTED_EDGE('',*,*,#18592,.T.);
#25445=ORIENTED_EDGE('',*,*,#18589,.T.);
#25446=ORIENTED_EDGE('',*,*,#18632,.T.);
#25447=ORIENTED_EDGE('',*,*,#18629,.T.);
#25448=ORIENTED_EDGE('',*,*,#18626,.T.);
#25449=ORIENTED_EDGE('',*,*,#18623,.T.);
#25450=ORIENTED_EDGE('',*,*,#18620,.T.);
#25451=ORIENTED_EDGE('',*,*,#18617,.T.);
#25452=ORIENTED_EDGE('',*,*,#18614,.T.);
#25453=ORIENTED_EDGE('',*,*,#18611,.T.);
#25454=ORIENTED_EDGE('',*,*,#18587,.T.);
#25455=ORIENTED_EDGE('',*,*,#18591,.T.);
#25456=ORIENTED_EDGE('',*,*,#18594,.T.);
#25457=ORIENTED_EDGE('',*,*,#18597,.T.);
#25458=ORIENTED_EDGE('',*,*,#18600,.T.);
#25459=ORIENTED_EDGE('',*,*,#18603,.T.);
#25460=ORIENTED_EDGE('',*,*,#18606,.T.);
#25461=ORIENTED_EDGE('',*,*,#18608,.T.);
#25462=ORIENTED_EDGE('',*,*,#18633,.F.);
#25463=ORIENTED_EDGE('',*,*,#18634,.T.);
#25464=ORIENTED_EDGE('',*,*,#18635,.F.);
#25465=ORIENTED_EDGE('',*,*,#18636,.F.);
#25466=ORIENTED_EDGE('',*,*,#18637,.F.);
#25467=ORIENTED_EDGE('',*,*,#18638,.T.);
#25468=ORIENTED_EDGE('',*,*,#18639,.F.);
#25469=ORIENTED_EDGE('',*,*,#18634,.F.);
#25470=ORIENTED_EDGE('',*,*,#18640,.F.);
#25471=ORIENTED_EDGE('',*,*,#18641,.T.);
#25472=ORIENTED_EDGE('',*,*,#18642,.F.);
#25473=ORIENTED_EDGE('',*,*,#18638,.F.);
#25474=ORIENTED_EDGE('',*,*,#18643,.F.);
#25475=ORIENTED_EDGE('',*,*,#18644,.T.);
#25476=ORIENTED_EDGE('',*,*,#18645,.F.);
#25477=ORIENTED_EDGE('',*,*,#18641,.F.);
#25478=ORIENTED_EDGE('',*,*,#18646,.F.);
#25479=ORIENTED_EDGE('',*,*,#18647,.T.);
#25480=ORIENTED_EDGE('',*,*,#18648,.F.);
#25481=ORIENTED_EDGE('',*,*,#18644,.F.);
#25482=ORIENTED_EDGE('',*,*,#18649,.F.);
#25483=ORIENTED_EDGE('',*,*,#18650,.T.);
#25484=ORIENTED_EDGE('',*,*,#18651,.F.);
#25485=ORIENTED_EDGE('',*,*,#18647,.F.);
#25486=ORIENTED_EDGE('',*,*,#18652,.F.);
#25487=ORIENTED_EDGE('',*,*,#18653,.T.);
#25488=ORIENTED_EDGE('',*,*,#18654,.F.);
#25489=ORIENTED_EDGE('',*,*,#18650,.F.);
#25490=ORIENTED_EDGE('',*,*,#18655,.F.);
#25491=ORIENTED_EDGE('',*,*,#18636,.T.);
#25492=ORIENTED_EDGE('',*,*,#18656,.F.);
#25493=ORIENTED_EDGE('',*,*,#18653,.F.);
#25494=ORIENTED_EDGE('',*,*,#18657,.F.);
#25495=ORIENTED_EDGE('',*,*,#18658,.T.);
#25496=ORIENTED_EDGE('',*,*,#18659,.F.);
#25497=ORIENTED_EDGE('',*,*,#18660,.F.);
#25498=ORIENTED_EDGE('',*,*,#18661,.F.);
#25499=ORIENTED_EDGE('',*,*,#18660,.T.);
#25500=ORIENTED_EDGE('',*,*,#18662,.F.);
#25501=ORIENTED_EDGE('',*,*,#18663,.F.);
#25502=ORIENTED_EDGE('',*,*,#18664,.F.);
#25503=ORIENTED_EDGE('',*,*,#18663,.T.);
#25504=ORIENTED_EDGE('',*,*,#18665,.F.);
#25505=ORIENTED_EDGE('',*,*,#18666,.F.);
#25506=ORIENTED_EDGE('',*,*,#18667,.F.);
#25507=ORIENTED_EDGE('',*,*,#18666,.T.);
#25508=ORIENTED_EDGE('',*,*,#18668,.F.);
#25509=ORIENTED_EDGE('',*,*,#18669,.F.);
#25510=ORIENTED_EDGE('',*,*,#18670,.F.);
#25511=ORIENTED_EDGE('',*,*,#18669,.T.);
#25512=ORIENTED_EDGE('',*,*,#18671,.F.);
#25513=ORIENTED_EDGE('',*,*,#18672,.F.);
#25514=ORIENTED_EDGE('',*,*,#18673,.F.);
#25515=ORIENTED_EDGE('',*,*,#18672,.T.);
#25516=ORIENTED_EDGE('',*,*,#18674,.F.);
#25517=ORIENTED_EDGE('',*,*,#18675,.F.);
#25518=ORIENTED_EDGE('',*,*,#18676,.F.);
#25519=ORIENTED_EDGE('',*,*,#18675,.T.);
#25520=ORIENTED_EDGE('',*,*,#18677,.F.);
#25521=ORIENTED_EDGE('',*,*,#18678,.F.);
#25522=ORIENTED_EDGE('',*,*,#18679,.F.);
#25523=ORIENTED_EDGE('',*,*,#18678,.T.);
#25524=ORIENTED_EDGE('',*,*,#18680,.F.);
#25525=ORIENTED_EDGE('',*,*,#18658,.F.);
#25526=ORIENTED_EDGE('',*,*,#18679,.T.);
#25527=ORIENTED_EDGE('',*,*,#18657,.T.);
#25528=ORIENTED_EDGE('',*,*,#18661,.T.);
#25529=ORIENTED_EDGE('',*,*,#18664,.T.);
#25530=ORIENTED_EDGE('',*,*,#18667,.T.);
#25531=ORIENTED_EDGE('',*,*,#18670,.T.);
#25532=ORIENTED_EDGE('',*,*,#18673,.T.);
#25533=ORIENTED_EDGE('',*,*,#18676,.T.);
#25534=ORIENTED_EDGE('',*,*,#18633,.T.);
#25535=ORIENTED_EDGE('',*,*,#18655,.T.);
#25536=ORIENTED_EDGE('',*,*,#18652,.T.);
#25537=ORIENTED_EDGE('',*,*,#18649,.T.);
#25538=ORIENTED_EDGE('',*,*,#18646,.T.);
#25539=ORIENTED_EDGE('',*,*,#18643,.T.);
#25540=ORIENTED_EDGE('',*,*,#18640,.T.);
#25541=ORIENTED_EDGE('',*,*,#18637,.T.);
#25542=ORIENTED_EDGE('',*,*,#18680,.T.);
#25543=ORIENTED_EDGE('',*,*,#18677,.T.);
#25544=ORIENTED_EDGE('',*,*,#18674,.T.);
#25545=ORIENTED_EDGE('',*,*,#18671,.T.);
#25546=ORIENTED_EDGE('',*,*,#18668,.T.);
#25547=ORIENTED_EDGE('',*,*,#18665,.T.);
#25548=ORIENTED_EDGE('',*,*,#18662,.T.);
#25549=ORIENTED_EDGE('',*,*,#18659,.T.);
#25550=ORIENTED_EDGE('',*,*,#18635,.T.);
#25551=ORIENTED_EDGE('',*,*,#18639,.T.);
#25552=ORIENTED_EDGE('',*,*,#18642,.T.);
#25553=ORIENTED_EDGE('',*,*,#18645,.T.);
#25554=ORIENTED_EDGE('',*,*,#18648,.T.);
#25555=ORIENTED_EDGE('',*,*,#18651,.T.);
#25556=ORIENTED_EDGE('',*,*,#18654,.T.);
#25557=ORIENTED_EDGE('',*,*,#18656,.T.);
#25558=ORIENTED_EDGE('',*,*,#18681,.F.);
#25559=ORIENTED_EDGE('',*,*,#18682,.T.);
#25560=ORIENTED_EDGE('',*,*,#18683,.F.);
#25561=ORIENTED_EDGE('',*,*,#18684,.F.);
#25562=ORIENTED_EDGE('',*,*,#18685,.F.);
#25563=ORIENTED_EDGE('',*,*,#18686,.T.);
#25564=ORIENTED_EDGE('',*,*,#18687,.F.);
#25565=ORIENTED_EDGE('',*,*,#18682,.F.);
#25566=ORIENTED_EDGE('',*,*,#18688,.F.);
#25567=ORIENTED_EDGE('',*,*,#18689,.T.);
#25568=ORIENTED_EDGE('',*,*,#18690,.F.);
#25569=ORIENTED_EDGE('',*,*,#18686,.F.);
#25570=ORIENTED_EDGE('',*,*,#18691,.F.);
#25571=ORIENTED_EDGE('',*,*,#18692,.T.);
#25572=ORIENTED_EDGE('',*,*,#18693,.F.);
#25573=ORIENTED_EDGE('',*,*,#18689,.F.);
#25574=ORIENTED_EDGE('',*,*,#18694,.F.);
#25575=ORIENTED_EDGE('',*,*,#18695,.T.);
#25576=ORIENTED_EDGE('',*,*,#18696,.F.);
#25577=ORIENTED_EDGE('',*,*,#18692,.F.);
#25578=ORIENTED_EDGE('',*,*,#18697,.F.);
#25579=ORIENTED_EDGE('',*,*,#18698,.T.);
#25580=ORIENTED_EDGE('',*,*,#18699,.F.);
#25581=ORIENTED_EDGE('',*,*,#18695,.F.);
#25582=ORIENTED_EDGE('',*,*,#18700,.F.);
#25583=ORIENTED_EDGE('',*,*,#18701,.T.);
#25584=ORIENTED_EDGE('',*,*,#18702,.F.);
#25585=ORIENTED_EDGE('',*,*,#18698,.F.);
#25586=ORIENTED_EDGE('',*,*,#18703,.F.);
#25587=ORIENTED_EDGE('',*,*,#18684,.T.);
#25588=ORIENTED_EDGE('',*,*,#18704,.F.);
#25589=ORIENTED_EDGE('',*,*,#18701,.F.);
#25590=ORIENTED_EDGE('',*,*,#18705,.F.);
#25591=ORIENTED_EDGE('',*,*,#18706,.T.);
#25592=ORIENTED_EDGE('',*,*,#18707,.F.);
#25593=ORIENTED_EDGE('',*,*,#18708,.F.);
#25594=ORIENTED_EDGE('',*,*,#18709,.F.);
#25595=ORIENTED_EDGE('',*,*,#18708,.T.);
#25596=ORIENTED_EDGE('',*,*,#18710,.F.);
#25597=ORIENTED_EDGE('',*,*,#18711,.F.);
#25598=ORIENTED_EDGE('',*,*,#18712,.F.);
#25599=ORIENTED_EDGE('',*,*,#18711,.T.);
#25600=ORIENTED_EDGE('',*,*,#18713,.F.);
#25601=ORIENTED_EDGE('',*,*,#18714,.F.);
#25602=ORIENTED_EDGE('',*,*,#18715,.F.);
#25603=ORIENTED_EDGE('',*,*,#18714,.T.);
#25604=ORIENTED_EDGE('',*,*,#18716,.F.);
#25605=ORIENTED_EDGE('',*,*,#18717,.F.);
#25606=ORIENTED_EDGE('',*,*,#18718,.F.);
#25607=ORIENTED_EDGE('',*,*,#18717,.T.);
#25608=ORIENTED_EDGE('',*,*,#18719,.F.);
#25609=ORIENTED_EDGE('',*,*,#18720,.F.);
#25610=ORIENTED_EDGE('',*,*,#18721,.F.);
#25611=ORIENTED_EDGE('',*,*,#18720,.T.);
#25612=ORIENTED_EDGE('',*,*,#18722,.F.);
#25613=ORIENTED_EDGE('',*,*,#18723,.F.);
#25614=ORIENTED_EDGE('',*,*,#18724,.F.);
#25615=ORIENTED_EDGE('',*,*,#18723,.T.);
#25616=ORIENTED_EDGE('',*,*,#18725,.F.);
#25617=ORIENTED_EDGE('',*,*,#18726,.F.);
#25618=ORIENTED_EDGE('',*,*,#18727,.F.);
#25619=ORIENTED_EDGE('',*,*,#18726,.T.);
#25620=ORIENTED_EDGE('',*,*,#18728,.F.);
#25621=ORIENTED_EDGE('',*,*,#18706,.F.);
#25622=ORIENTED_EDGE('',*,*,#18727,.T.);
#25623=ORIENTED_EDGE('',*,*,#18705,.T.);
#25624=ORIENTED_EDGE('',*,*,#18709,.T.);
#25625=ORIENTED_EDGE('',*,*,#18712,.T.);
#25626=ORIENTED_EDGE('',*,*,#18715,.T.);
#25627=ORIENTED_EDGE('',*,*,#18718,.T.);
#25628=ORIENTED_EDGE('',*,*,#18721,.T.);
#25629=ORIENTED_EDGE('',*,*,#18724,.T.);
#25630=ORIENTED_EDGE('',*,*,#18681,.T.);
#25631=ORIENTED_EDGE('',*,*,#18703,.T.);
#25632=ORIENTED_EDGE('',*,*,#18700,.T.);
#25633=ORIENTED_EDGE('',*,*,#18697,.T.);
#25634=ORIENTED_EDGE('',*,*,#18694,.T.);
#25635=ORIENTED_EDGE('',*,*,#18691,.T.);
#25636=ORIENTED_EDGE('',*,*,#18688,.T.);
#25637=ORIENTED_EDGE('',*,*,#18685,.T.);
#25638=ORIENTED_EDGE('',*,*,#18728,.T.);
#25639=ORIENTED_EDGE('',*,*,#18725,.T.);
#25640=ORIENTED_EDGE('',*,*,#18722,.T.);
#25641=ORIENTED_EDGE('',*,*,#18719,.T.);
#25642=ORIENTED_EDGE('',*,*,#18716,.T.);
#25643=ORIENTED_EDGE('',*,*,#18713,.T.);
#25644=ORIENTED_EDGE('',*,*,#18710,.T.);
#25645=ORIENTED_EDGE('',*,*,#18707,.T.);
#25646=ORIENTED_EDGE('',*,*,#18683,.T.);
#25647=ORIENTED_EDGE('',*,*,#18687,.T.);
#25648=ORIENTED_EDGE('',*,*,#18690,.T.);
#25649=ORIENTED_EDGE('',*,*,#18693,.T.);
#25650=ORIENTED_EDGE('',*,*,#18696,.T.);
#25651=ORIENTED_EDGE('',*,*,#18699,.T.);
#25652=ORIENTED_EDGE('',*,*,#18702,.T.);
#25653=ORIENTED_EDGE('',*,*,#18704,.T.);
#25654=ORIENTED_EDGE('',*,*,#18729,.F.);
#25655=ORIENTED_EDGE('',*,*,#18730,.T.);
#25656=ORIENTED_EDGE('',*,*,#18731,.F.);
#25657=ORIENTED_EDGE('',*,*,#18730,.F.);
#25658=ORIENTED_EDGE('',*,*,#18732,.F.);
#25659=ORIENTED_EDGE('',*,*,#18733,.T.);
#25660=ORIENTED_EDGE('',*,*,#18734,.F.);
#25661=ORIENTED_EDGE('',*,*,#18733,.F.);
#25662=ORIENTED_EDGE('',*,*,#18735,.F.);
#25663=ORIENTED_EDGE('',*,*,#18736,.T.);
#25664=ORIENTED_EDGE('',*,*,#18737,.F.);
#25665=ORIENTED_EDGE('',*,*,#18736,.F.);
#25666=ORIENTED_EDGE('',*,*,#18738,.F.);
#25667=ORIENTED_EDGE('',*,*,#18739,.T.);
#25668=ORIENTED_EDGE('',*,*,#18740,.F.);
#25669=ORIENTED_EDGE('',*,*,#18739,.F.);
#25670=ORIENTED_EDGE('',*,*,#18741,.F.);
#25671=ORIENTED_EDGE('',*,*,#18742,.T.);
#25672=ORIENTED_EDGE('',*,*,#18743,.F.);
#25673=ORIENTED_EDGE('',*,*,#18742,.F.);
#25674=ORIENTED_EDGE('',*,*,#18744,.F.);
#25675=ORIENTED_EDGE('',*,*,#18745,.T.);
#25676=ORIENTED_EDGE('',*,*,#18746,.F.);
#25677=ORIENTED_EDGE('',*,*,#18745,.F.);
#25678=ORIENTED_EDGE('',*,*,#18747,.F.);
#25679=ORIENTED_EDGE('',*,*,#18748,.T.);
#25680=ORIENTED_EDGE('',*,*,#18749,.F.);
#25681=ORIENTED_EDGE('',*,*,#18748,.F.);
#25682=ORIENTED_EDGE('',*,*,#18750,.F.);
#25683=ORIENTED_EDGE('',*,*,#18751,.T.);
#25684=ORIENTED_EDGE('',*,*,#18752,.F.);
#25685=ORIENTED_EDGE('',*,*,#18751,.F.);
#25686=ORIENTED_EDGE('',*,*,#18753,.F.);
#25687=ORIENTED_EDGE('',*,*,#18754,.T.);
#25688=ORIENTED_EDGE('',*,*,#18755,.F.);
#25689=ORIENTED_EDGE('',*,*,#18754,.F.);
#25690=ORIENTED_EDGE('',*,*,#18756,.F.);
#25691=ORIENTED_EDGE('',*,*,#18757,.T.);
#25692=ORIENTED_EDGE('',*,*,#18758,.F.);
#25693=ORIENTED_EDGE('',*,*,#18757,.F.);
#25694=ORIENTED_EDGE('',*,*,#18759,.F.);
#25695=ORIENTED_EDGE('',*,*,#18760,.T.);
#25696=ORIENTED_EDGE('',*,*,#18761,.F.);
#25697=ORIENTED_EDGE('',*,*,#18760,.F.);
#25698=ORIENTED_EDGE('',*,*,#18762,.F.);
#25699=ORIENTED_EDGE('',*,*,#18763,.T.);
#25700=ORIENTED_EDGE('',*,*,#18764,.F.);
#25701=ORIENTED_EDGE('',*,*,#18763,.F.);
#25702=ORIENTED_EDGE('',*,*,#18765,.F.);
#25703=ORIENTED_EDGE('',*,*,#18766,.T.);
#25704=ORIENTED_EDGE('',*,*,#18767,.F.);
#25705=ORIENTED_EDGE('',*,*,#18766,.F.);
#25706=ORIENTED_EDGE('',*,*,#18768,.F.);
#25707=ORIENTED_EDGE('',*,*,#18769,.T.);
#25708=ORIENTED_EDGE('',*,*,#18770,.F.);
#25709=ORIENTED_EDGE('',*,*,#18769,.F.);
#25710=ORIENTED_EDGE('',*,*,#18771,.F.);
#25711=ORIENTED_EDGE('',*,*,#18772,.T.);
#25712=ORIENTED_EDGE('',*,*,#18773,.F.);
#25713=ORIENTED_EDGE('',*,*,#18772,.F.);
#25714=ORIENTED_EDGE('',*,*,#18774,.F.);
#25715=ORIENTED_EDGE('',*,*,#18775,.T.);
#25716=ORIENTED_EDGE('',*,*,#18776,.F.);
#25717=ORIENTED_EDGE('',*,*,#18775,.F.);
#25718=ORIENTED_EDGE('',*,*,#18777,.T.);
#25719=ORIENTED_EDGE('',*,*,#18778,.F.);
#25720=ORIENTED_EDGE('',*,*,#18779,.T.);
#25721=ORIENTED_EDGE('',*,*,#18780,.F.);
#25722=ORIENTED_EDGE('',*,*,#18734,.T.);
#25723=ORIENTED_EDGE('',*,*,#18740,.T.);
#25724=ORIENTED_EDGE('',*,*,#18746,.T.);
#25725=ORIENTED_EDGE('',*,*,#18752,.T.);
#25726=ORIENTED_EDGE('',*,*,#18758,.T.);
#25727=ORIENTED_EDGE('',*,*,#18764,.T.);
#25728=ORIENTED_EDGE('',*,*,#18770,.T.);
#25729=ORIENTED_EDGE('',*,*,#18776,.T.);
#25730=ORIENTED_EDGE('',*,*,#18779,.F.);
#25731=ORIENTED_EDGE('',*,*,#18781,.F.);
#25732=ORIENTED_EDGE('',*,*,#18782,.T.);
#25733=ORIENTED_EDGE('',*,*,#18783,.F.);
#25734=ORIENTED_EDGE('',*,*,#18782,.F.);
#25735=ORIENTED_EDGE('',*,*,#18784,.F.);
#25736=ORIENTED_EDGE('',*,*,#18785,.T.);
#25737=ORIENTED_EDGE('',*,*,#18786,.F.);
#25738=ORIENTED_EDGE('',*,*,#18729,.T.);
#25739=ORIENTED_EDGE('',*,*,#18735,.T.);
#25740=ORIENTED_EDGE('',*,*,#18741,.T.);
#25741=ORIENTED_EDGE('',*,*,#18747,.T.);
#25742=ORIENTED_EDGE('',*,*,#18753,.T.);
#25743=ORIENTED_EDGE('',*,*,#18759,.T.);
#25744=ORIENTED_EDGE('',*,*,#18765,.T.);
#25745=ORIENTED_EDGE('',*,*,#18771,.T.);
#25746=ORIENTED_EDGE('',*,*,#18785,.F.);
#25747=ORIENTED_EDGE('',*,*,#18787,.F.);
#25748=ORIENTED_EDGE('',*,*,#18777,.F.);
#25749=ORIENTED_EDGE('',*,*,#18788,.F.);
#25750=ORIENTED_EDGE('',*,*,#18789,.T.);
#25751=ORIENTED_EDGE('',*,*,#18790,.T.);
#25752=ORIENTED_EDGE('',*,*,#18791,.T.);
#25753=ORIENTED_EDGE('',*,*,#18792,.T.);
#25754=ORIENTED_EDGE('',*,*,#18778,.T.);
#25755=ORIENTED_EDGE('',*,*,#18787,.T.);
#25756=ORIENTED_EDGE('',*,*,#18784,.T.);
#25757=ORIENTED_EDGE('',*,*,#18781,.T.);
#25758=ORIENTED_EDGE('',*,*,#18793,.F.);
#25759=ORIENTED_EDGE('',*,*,#18794,.F.);
#25760=ORIENTED_EDGE('',*,*,#18795,.F.);
#25761=ORIENTED_EDGE('',*,*,#18790,.F.);
#25762=ORIENTED_EDGE('',*,*,#18732,.T.);
#25763=ORIENTED_EDGE('',*,*,#18738,.T.);
#25764=ORIENTED_EDGE('',*,*,#18744,.T.);
#25765=ORIENTED_EDGE('',*,*,#18750,.T.);
#25766=ORIENTED_EDGE('',*,*,#18756,.T.);
#25767=ORIENTED_EDGE('',*,*,#18762,.T.);
#25768=ORIENTED_EDGE('',*,*,#18768,.T.);
#25769=ORIENTED_EDGE('',*,*,#18774,.T.);
#25770=ORIENTED_EDGE('',*,*,#18795,.T.);
#25771=ORIENTED_EDGE('',*,*,#18796,.F.);
#25772=ORIENTED_EDGE('',*,*,#18797,.F.);
#25773=ORIENTED_EDGE('',*,*,#18791,.F.);
#25774=ORIENTED_EDGE('',*,*,#18797,.T.);
#25775=ORIENTED_EDGE('',*,*,#18798,.F.);
#25776=ORIENTED_EDGE('',*,*,#18799,.F.);
#25777=ORIENTED_EDGE('',*,*,#18792,.F.);
#25778=ORIENTED_EDGE('',*,*,#18731,.T.);
#25779=ORIENTED_EDGE('',*,*,#18737,.T.);
#25780=ORIENTED_EDGE('',*,*,#18743,.T.);
#25781=ORIENTED_EDGE('',*,*,#18749,.T.);
#25782=ORIENTED_EDGE('',*,*,#18755,.T.);
#25783=ORIENTED_EDGE('',*,*,#18761,.T.);
#25784=ORIENTED_EDGE('',*,*,#18767,.T.);
#25785=ORIENTED_EDGE('',*,*,#18773,.T.);
#25786=ORIENTED_EDGE('',*,*,#18799,.T.);
#25787=ORIENTED_EDGE('',*,*,#18800,.F.);
#25788=ORIENTED_EDGE('',*,*,#18793,.T.);
#25789=ORIENTED_EDGE('',*,*,#18789,.F.);
#25790=ORIENTED_EDGE('',*,*,#18800,.T.);
#25791=ORIENTED_EDGE('',*,*,#18798,.T.);
#25792=ORIENTED_EDGE('',*,*,#18796,.T.);
#25793=ORIENTED_EDGE('',*,*,#18794,.T.);
#25794=ORIENTED_EDGE('',*,*,#18780,.T.);
#25795=ORIENTED_EDGE('',*,*,#18783,.T.);
#25796=ORIENTED_EDGE('',*,*,#18786,.T.);
#25797=ORIENTED_EDGE('',*,*,#18788,.T.);
#25798=ORIENTED_EDGE('',*,*,#18801,.F.);
#25799=ORIENTED_EDGE('',*,*,#18802,.F.);
#25800=ORIENTED_EDGE('',*,*,#18803,.F.);
#25801=ORIENTED_EDGE('',*,*,#18804,.F.);
#25802=ORIENTED_EDGE('',*,*,#18805,.F.);
#25803=ORIENTED_EDGE('',*,*,#18806,.F.);
#25804=ORIENTED_EDGE('',*,*,#18807,.F.);
#25805=ORIENTED_EDGE('',*,*,#18808,.F.);
#25806=ORIENTED_EDGE('',*,*,#18809,.F.);
#25807=ORIENTED_EDGE('',*,*,#18810,.F.);
#25808=ORIENTED_EDGE('',*,*,#18811,.F.);
#25809=ORIENTED_EDGE('',*,*,#18812,.F.);
#25810=ORIENTED_EDGE('',*,*,#18813,.F.);
#25811=ORIENTED_EDGE('',*,*,#18814,.F.);
#25812=ORIENTED_EDGE('',*,*,#18802,.T.);
#25813=ORIENTED_EDGE('',*,*,#18815,.F.);
#25814=ORIENTED_EDGE('',*,*,#18811,.T.);
#25815=ORIENTED_EDGE('',*,*,#18816,.F.);
#25816=ORIENTED_EDGE('',*,*,#18817,.T.);
#25817=ORIENTED_EDGE('',*,*,#18818,.F.);
#25818=ORIENTED_EDGE('',*,*,#18817,.F.);
#25819=ORIENTED_EDGE('',*,*,#18812,.T.);
#25820=ORIENTED_EDGE('',*,*,#18819,.T.);
#25821=ORIENTED_EDGE('',*,*,#18818,.T.);
#25822=ORIENTED_EDGE('',*,*,#18819,.F.);
#25823=ORIENTED_EDGE('',*,*,#18820,.T.);
#25824=ORIENTED_EDGE('',*,*,#18821,.F.);
#25825=ORIENTED_EDGE('',*,*,#18820,.F.);
#25826=ORIENTED_EDGE('',*,*,#18813,.T.);
#25827=ORIENTED_EDGE('',*,*,#18822,.T.);
#25828=ORIENTED_EDGE('',*,*,#18821,.T.);
#25829=ORIENTED_EDGE('',*,*,#18822,.F.);
#25830=ORIENTED_EDGE('',*,*,#18823,.T.);
#25831=ORIENTED_EDGE('',*,*,#18824,.F.);
#25832=ORIENTED_EDGE('',*,*,#18823,.F.);
#25833=ORIENTED_EDGE('',*,*,#18814,.T.);
#25834=ORIENTED_EDGE('',*,*,#18825,.T.);
#25835=ORIENTED_EDGE('',*,*,#18824,.T.);
#25836=ORIENTED_EDGE('',*,*,#18825,.F.);
#25837=ORIENTED_EDGE('',*,*,#18826,.T.);
#25838=ORIENTED_EDGE('',*,*,#18827,.T.);
#25839=ORIENTED_EDGE('',*,*,#18826,.F.);
#25840=ORIENTED_EDGE('',*,*,#18827,.F.);
#25841=ORIENTED_EDGE('',*,*,#18828,.T.);
#25842=ORIENTED_EDGE('',*,*,#18805,.T.);
#25843=ORIENTED_EDGE('',*,*,#18828,.F.);
#25844=ORIENTED_EDGE('',*,*,#18829,.T.);
#25845=ORIENTED_EDGE('',*,*,#18830,.T.);
#25846=ORIENTED_EDGE('',*,*,#18829,.F.);
#25847=ORIENTED_EDGE('',*,*,#18830,.F.);
#25848=ORIENTED_EDGE('',*,*,#18831,.T.);
#25849=ORIENTED_EDGE('',*,*,#18806,.T.);
#25850=ORIENTED_EDGE('',*,*,#18831,.F.);
#25851=ORIENTED_EDGE('',*,*,#18832,.T.);
#25852=ORIENTED_EDGE('',*,*,#18833,.T.);
#25853=ORIENTED_EDGE('',*,*,#18832,.F.);
#25854=ORIENTED_EDGE('',*,*,#18833,.F.);
#25855=ORIENTED_EDGE('',*,*,#18834,.T.);
#25856=ORIENTED_EDGE('',*,*,#18807,.T.);
#25857=ORIENTED_EDGE('',*,*,#18834,.F.);
#25858=ORIENTED_EDGE('',*,*,#18835,.F.);
#25859=ORIENTED_EDGE('',*,*,#18836,.T.);
#25860=ORIENTED_EDGE('',*,*,#18837,.F.);
#25861=ORIENTED_EDGE('',*,*,#18836,.F.);
#25862=ORIENTED_EDGE('',*,*,#18838,.F.);
#25863=ORIENTED_EDGE('',*,*,#18839,.T.);
#25864=ORIENTED_EDGE('',*,*,#18840,.F.);
#25865=ORIENTED_EDGE('',*,*,#18839,.F.);
#25866=ORIENTED_EDGE('',*,*,#18841,.F.);
#25867=ORIENTED_EDGE('',*,*,#18842,.T.);
#25868=ORIENTED_EDGE('',*,*,#18843,.F.);
#25869=ORIENTED_EDGE('',*,*,#18842,.F.);
#25870=ORIENTED_EDGE('',*,*,#18844,.F.);
#25871=ORIENTED_EDGE('',*,*,#18845,.T.);
#25872=ORIENTED_EDGE('',*,*,#18846,.F.);
#25873=ORIENTED_EDGE('',*,*,#18845,.F.);
#25874=ORIENTED_EDGE('',*,*,#18847,.F.);
#25875=ORIENTED_EDGE('',*,*,#18848,.T.);
#25876=ORIENTED_EDGE('',*,*,#18849,.F.);
#25877=ORIENTED_EDGE('',*,*,#18848,.F.);
#25878=ORIENTED_EDGE('',*,*,#18850,.F.);
#25879=ORIENTED_EDGE('',*,*,#18851,.T.);
#25880=ORIENTED_EDGE('',*,*,#18852,.F.);
#25881=ORIENTED_EDGE('',*,*,#18851,.F.);
#25882=ORIENTED_EDGE('',*,*,#18853,.F.);
#25883=ORIENTED_EDGE('',*,*,#18854,.T.);
#25884=ORIENTED_EDGE('',*,*,#18855,.F.);
#25885=ORIENTED_EDGE('',*,*,#18854,.F.);
#25886=ORIENTED_EDGE('',*,*,#18856,.F.);
#25887=ORIENTED_EDGE('',*,*,#18857,.T.);
#25888=ORIENTED_EDGE('',*,*,#18858,.F.);
#25889=ORIENTED_EDGE('',*,*,#18857,.F.);
#25890=ORIENTED_EDGE('',*,*,#18859,.F.);
#25891=ORIENTED_EDGE('',*,*,#18860,.T.);
#25892=ORIENTED_EDGE('',*,*,#18861,.F.);
#25893=ORIENTED_EDGE('',*,*,#18860,.F.);
#25894=ORIENTED_EDGE('',*,*,#18862,.F.);
#25895=ORIENTED_EDGE('',*,*,#18863,.T.);
#25896=ORIENTED_EDGE('',*,*,#18864,.F.);
#25897=ORIENTED_EDGE('',*,*,#18863,.F.);
#25898=ORIENTED_EDGE('',*,*,#18801,.T.);
#25899=ORIENTED_EDGE('',*,*,#18865,.T.);
#25900=ORIENTED_EDGE('',*,*,#18808,.T.);
#25901=ORIENTED_EDGE('',*,*,#18815,.T.);
#25902=ORIENTED_EDGE('',*,*,#18837,.T.);
#25903=ORIENTED_EDGE('',*,*,#18840,.T.);
#25904=ORIENTED_EDGE('',*,*,#18843,.T.);
#25905=ORIENTED_EDGE('',*,*,#18846,.T.);
#25906=ORIENTED_EDGE('',*,*,#18849,.T.);
#25907=ORIENTED_EDGE('',*,*,#18852,.T.);
#25908=ORIENTED_EDGE('',*,*,#18855,.T.);
#25909=ORIENTED_EDGE('',*,*,#18858,.T.);
#25910=ORIENTED_EDGE('',*,*,#18859,.T.);
#25911=ORIENTED_EDGE('',*,*,#18862,.T.);
#25912=ORIENTED_EDGE('',*,*,#18804,.T.);
#25913=ORIENTED_EDGE('',*,*,#18866,.F.);
#25914=ORIENTED_EDGE('',*,*,#18809,.T.);
#25915=ORIENTED_EDGE('',*,*,#18865,.F.);
#25916=ORIENTED_EDGE('',*,*,#18803,.T.);
#25917=ORIENTED_EDGE('',*,*,#18816,.T.);
#25918=ORIENTED_EDGE('',*,*,#18810,.T.);
#25919=ORIENTED_EDGE('',*,*,#18866,.T.);
#25920=ORIENTED_EDGE('',*,*,#18835,.T.);
#25921=ORIENTED_EDGE('',*,*,#18838,.T.);
#25922=ORIENTED_EDGE('',*,*,#18841,.T.);
#25923=ORIENTED_EDGE('',*,*,#18844,.T.);
#25924=ORIENTED_EDGE('',*,*,#18847,.T.);
#25925=ORIENTED_EDGE('',*,*,#18850,.T.);
#25926=ORIENTED_EDGE('',*,*,#18853,.T.);
#25927=ORIENTED_EDGE('',*,*,#18856,.T.);
#25928=ORIENTED_EDGE('',*,*,#18861,.T.);
#25929=ORIENTED_EDGE('',*,*,#18864,.T.);
#25930=ORIENTED_EDGE('',*,*,#18867,.F.);
#25931=ORIENTED_EDGE('',*,*,#18868,.F.);
#25932=ORIENTED_EDGE('',*,*,#18869,.F.);
#25933=ORIENTED_EDGE('',*,*,#18870,.F.);
#25934=ORIENTED_EDGE('',*,*,#18871,.F.);
#25935=ORIENTED_EDGE('',*,*,#18872,.F.);
#25936=ORIENTED_EDGE('',*,*,#18873,.F.);
#25937=ORIENTED_EDGE('',*,*,#18874,.F.);
#25938=ORIENTED_EDGE('',*,*,#18875,.F.);
#25939=ORIENTED_EDGE('',*,*,#18876,.F.);
#25940=ORIENTED_EDGE('',*,*,#18877,.F.);
#25941=ORIENTED_EDGE('',*,*,#18878,.F.);
#25942=ORIENTED_EDGE('',*,*,#18879,.F.);
#25943=ORIENTED_EDGE('',*,*,#18880,.F.);
#25944=ORIENTED_EDGE('',*,*,#18868,.T.);
#25945=ORIENTED_EDGE('',*,*,#18881,.F.);
#25946=ORIENTED_EDGE('',*,*,#18877,.T.);
#25947=ORIENTED_EDGE('',*,*,#18882,.F.);
#25948=ORIENTED_EDGE('',*,*,#18883,.T.);
#25949=ORIENTED_EDGE('',*,*,#18884,.F.);
#25950=ORIENTED_EDGE('',*,*,#18883,.F.);
#25951=ORIENTED_EDGE('',*,*,#18871,.T.);
#25952=ORIENTED_EDGE('',*,*,#18885,.T.);
#25953=ORIENTED_EDGE('',*,*,#18884,.T.);
#25954=ORIENTED_EDGE('',*,*,#18885,.F.);
#25955=ORIENTED_EDGE('',*,*,#18886,.T.);
#25956=ORIENTED_EDGE('',*,*,#18887,.F.);
#25957=ORIENTED_EDGE('',*,*,#18886,.F.);
#25958=ORIENTED_EDGE('',*,*,#18872,.T.);
#25959=ORIENTED_EDGE('',*,*,#18888,.T.);
#25960=ORIENTED_EDGE('',*,*,#18887,.T.);
#25961=ORIENTED_EDGE('',*,*,#18888,.F.);
#25962=ORIENTED_EDGE('',*,*,#18889,.T.);
#25963=ORIENTED_EDGE('',*,*,#18890,.F.);
#25964=ORIENTED_EDGE('',*,*,#18889,.F.);
#25965=ORIENTED_EDGE('',*,*,#18873,.T.);
#25966=ORIENTED_EDGE('',*,*,#18891,.T.);
#25967=ORIENTED_EDGE('',*,*,#18890,.T.);
#25968=ORIENTED_EDGE('',*,*,#18891,.F.);
#25969=ORIENTED_EDGE('',*,*,#18892,.T.);
#25970=ORIENTED_EDGE('',*,*,#18893,.T.);
#25971=ORIENTED_EDGE('',*,*,#18892,.F.);
#25972=ORIENTED_EDGE('',*,*,#18893,.F.);
#25973=ORIENTED_EDGE('',*,*,#18894,.T.);
#25974=ORIENTED_EDGE('',*,*,#18880,.T.);
#25975=ORIENTED_EDGE('',*,*,#18894,.F.);
#25976=ORIENTED_EDGE('',*,*,#18895,.T.);
#25977=ORIENTED_EDGE('',*,*,#18896,.T.);
#25978=ORIENTED_EDGE('',*,*,#18895,.F.);
#25979=ORIENTED_EDGE('',*,*,#18896,.F.);
#25980=ORIENTED_EDGE('',*,*,#18897,.T.);
#25981=ORIENTED_EDGE('',*,*,#18879,.T.);
#25982=ORIENTED_EDGE('',*,*,#18897,.F.);
#25983=ORIENTED_EDGE('',*,*,#18898,.T.);
#25984=ORIENTED_EDGE('',*,*,#18899,.T.);
#25985=ORIENTED_EDGE('',*,*,#18898,.F.);
#25986=ORIENTED_EDGE('',*,*,#18899,.F.);
#25987=ORIENTED_EDGE('',*,*,#18900,.T.);
#25988=ORIENTED_EDGE('',*,*,#18878,.T.);
#25989=ORIENTED_EDGE('',*,*,#18900,.F.);
#25990=ORIENTED_EDGE('',*,*,#18901,.F.);
#25991=ORIENTED_EDGE('',*,*,#18902,.T.);
#25992=ORIENTED_EDGE('',*,*,#18903,.F.);
#25993=ORIENTED_EDGE('',*,*,#18902,.F.);
#25994=ORIENTED_EDGE('',*,*,#18904,.F.);
#25995=ORIENTED_EDGE('',*,*,#18905,.T.);
#25996=ORIENTED_EDGE('',*,*,#18906,.F.);
#25997=ORIENTED_EDGE('',*,*,#18905,.F.);
#25998=ORIENTED_EDGE('',*,*,#18907,.F.);
#25999=ORIENTED_EDGE('',*,*,#18908,.T.);
#26000=ORIENTED_EDGE('',*,*,#18909,.F.);
#26001=ORIENTED_EDGE('',*,*,#18908,.F.);
#26002=ORIENTED_EDGE('',*,*,#18910,.F.);
#26003=ORIENTED_EDGE('',*,*,#18911,.T.);
#26004=ORIENTED_EDGE('',*,*,#18912,.F.);
#26005=ORIENTED_EDGE('',*,*,#18911,.F.);
#26006=ORIENTED_EDGE('',*,*,#18913,.F.);
#26007=ORIENTED_EDGE('',*,*,#18914,.T.);
#26008=ORIENTED_EDGE('',*,*,#18915,.F.);
#26009=ORIENTED_EDGE('',*,*,#18914,.F.);
#26010=ORIENTED_EDGE('',*,*,#18916,.F.);
#26011=ORIENTED_EDGE('',*,*,#18917,.T.);
#26012=ORIENTED_EDGE('',*,*,#18918,.F.);
#26013=ORIENTED_EDGE('',*,*,#18917,.F.);
#26014=ORIENTED_EDGE('',*,*,#18919,.F.);
#26015=ORIENTED_EDGE('',*,*,#18920,.T.);
#26016=ORIENTED_EDGE('',*,*,#18921,.F.);
#26017=ORIENTED_EDGE('',*,*,#18920,.F.);
#26018=ORIENTED_EDGE('',*,*,#18922,.F.);
#26019=ORIENTED_EDGE('',*,*,#18923,.T.);
#26020=ORIENTED_EDGE('',*,*,#18924,.F.);
#26021=ORIENTED_EDGE('',*,*,#18923,.F.);
#26022=ORIENTED_EDGE('',*,*,#18925,.F.);
#26023=ORIENTED_EDGE('',*,*,#18926,.T.);
#26024=ORIENTED_EDGE('',*,*,#18927,.F.);
#26025=ORIENTED_EDGE('',*,*,#18926,.F.);
#26026=ORIENTED_EDGE('',*,*,#18928,.F.);
#26027=ORIENTED_EDGE('',*,*,#18929,.T.);
#26028=ORIENTED_EDGE('',*,*,#18930,.F.);
#26029=ORIENTED_EDGE('',*,*,#18929,.F.);
#26030=ORIENTED_EDGE('',*,*,#18867,.T.);
#26031=ORIENTED_EDGE('',*,*,#18931,.T.);
#26032=ORIENTED_EDGE('',*,*,#18874,.T.);
#26033=ORIENTED_EDGE('',*,*,#18881,.T.);
#26034=ORIENTED_EDGE('',*,*,#18903,.T.);
#26035=ORIENTED_EDGE('',*,*,#18906,.T.);
#26036=ORIENTED_EDGE('',*,*,#18909,.T.);
#26037=ORIENTED_EDGE('',*,*,#18912,.T.);
#26038=ORIENTED_EDGE('',*,*,#18915,.T.);
#26039=ORIENTED_EDGE('',*,*,#18918,.T.);
#26040=ORIENTED_EDGE('',*,*,#18921,.T.);
#26041=ORIENTED_EDGE('',*,*,#18924,.T.);
#26042=ORIENTED_EDGE('',*,*,#18925,.T.);
#26043=ORIENTED_EDGE('',*,*,#18928,.T.);
#26044=ORIENTED_EDGE('',*,*,#18870,.T.);
#26045=ORIENTED_EDGE('',*,*,#18932,.F.);
#26046=ORIENTED_EDGE('',*,*,#18875,.T.);
#26047=ORIENTED_EDGE('',*,*,#18931,.F.);
#26048=ORIENTED_EDGE('',*,*,#18869,.T.);
#26049=ORIENTED_EDGE('',*,*,#18882,.T.);
#26050=ORIENTED_EDGE('',*,*,#18876,.T.);
#26051=ORIENTED_EDGE('',*,*,#18932,.T.);
#26052=ORIENTED_EDGE('',*,*,#18901,.T.);
#26053=ORIENTED_EDGE('',*,*,#18904,.T.);
#26054=ORIENTED_EDGE('',*,*,#18907,.T.);
#26055=ORIENTED_EDGE('',*,*,#18910,.T.);
#26056=ORIENTED_EDGE('',*,*,#18913,.T.);
#26057=ORIENTED_EDGE('',*,*,#18916,.T.);
#26058=ORIENTED_EDGE('',*,*,#18919,.T.);
#26059=ORIENTED_EDGE('',*,*,#18922,.T.);
#26060=ORIENTED_EDGE('',*,*,#18927,.T.);
#26061=ORIENTED_EDGE('',*,*,#18930,.T.);
#26062=ORIENTED_EDGE('',*,*,#18933,.F.);
#26063=ORIENTED_EDGE('',*,*,#18934,.T.);
#26064=ORIENTED_EDGE('',*,*,#18935,.F.);
#26065=ORIENTED_EDGE('',*,*,#18934,.F.);
#26066=ORIENTED_EDGE('',*,*,#18936,.F.);
#26067=ORIENTED_EDGE('',*,*,#18937,.T.);
#26068=ORIENTED_EDGE('',*,*,#18938,.F.);
#26069=ORIENTED_EDGE('',*,*,#18937,.F.);
#26070=ORIENTED_EDGE('',*,*,#18939,.F.);
#26071=ORIENTED_EDGE('',*,*,#18940,.T.);
#26072=ORIENTED_EDGE('',*,*,#18941,.F.);
#26073=ORIENTED_EDGE('',*,*,#18940,.F.);
#26074=ORIENTED_EDGE('',*,*,#18942,.F.);
#26075=ORIENTED_EDGE('',*,*,#18943,.T.);
#26076=ORIENTED_EDGE('',*,*,#18944,.F.);
#26077=ORIENTED_EDGE('',*,*,#18943,.F.);
#26078=ORIENTED_EDGE('',*,*,#18945,.F.);
#26079=ORIENTED_EDGE('',*,*,#18946,.T.);
#26080=ORIENTED_EDGE('',*,*,#18947,.F.);
#26081=ORIENTED_EDGE('',*,*,#18946,.F.);
#26082=ORIENTED_EDGE('',*,*,#18948,.F.);
#26083=ORIENTED_EDGE('',*,*,#18949,.T.);
#26084=ORIENTED_EDGE('',*,*,#18950,.F.);
#26085=ORIENTED_EDGE('',*,*,#18949,.F.);
#26086=ORIENTED_EDGE('',*,*,#18951,.T.);
#26087=ORIENTED_EDGE('',*,*,#18952,.T.);
#26088=ORIENTED_EDGE('',*,*,#18953,.F.);
#26089=ORIENTED_EDGE('',*,*,#18954,.F.);
#26090=ORIENTED_EDGE('',*,*,#18955,.T.);
#26091=ORIENTED_EDGE('',*,*,#18954,.T.);
#26092=ORIENTED_EDGE('',*,*,#18956,.F.);
#26093=ORIENTED_EDGE('',*,*,#18957,.F.);
#26094=ORIENTED_EDGE('',*,*,#18958,.T.);
#26095=ORIENTED_EDGE('',*,*,#18957,.T.);
#26096=ORIENTED_EDGE('',*,*,#18959,.F.);
#26097=ORIENTED_EDGE('',*,*,#18960,.F.);
#26098=ORIENTED_EDGE('',*,*,#18961,.T.);
#26099=ORIENTED_EDGE('',*,*,#18960,.T.);
#26100=ORIENTED_EDGE('',*,*,#18962,.F.);
#26101=ORIENTED_EDGE('',*,*,#18952,.F.);
#26102=ORIENTED_EDGE('',*,*,#18962,.T.);
#26103=ORIENTED_EDGE('',*,*,#18959,.T.);
#26104=ORIENTED_EDGE('',*,*,#18956,.T.);
#26105=ORIENTED_EDGE('',*,*,#18953,.T.);
#26106=ORIENTED_EDGE('',*,*,#18935,.T.);
#26107=ORIENTED_EDGE('',*,*,#18938,.T.);
#26108=ORIENTED_EDGE('',*,*,#18941,.T.);
#26109=ORIENTED_EDGE('',*,*,#18944,.T.);
#26110=ORIENTED_EDGE('',*,*,#18947,.T.);
#26111=ORIENTED_EDGE('',*,*,#18950,.T.);
#26112=ORIENTED_EDGE('',*,*,#18961,.F.);
#26113=ORIENTED_EDGE('',*,*,#18951,.F.);
#26114=ORIENTED_EDGE('',*,*,#18955,.F.);
#26115=ORIENTED_EDGE('',*,*,#18958,.F.);
#26116=ORIENTED_EDGE('',*,*,#18933,.T.);
#26117=ORIENTED_EDGE('',*,*,#18936,.T.);
#26118=ORIENTED_EDGE('',*,*,#18939,.T.);
#26119=ORIENTED_EDGE('',*,*,#18942,.T.);
#26120=ORIENTED_EDGE('',*,*,#18945,.T.);
#26121=ORIENTED_EDGE('',*,*,#18948,.T.);
#26122=ORIENTED_EDGE('',*,*,#18963,.F.);
#26123=ORIENTED_EDGE('',*,*,#18964,.F.);
#26124=ORIENTED_EDGE('',*,*,#18965,.F.);
#26125=ORIENTED_EDGE('',*,*,#18966,.F.);
#26126=ORIENTED_EDGE('',*,*,#18966,.T.);
#26127=ORIENTED_EDGE('',*,*,#18967,.T.);
#26128=ORIENTED_EDGE('',*,*,#18968,.F.);
#26129=ORIENTED_EDGE('',*,*,#18969,.T.);
#26130=ORIENTED_EDGE('',*,*,#18965,.T.);
#26131=ORIENTED_EDGE('',*,*,#18970,.T.);
#26132=ORIENTED_EDGE('',*,*,#18971,.F.);
#26133=ORIENTED_EDGE('',*,*,#18972,.F.);
#26134=ORIENTED_EDGE('',*,*,#18973,.T.);
#26135=ORIENTED_EDGE('',*,*,#18974,.F.);
#26136=ORIENTED_EDGE('',*,*,#18975,.F.);
#26137=ORIENTED_EDGE('',*,*,#18967,.F.);
#26138=ORIENTED_EDGE('',*,*,#18976,.F.);
#26139=ORIENTED_EDGE('',*,*,#18973,.F.);
#26140=ORIENTED_EDGE('',*,*,#18977,.F.);
#26141=ORIENTED_EDGE('',*,*,#18978,.F.);
#26142=ORIENTED_EDGE('',*,*,#18963,.T.);
#26143=ORIENTED_EDGE('',*,*,#18969,.F.);
#26144=ORIENTED_EDGE('',*,*,#18979,.F.);
#26145=ORIENTED_EDGE('',*,*,#18980,.F.);
#26146=ORIENTED_EDGE('',*,*,#18978,.T.);
#26147=ORIENTED_EDGE('',*,*,#18981,.F.);
#26148=ORIENTED_EDGE('',*,*,#18982,.F.);
#26149=ORIENTED_EDGE('',*,*,#18983,.T.);
#26150=ORIENTED_EDGE('',*,*,#18977,.T.);
#26151=ORIENTED_EDGE('',*,*,#18972,.T.);
#26152=ORIENTED_EDGE('',*,*,#18984,.F.);
#26153=ORIENTED_EDGE('',*,*,#18981,.T.);
#26154=ORIENTED_EDGE('',*,*,#18976,.T.);
#26155=ORIENTED_EDGE('',*,*,#18980,.T.);
#26156=ORIENTED_EDGE('',*,*,#18985,.F.);
#26157=ORIENTED_EDGE('',*,*,#18974,.T.);
#26158=ORIENTED_EDGE('',*,*,#18982,.T.);
#26159=ORIENTED_EDGE('',*,*,#18984,.T.);
#26160=ORIENTED_EDGE('',*,*,#18971,.T.);
#26161=ORIENTED_EDGE('',*,*,#18986,.T.);
#26162=ORIENTED_EDGE('',*,*,#18975,.T.);
#26163=ORIENTED_EDGE('',*,*,#18985,.T.);
#26164=ORIENTED_EDGE('',*,*,#18979,.T.);
#26165=ORIENTED_EDGE('',*,*,#18968,.T.);
#26166=ORIENTED_EDGE('',*,*,#18964,.T.);
#26167=ORIENTED_EDGE('',*,*,#18983,.F.);
#26168=ORIENTED_EDGE('',*,*,#18986,.F.);
#26169=ORIENTED_EDGE('',*,*,#18970,.F.);
#26170=ORIENTED_EDGE('',*,*,#18987,.F.);
#26171=ORIENTED_EDGE('',*,*,#18988,.T.);
#26172=ORIENTED_EDGE('',*,*,#18989,.F.);
#26173=ORIENTED_EDGE('',*,*,#18988,.F.);
#26174=ORIENTED_EDGE('',*,*,#18990,.F.);
#26175=ORIENTED_EDGE('',*,*,#18991,.T.);
#26176=ORIENTED_EDGE('',*,*,#18992,.F.);
#26177=ORIENTED_EDGE('',*,*,#18991,.F.);
#26178=ORIENTED_EDGE('',*,*,#18993,.F.);
#26179=ORIENTED_EDGE('',*,*,#18994,.T.);
#26180=ORIENTED_EDGE('',*,*,#18995,.F.);
#26181=ORIENTED_EDGE('',*,*,#18994,.F.);
#26182=ORIENTED_EDGE('',*,*,#18996,.F.);
#26183=ORIENTED_EDGE('',*,*,#18997,.T.);
#26184=ORIENTED_EDGE('',*,*,#18998,.F.);
#26185=ORIENTED_EDGE('',*,*,#18997,.F.);
#26186=ORIENTED_EDGE('',*,*,#18999,.F.);
#26187=ORIENTED_EDGE('',*,*,#19000,.T.);
#26188=ORIENTED_EDGE('',*,*,#19001,.F.);
#26189=ORIENTED_EDGE('',*,*,#19002,.F.);
#26190=ORIENTED_EDGE('',*,*,#19003,.F.);
#26191=ORIENTED_EDGE('',*,*,#19004,.T.);
#26192=ORIENTED_EDGE('',*,*,#19005,.F.);
#26193=ORIENTED_EDGE('',*,*,#19000,.F.);
#26194=ORIENTED_EDGE('',*,*,#19006,.F.);
#26195=ORIENTED_EDGE('',*,*,#19007,.T.);
#26196=ORIENTED_EDGE('',*,*,#19008,.F.);
#26197=ORIENTED_EDGE('',*,*,#19004,.F.);
#26198=ORIENTED_EDGE('',*,*,#19009,.F.);
#26199=ORIENTED_EDGE('',*,*,#19002,.T.);
#26200=ORIENTED_EDGE('',*,*,#19010,.F.);
#26201=ORIENTED_EDGE('',*,*,#19007,.F.);
#26202=ORIENTED_EDGE('',*,*,#19011,.T.);
#26203=ORIENTED_EDGE('',*,*,#19012,.T.);
#26204=ORIENTED_EDGE('',*,*,#19013,.F.);
#26205=ORIENTED_EDGE('',*,*,#19014,.F.);
#26206=ORIENTED_EDGE('',*,*,#19015,.T.);
#26207=ORIENTED_EDGE('',*,*,#19014,.T.);
#26208=ORIENTED_EDGE('',*,*,#19016,.F.);
#26209=ORIENTED_EDGE('',*,*,#19017,.F.);
#26210=ORIENTED_EDGE('',*,*,#19018,.T.);
#26211=ORIENTED_EDGE('',*,*,#19017,.T.);
#26212=ORIENTED_EDGE('',*,*,#19019,.F.);
#26213=ORIENTED_EDGE('',*,*,#19020,.F.);
#26214=ORIENTED_EDGE('',*,*,#19021,.T.);
#26215=ORIENTED_EDGE('',*,*,#19020,.T.);
#26216=ORIENTED_EDGE('',*,*,#19022,.F.);
#26217=ORIENTED_EDGE('',*,*,#19012,.F.);
#26218=ORIENTED_EDGE('',*,*,#19022,.T.);
#26219=ORIENTED_EDGE('',*,*,#19019,.T.);
#26220=ORIENTED_EDGE('',*,*,#19016,.T.);
#26221=ORIENTED_EDGE('',*,*,#19013,.T.);
#26222=ORIENTED_EDGE('',*,*,#18987,.T.);
#26223=ORIENTED_EDGE('',*,*,#18990,.T.);
#26224=ORIENTED_EDGE('',*,*,#18993,.T.);
#26225=ORIENTED_EDGE('',*,*,#18996,.T.);
#26226=ORIENTED_EDGE('',*,*,#19001,.T.);
#26227=ORIENTED_EDGE('',*,*,#19005,.T.);
#26228=ORIENTED_EDGE('',*,*,#19008,.T.);
#26229=ORIENTED_EDGE('',*,*,#19010,.T.);
#26230=ORIENTED_EDGE('',*,*,#19021,.F.);
#26231=ORIENTED_EDGE('',*,*,#19011,.F.);
#26232=ORIENTED_EDGE('',*,*,#19015,.F.);
#26233=ORIENTED_EDGE('',*,*,#19018,.F.);
#26234=ORIENTED_EDGE('',*,*,#18989,.T.);
#26235=ORIENTED_EDGE('',*,*,#18992,.T.);
#26236=ORIENTED_EDGE('',*,*,#18995,.T.);
#26237=ORIENTED_EDGE('',*,*,#18998,.T.);
#26238=ORIENTED_EDGE('',*,*,#18999,.T.);
#26239=ORIENTED_EDGE('',*,*,#19009,.T.);
#26240=ORIENTED_EDGE('',*,*,#19006,.T.);
#26241=ORIENTED_EDGE('',*,*,#19003,.T.);
#26242=ORIENTED_EDGE('',*,*,#19023,.F.);
#26243=ORIENTED_EDGE('',*,*,#19024,.F.);
#26244=ORIENTED_EDGE('',*,*,#19025,.T.);
#26245=ORIENTED_EDGE('',*,*,#19026,.T.);
#26246=ORIENTED_EDGE('',*,*,#19027,.T.);
#26247=ORIENTED_EDGE('',*,*,#19028,.T.);
#26248=ORIENTED_EDGE('',*,*,#19029,.F.);
#26249=ORIENTED_EDGE('',*,*,#19030,.T.);
#26250=ORIENTED_EDGE('',*,*,#19031,.T.);
#26251=ORIENTED_EDGE('',*,*,#19032,.F.);
#26252=ORIENTED_EDGE('',*,*,#19033,.F.);
#26253=ORIENTED_EDGE('',*,*,#19032,.T.);
#26254=ORIENTED_EDGE('',*,*,#19034,.T.);
#26255=ORIENTED_EDGE('',*,*,#19035,.F.);
#26256=ORIENTED_EDGE('',*,*,#19036,.F.);
#26257=ORIENTED_EDGE('',*,*,#19037,.T.);
#26258=ORIENTED_EDGE('',*,*,#19038,.T.);
#26259=ORIENTED_EDGE('',*,*,#19030,.F.);
#26260=ORIENTED_EDGE('',*,*,#19039,.F.);
#26261=ORIENTED_EDGE('',*,*,#19035,.T.);
#26262=ORIENTED_EDGE('',*,*,#19040,.T.);
#26263=ORIENTED_EDGE('',*,*,#19037,.F.);
#26264=ORIENTED_EDGE('',*,*,#19034,.F.);
#26265=ORIENTED_EDGE('',*,*,#19031,.F.);
#26266=ORIENTED_EDGE('',*,*,#19038,.F.);
#26267=ORIENTED_EDGE('',*,*,#19040,.F.);
#26268=ORIENTED_EDGE('',*,*,#19041,.T.);
#26269=ORIENTED_EDGE('',*,*,#19042,.T.);
#26270=ORIENTED_EDGE('',*,*,#19043,.T.);
#26271=ORIENTED_EDGE('',*,*,#19044,.T.);
#26272=ORIENTED_EDGE('',*,*,#19043,.F.);
#26273=ORIENTED_EDGE('',*,*,#19045,.F.);
#26274=ORIENTED_EDGE('',*,*,#19044,.F.);
#26275=ORIENTED_EDGE('',*,*,#19046,.F.);
#26276=ORIENTED_EDGE('',*,*,#19047,.T.);
#26277=ORIENTED_EDGE('',*,*,#19041,.F.);
#26278=ORIENTED_EDGE('',*,*,#19042,.F.);
#26279=ORIENTED_EDGE('',*,*,#19047,.F.);
#26280=ORIENTED_EDGE('',*,*,#19039,.T.);
#26281=ORIENTED_EDGE('',*,*,#19036,.T.);
#26282=ORIENTED_EDGE('',*,*,#19029,.T.);
#26283=ORIENTED_EDGE('',*,*,#19033,.T.);
#26284=ORIENTED_EDGE('',*,*,#19048,.T.);
#26285=ORIENTED_EDGE('',*,*,#19049,.T.);
#26286=ORIENTED_EDGE('',*,*,#19050,.T.);
#26287=ORIENTED_EDGE('',*,*,#19051,.T.);
#26288=ORIENTED_EDGE('',*,*,#19049,.F.);
#26289=ORIENTED_EDGE('',*,*,#19052,.F.);
#26290=ORIENTED_EDGE('',*,*,#19048,.F.);
#26291=ORIENTED_EDGE('',*,*,#19051,.F.);
#26292=ORIENTED_EDGE('',*,*,#19053,.T.);
#26293=ORIENTED_EDGE('',*,*,#19054,.F.);
#26294=ORIENTED_EDGE('',*,*,#19055,.F.);
#26295=ORIENTED_EDGE('',*,*,#19053,.F.);
#26296=ORIENTED_EDGE('',*,*,#19050,.F.);
#26297=ORIENTED_EDGE('',*,*,#19056,.T.);
#26298=ORIENTED_EDGE('',*,*,#19057,.T.);
#26299=ORIENTED_EDGE('',*,*,#19058,.T.);
#26300=ORIENTED_EDGE('',*,*,#19052,.T.);
#26301=ORIENTED_EDGE('',*,*,#19058,.F.);
#26302=ORIENTED_EDGE('',*,*,#19059,.F.);
#26303=ORIENTED_EDGE('',*,*,#19060,.T.);
#26304=ORIENTED_EDGE('',*,*,#19056,.F.);
#26305=ORIENTED_EDGE('',*,*,#19057,.F.);
#26306=ORIENTED_EDGE('',*,*,#19060,.F.);
#26307=ORIENTED_EDGE('',*,*,#19061,.F.);
#26308=ORIENTED_EDGE('',*,*,#19062,.T.);
#26309=ORIENTED_EDGE('',*,*,#19063,.T.);
#26310=ORIENTED_EDGE('',*,*,#19064,.T.);
#26311=ORIENTED_EDGE('',*,*,#19045,.T.);
#26312=ORIENTED_EDGE('',*,*,#19064,.F.);
#26313=ORIENTED_EDGE('',*,*,#19062,.F.);
#26314=ORIENTED_EDGE('',*,*,#19063,.F.);
#26315=ORIENTED_EDGE('',*,*,#19065,.T.);
#26316=ORIENTED_EDGE('',*,*,#19066,.T.);
#26317=ORIENTED_EDGE('',*,*,#19067,.T.);
#26318=ORIENTED_EDGE('',*,*,#19065,.F.);
#26319=ORIENTED_EDGE('',*,*,#19054,.T.);
#26320=ORIENTED_EDGE('',*,*,#19055,.T.);
#26321=ORIENTED_EDGE('',*,*,#19068,.T.);
#26322=ORIENTED_EDGE('',*,*,#19069,.T.);
#26323=ORIENTED_EDGE('',*,*,#19068,.F.);
#26324=ORIENTED_EDGE('',*,*,#19069,.F.);
#26325=ORIENTED_EDGE('',*,*,#19027,.F.);
#26326=ORIENTED_EDGE('',*,*,#19070,.T.);
#26327=ORIENTED_EDGE('',*,*,#19071,.T.);
#26328=ORIENTED_EDGE('',*,*,#19072,.F.);
#26329=ORIENTED_EDGE('',*,*,#19073,.F.);
#26330=ORIENTED_EDGE('',*,*,#19074,.F.);
#26331=ORIENTED_EDGE('',*,*,#19072,.T.);
#26332=ORIENTED_EDGE('',*,*,#19075,.T.);
#26333=ORIENTED_EDGE('',*,*,#19076,.F.);
#26334=ORIENTED_EDGE('',*,*,#19026,.F.);
#26335=ORIENTED_EDGE('',*,*,#19077,.T.);
#26336=ORIENTED_EDGE('',*,*,#19078,.T.);
#26337=ORIENTED_EDGE('',*,*,#19070,.F.);
#26338=ORIENTED_EDGE('',*,*,#19025,.F.);
#26339=ORIENTED_EDGE('',*,*,#19079,.F.);
#26340=ORIENTED_EDGE('',*,*,#19076,.T.);
#26341=ORIENTED_EDGE('',*,*,#19080,.T.);
#26342=ORIENTED_EDGE('',*,*,#19077,.F.);
#26343=ORIENTED_EDGE('',*,*,#19071,.F.);
#26344=ORIENTED_EDGE('',*,*,#19078,.F.);
#26345=ORIENTED_EDGE('',*,*,#19080,.F.);
#26346=ORIENTED_EDGE('',*,*,#19075,.F.);
#26347=ORIENTED_EDGE('',*,*,#19023,.T.);
#26348=ORIENTED_EDGE('',*,*,#19081,.T.);
#26349=ORIENTED_EDGE('',*,*,#19073,.T.);
#26350=ORIENTED_EDGE('',*,*,#19074,.T.);
#26351=ORIENTED_EDGE('',*,*,#19079,.T.);
#26352=ORIENTED_EDGE('',*,*,#19082,.F.);
#26353=ORIENTED_EDGE('',*,*,#19046,.T.);
#26354=ORIENTED_EDGE('',*,*,#19083,.T.);
#26355=ORIENTED_EDGE('',*,*,#19084,.F.);
#26356=ORIENTED_EDGE('',*,*,#19083,.F.);
#26357=ORIENTED_EDGE('',*,*,#19084,.T.);
#26358=ORIENTED_EDGE('',*,*,#19085,.F.);
#26359=ORIENTED_EDGE('',*,*,#19086,.T.);
#26360=ORIENTED_EDGE('',*,*,#19061,.T.);
#26361=ORIENTED_EDGE('',*,*,#19059,.T.);
#26362=ORIENTED_EDGE('',*,*,#19086,.F.);
#26363=ORIENTED_EDGE('',*,*,#19087,.F.);
#26364=ORIENTED_EDGE('',*,*,#19085,.T.);
#26365=ORIENTED_EDGE('',*,*,#19028,.F.);
#26366=ORIENTED_EDGE('',*,*,#19081,.F.);
#26367=ORIENTED_EDGE('',*,*,#19088,.T.);
#26368=ORIENTED_EDGE('',*,*,#19087,.T.);
#26369=ORIENTED_EDGE('',*,*,#19088,.F.);
#26370=ORIENTED_EDGE('',*,*,#19024,.T.);
#26371=ORIENTED_EDGE('',*,*,#19089,.T.);
#26372=ORIENTED_EDGE('',*,*,#19090,.F.);
#26373=ORIENTED_EDGE('',*,*,#19089,.F.);
#26374=ORIENTED_EDGE('',*,*,#19082,.T.);
#26375=ORIENTED_EDGE('',*,*,#19090,.T.);
#26376=ORIENTED_EDGE('',*,*,#19091,.F.);
#26377=ORIENTED_EDGE('',*,*,#19066,.F.);
#26378=ORIENTED_EDGE('',*,*,#19067,.F.);
#26379=ORIENTED_EDGE('',*,*,#19092,.T.);
#26380=ORIENTED_EDGE('',*,*,#19091,.T.);
#26381=ORIENTED_EDGE('',*,*,#19092,.F.);
#26382=ORIENTED_EDGE('',*,*,#19093,.F.);
#26383=ORIENTED_EDGE('',*,*,#19094,.F.);
#26384=ORIENTED_EDGE('',*,*,#19095,.T.);
#26385=ORIENTED_EDGE('',*,*,#19096,.T.);
#26386=ORIENTED_EDGE('',*,*,#19097,.T.);
#26387=ORIENTED_EDGE('',*,*,#19098,.T.);
#26388=ORIENTED_EDGE('',*,*,#19099,.T.);
#26389=ORIENTED_EDGE('',*,*,#19100,.T.);
#26390=ORIENTED_EDGE('',*,*,#19101,.T.);
#26391=ORIENTED_EDGE('',*,*,#19102,.T.);
#26392=ORIENTED_EDGE('',*,*,#19101,.F.);
#26393=ORIENTED_EDGE('',*,*,#19099,.F.);
#26394=ORIENTED_EDGE('',*,*,#19100,.F.);
#26395=ORIENTED_EDGE('',*,*,#19103,.T.);
#26396=ORIENTED_EDGE('',*,*,#19104,.T.);
#26397=ORIENTED_EDGE('',*,*,#19103,.F.);
#26398=ORIENTED_EDGE('',*,*,#19105,.T.);
#26399=ORIENTED_EDGE('',*,*,#19106,.T.);
#26400=ORIENTED_EDGE('',*,*,#19107,.T.);
#26401=ORIENTED_EDGE('',*,*,#19108,.T.);
#26402=ORIENTED_EDGE('',*,*,#19102,.F.);
#26403=ORIENTED_EDGE('',*,*,#19109,.T.);
#26404=ORIENTED_EDGE('',*,*,#19110,.T.);
#26405=ORIENTED_EDGE('',*,*,#19111,.T.);
#26406=ORIENTED_EDGE('',*,*,#19112,.T.);
#26407=ORIENTED_EDGE('',*,*,#19111,.F.);
#26408=ORIENTED_EDGE('',*,*,#19109,.F.);
#26409=ORIENTED_EDGE('',*,*,#19110,.F.);
#26410=ORIENTED_EDGE('',*,*,#19113,.T.);
#26411=ORIENTED_EDGE('',*,*,#19114,.F.);
#26412=ORIENTED_EDGE('',*,*,#19115,.F.);
#26413=ORIENTED_EDGE('',*,*,#19113,.F.);
#26414=ORIENTED_EDGE('',*,*,#19112,.F.);
#26415=ORIENTED_EDGE('',*,*,#19104,.F.);
#26416=ORIENTED_EDGE('',*,*,#19107,.F.);
#26417=ORIENTED_EDGE('',*,*,#19116,.T.);
#26418=ORIENTED_EDGE('',*,*,#19117,.T.);
#26419=ORIENTED_EDGE('',*,*,#19118,.F.);
#26420=ORIENTED_EDGE('',*,*,#19108,.F.);
#26421=ORIENTED_EDGE('',*,*,#19118,.T.);
#26422=ORIENTED_EDGE('',*,*,#19119,.T.);
#26423=ORIENTED_EDGE('',*,*,#19120,.F.);
#26424=ORIENTED_EDGE('',*,*,#19105,.F.);
#26425=ORIENTED_EDGE('',*,*,#19120,.T.);
#26426=ORIENTED_EDGE('',*,*,#19121,.T.);
#26427=ORIENTED_EDGE('',*,*,#19122,.F.);
#26428=ORIENTED_EDGE('',*,*,#19106,.F.);
#26429=ORIENTED_EDGE('',*,*,#19122,.T.);
#26430=ORIENTED_EDGE('',*,*,#19123,.T.);
#26431=ORIENTED_EDGE('',*,*,#19116,.F.);
#26432=ORIENTED_EDGE('',*,*,#19123,.F.);
#26433=ORIENTED_EDGE('',*,*,#19121,.F.);
#26434=ORIENTED_EDGE('',*,*,#19119,.F.);
#26435=ORIENTED_EDGE('',*,*,#19117,.F.);
#26436=ORIENTED_EDGE('',*,*,#19124,.T.);
#26437=ORIENTED_EDGE('',*,*,#19125,.T.);
#26438=ORIENTED_EDGE('',*,*,#19126,.T.);
#26439=ORIENTED_EDGE('',*,*,#19127,.T.);
#26440=ORIENTED_EDGE('',*,*,#19126,.F.);
#26441=ORIENTED_EDGE('',*,*,#19127,.F.);
#26442=ORIENTED_EDGE('',*,*,#19128,.F.);
#26443=ORIENTED_EDGE('',*,*,#19129,.F.);
#26444=ORIENTED_EDGE('',*,*,#19130,.T.);
#26445=ORIENTED_EDGE('',*,*,#19124,.F.);
#26446=ORIENTED_EDGE('',*,*,#19125,.F.);
#26447=ORIENTED_EDGE('',*,*,#19130,.F.);
#26448=ORIENTED_EDGE('',*,*,#19131,.F.);
#26449=ORIENTED_EDGE('',*,*,#19128,.T.);
#26450=ORIENTED_EDGE('',*,*,#19132,.T.);
#26451=ORIENTED_EDGE('',*,*,#19133,.T.);
#26452=ORIENTED_EDGE('',*,*,#19134,.T.);
#26453=ORIENTED_EDGE('',*,*,#19132,.F.);
#26454=ORIENTED_EDGE('',*,*,#19134,.F.);
#26455=ORIENTED_EDGE('',*,*,#19135,.T.);
#26456=ORIENTED_EDGE('',*,*,#19136,.F.);
#26457=ORIENTED_EDGE('',*,*,#19137,.F.);
#26458=ORIENTED_EDGE('',*,*,#19135,.F.);
#26459=ORIENTED_EDGE('',*,*,#19133,.F.);
#26460=ORIENTED_EDGE('',*,*,#19114,.T.);
#26461=ORIENTED_EDGE('',*,*,#19115,.T.);
#26462=ORIENTED_EDGE('',*,*,#19138,.T.);
#26463=ORIENTED_EDGE('',*,*,#19139,.T.);
#26464=ORIENTED_EDGE('',*,*,#19138,.F.);
#26465=ORIENTED_EDGE('',*,*,#19140,.F.);
#26466=ORIENTED_EDGE('',*,*,#19139,.F.);
#26467=ORIENTED_EDGE('',*,*,#19141,.T.);
#26468=ORIENTED_EDGE('',*,*,#19142,.T.);
#26469=ORIENTED_EDGE('',*,*,#19143,.T.);
#26470=ORIENTED_EDGE('',*,*,#19140,.T.);
#26471=ORIENTED_EDGE('',*,*,#19143,.F.);
#26472=ORIENTED_EDGE('',*,*,#19141,.F.);
#26473=ORIENTED_EDGE('',*,*,#19142,.F.);
#26474=ORIENTED_EDGE('',*,*,#19144,.T.);
#26475=ORIENTED_EDGE('',*,*,#19145,.T.);
#26476=ORIENTED_EDGE('',*,*,#19146,.T.);
#26477=ORIENTED_EDGE('',*,*,#19144,.F.);
#26478=ORIENTED_EDGE('',*,*,#19136,.T.);
#26479=ORIENTED_EDGE('',*,*,#19137,.T.);
#26480=ORIENTED_EDGE('',*,*,#19147,.T.);
#26481=ORIENTED_EDGE('',*,*,#19148,.T.);
#26482=ORIENTED_EDGE('',*,*,#19147,.F.);
#26483=ORIENTED_EDGE('',*,*,#19148,.F.);
#26484=ORIENTED_EDGE('',*,*,#19097,.F.);
#26485=ORIENTED_EDGE('',*,*,#19149,.T.);
#26486=ORIENTED_EDGE('',*,*,#19150,.T.);
#26487=ORIENTED_EDGE('',*,*,#19151,.F.);
#26488=ORIENTED_EDGE('',*,*,#19152,.F.);
#26489=ORIENTED_EDGE('',*,*,#19153,.F.);
#26490=ORIENTED_EDGE('',*,*,#19151,.T.);
#26491=ORIENTED_EDGE('',*,*,#19154,.T.);
#26492=ORIENTED_EDGE('',*,*,#19155,.F.);
#26493=ORIENTED_EDGE('',*,*,#19096,.F.);
#26494=ORIENTED_EDGE('',*,*,#19156,.T.);
#26495=ORIENTED_EDGE('',*,*,#19157,.T.);
#26496=ORIENTED_EDGE('',*,*,#19149,.F.);
#26497=ORIENTED_EDGE('',*,*,#19095,.F.);
#26498=ORIENTED_EDGE('',*,*,#19158,.F.);
#26499=ORIENTED_EDGE('',*,*,#19155,.T.);
#26500=ORIENTED_EDGE('',*,*,#19159,.T.);
#26501=ORIENTED_EDGE('',*,*,#19156,.F.);
#26502=ORIENTED_EDGE('',*,*,#19150,.F.);
#26503=ORIENTED_EDGE('',*,*,#19157,.F.);
#26504=ORIENTED_EDGE('',*,*,#19159,.F.);
#26505=ORIENTED_EDGE('',*,*,#19154,.F.);
#26506=ORIENTED_EDGE('',*,*,#19093,.T.);
#26507=ORIENTED_EDGE('',*,*,#19160,.T.);
#26508=ORIENTED_EDGE('',*,*,#19152,.T.);
#26509=ORIENTED_EDGE('',*,*,#19153,.T.);
#26510=ORIENTED_EDGE('',*,*,#19158,.T.);
#26511=ORIENTED_EDGE('',*,*,#19161,.F.);
#26512=ORIENTED_EDGE('',*,*,#19162,.F.);
#26513=ORIENTED_EDGE('',*,*,#19163,.T.);
#26514=ORIENTED_EDGE('',*,*,#19131,.T.);
#26515=ORIENTED_EDGE('',*,*,#19129,.T.);
#26516=ORIENTED_EDGE('',*,*,#19163,.F.);
#26517=ORIENTED_EDGE('',*,*,#19164,.F.);
#26518=ORIENTED_EDGE('',*,*,#19162,.T.);
#26519=ORIENTED_EDGE('',*,*,#19098,.F.);
#26520=ORIENTED_EDGE('',*,*,#19160,.F.);
#26521=ORIENTED_EDGE('',*,*,#19165,.T.);
#26522=ORIENTED_EDGE('',*,*,#19164,.T.);
#26523=ORIENTED_EDGE('',*,*,#19165,.F.);
#26524=ORIENTED_EDGE('',*,*,#19094,.T.);
#26525=ORIENTED_EDGE('',*,*,#19166,.T.);
#26526=ORIENTED_EDGE('',*,*,#19167,.F.);
#26527=ORIENTED_EDGE('',*,*,#19166,.F.);
#26528=ORIENTED_EDGE('',*,*,#19161,.T.);
#26529=ORIENTED_EDGE('',*,*,#19167,.T.);
#26530=ORIENTED_EDGE('',*,*,#19168,.F.);
#26531=ORIENTED_EDGE('',*,*,#19145,.F.);
#26532=ORIENTED_EDGE('',*,*,#19146,.F.);
#26533=ORIENTED_EDGE('',*,*,#19169,.T.);
#26534=ORIENTED_EDGE('',*,*,#19168,.T.);
#26535=ORIENTED_EDGE('',*,*,#19169,.F.);
#26536=ORIENTED_EDGE('',*,*,#19170,.F.);
#26537=ORIENTED_EDGE('',*,*,#19171,.F.);
#26538=ORIENTED_EDGE('',*,*,#19172,.T.);
#26539=ORIENTED_EDGE('',*,*,#19173,.F.);
#26540=ORIENTED_EDGE('',*,*,#19174,.F.);
#26541=ORIENTED_EDGE('',*,*,#19175,.T.);
#26542=ORIENTED_EDGE('',*,*,#19176,.F.);
#26543=ORIENTED_EDGE('',*,*,#19172,.F.);
#26544=ORIENTED_EDGE('',*,*,#19177,.F.);
#26545=ORIENTED_EDGE('',*,*,#19178,.F.);
#26546=ORIENTED_EDGE('',*,*,#19175,.F.);
#26547=ORIENTED_EDGE('',*,*,#19179,.F.);
#26548=ORIENTED_EDGE('',*,*,#19180,.T.);
#26549=ORIENTED_EDGE('',*,*,#19173,.T.);
#26550=ORIENTED_EDGE('',*,*,#19176,.T.);
#26551=ORIENTED_EDGE('',*,*,#19178,.T.);
#26552=ORIENTED_EDGE('',*,*,#19181,.T.);
#26553=ORIENTED_EDGE('',*,*,#19170,.T.);
#26554=ORIENTED_EDGE('',*,*,#19181,.F.);
#26555=ORIENTED_EDGE('',*,*,#19177,.T.);
#26556=ORIENTED_EDGE('',*,*,#19182,.F.);
#26557=ORIENTED_EDGE('',*,*,#19183,.F.);
#26558=ORIENTED_EDGE('',*,*,#19184,.T.);
#26559=ORIENTED_EDGE('',*,*,#19180,.F.);
#26560=ORIENTED_EDGE('',*,*,#19184,.F.);
#26561=ORIENTED_EDGE('',*,*,#19183,.T.);
#26562=ORIENTED_EDGE('',*,*,#19171,.T.);
#26563=ORIENTED_EDGE('',*,*,#19182,.T.);
#26564=ORIENTED_EDGE('',*,*,#19179,.T.);
#26565=ORIENTED_EDGE('',*,*,#19174,.T.);
#26566=ORIENTED_EDGE('',*,*,#19185,.F.);
#26567=ORIENTED_EDGE('',*,*,#19186,.T.);
#26568=ORIENTED_EDGE('',*,*,#19187,.F.);
#26569=ORIENTED_EDGE('',*,*,#19186,.F.);
#26570=ORIENTED_EDGE('',*,*,#19188,.T.);
#26571=ORIENTED_EDGE('',*,*,#19189,.T.);
#26572=ORIENTED_EDGE('',*,*,#19190,.F.);
#26573=ORIENTED_EDGE('',*,*,#19189,.F.);
#26574=ORIENTED_EDGE('',*,*,#19188,.F.);
#26575=ORIENTED_EDGE('',*,*,#19187,.T.);
#26576=ORIENTED_EDGE('',*,*,#19190,.T.);
#26577=ORIENTED_EDGE('',*,*,#19185,.T.);
#26578=ORIENTED_EDGE('',*,*,#19191,.T.);
#26579=ORIENTED_EDGE('',*,*,#19192,.T.);
#26580=ORIENTED_EDGE('',*,*,#19193,.T.);
#26581=ORIENTED_EDGE('',*,*,#19194,.T.);
#26582=ORIENTED_EDGE('',*,*,#19192,.F.);
#26583=ORIENTED_EDGE('',*,*,#19194,.F.);
#26584=ORIENTED_EDGE('',*,*,#19195,.T.);
#26585=ORIENTED_EDGE('',*,*,#19196,.F.);
#26586=ORIENTED_EDGE('',*,*,#19195,.F.);
#26587=ORIENTED_EDGE('',*,*,#19193,.F.);
#26588=ORIENTED_EDGE('',*,*,#19191,.F.);
#26589=ORIENTED_EDGE('',*,*,#19197,.T.);
#26590=ORIENTED_EDGE('',*,*,#19198,.T.);
#26591=ORIENTED_EDGE('',*,*,#19199,.T.);
#26592=ORIENTED_EDGE('',*,*,#19200,.T.);
#26593=ORIENTED_EDGE('',*,*,#19201,.T.);
#26594=ORIENTED_EDGE('',*,*,#19202,.T.);
#26595=ORIENTED_EDGE('',*,*,#19196,.T.);
#26596=ORIENTED_EDGE('',*,*,#19202,.F.);
#26597=ORIENTED_EDGE('',*,*,#19203,.T.);
#26598=ORIENTED_EDGE('',*,*,#19204,.T.);
#26599=ORIENTED_EDGE('',*,*,#19205,.T.);
#26600=ORIENTED_EDGE('',*,*,#19206,.F.);
#26601=ORIENTED_EDGE('',*,*,#19207,.T.);
#26602=ORIENTED_EDGE('',*,*,#19208,.T.);
#26603=ORIENTED_EDGE('',*,*,#19209,.T.);
#26604=ORIENTED_EDGE('',*,*,#19210,.F.);
#26605=ORIENTED_EDGE('',*,*,#19211,.T.);
#26606=ORIENTED_EDGE('',*,*,#19212,.T.);
#26607=ORIENTED_EDGE('',*,*,#19213,.T.);
#26608=ORIENTED_EDGE('',*,*,#19214,.F.);
#26609=ORIENTED_EDGE('',*,*,#19215,.T.);
#26610=ORIENTED_EDGE('',*,*,#19216,.T.);
#26611=ORIENTED_EDGE('',*,*,#19217,.T.);
#26612=ORIENTED_EDGE('',*,*,#19218,.F.);
#26613=ORIENTED_EDGE('',*,*,#19219,.T.);
#26614=ORIENTED_EDGE('',*,*,#19220,.T.);
#26615=ORIENTED_EDGE('',*,*,#19221,.T.);
#26616=ORIENTED_EDGE('',*,*,#19222,.F.);
#26617=ORIENTED_EDGE('',*,*,#19223,.T.);
#26618=ORIENTED_EDGE('',*,*,#19224,.T.);
#26619=ORIENTED_EDGE('',*,*,#19225,.T.);
#26620=ORIENTED_EDGE('',*,*,#19226,.F.);
#26621=ORIENTED_EDGE('',*,*,#19227,.T.);
#26622=ORIENTED_EDGE('',*,*,#19228,.T.);
#26623=ORIENTED_EDGE('',*,*,#19229,.T.);
#26624=ORIENTED_EDGE('',*,*,#19230,.F.);
#26625=ORIENTED_EDGE('',*,*,#19231,.T.);
#26626=ORIENTED_EDGE('',*,*,#19232,.T.);
#26627=ORIENTED_EDGE('',*,*,#19233,.T.);
#26628=ORIENTED_EDGE('',*,*,#19234,.F.);
#26629=ORIENTED_EDGE('',*,*,#19235,.T.);
#26630=ORIENTED_EDGE('',*,*,#19236,.T.);
#26631=ORIENTED_EDGE('',*,*,#19237,.T.);
#26632=ORIENTED_EDGE('',*,*,#19238,.F.);
#26633=ORIENTED_EDGE('',*,*,#19239,.T.);
#26634=ORIENTED_EDGE('',*,*,#19240,.T.);
#26635=ORIENTED_EDGE('',*,*,#19241,.T.);
#26636=ORIENTED_EDGE('',*,*,#19242,.F.);
#26637=ORIENTED_EDGE('',*,*,#19243,.T.);
#26638=ORIENTED_EDGE('',*,*,#19244,.T.);
#26639=ORIENTED_EDGE('',*,*,#19245,.T.);
#26640=ORIENTED_EDGE('',*,*,#19246,.F.);
#26641=ORIENTED_EDGE('',*,*,#19247,.T.);
#26642=ORIENTED_EDGE('',*,*,#19248,.T.);
#26643=ORIENTED_EDGE('',*,*,#19249,.T.);
#26644=ORIENTED_EDGE('',*,*,#19250,.F.);
#26645=ORIENTED_EDGE('',*,*,#19251,.T.);
#26646=ORIENTED_EDGE('',*,*,#19252,.T.);
#26647=ORIENTED_EDGE('',*,*,#19253,.T.);
#26648=ORIENTED_EDGE('',*,*,#19254,.F.);
#26649=ORIENTED_EDGE('',*,*,#19255,.T.);
#26650=ORIENTED_EDGE('',*,*,#19256,.T.);
#26651=ORIENTED_EDGE('',*,*,#19257,.T.);
#26652=ORIENTED_EDGE('',*,*,#19258,.F.);
#26653=ORIENTED_EDGE('',*,*,#19259,.T.);
#26654=ORIENTED_EDGE('',*,*,#19260,.T.);
#26655=ORIENTED_EDGE('',*,*,#19261,.T.);
#26656=ORIENTED_EDGE('',*,*,#19262,.F.);
#26657=ORIENTED_EDGE('',*,*,#19263,.T.);
#26658=ORIENTED_EDGE('',*,*,#19264,.T.);
#26659=ORIENTED_EDGE('',*,*,#19265,.T.);
#26660=ORIENTED_EDGE('',*,*,#19266,.F.);
#26661=ORIENTED_EDGE('',*,*,#19267,.T.);
#26662=ORIENTED_EDGE('',*,*,#19268,.T.);
#26663=ORIENTED_EDGE('',*,*,#19269,.T.);
#26664=ORIENTED_EDGE('',*,*,#19270,.F.);
#26665=ORIENTED_EDGE('',*,*,#19271,.T.);
#26666=ORIENTED_EDGE('',*,*,#19272,.T.);
#26667=ORIENTED_EDGE('',*,*,#19273,.T.);
#26668=ORIENTED_EDGE('',*,*,#19274,.F.);
#26669=ORIENTED_EDGE('',*,*,#19275,.T.);
#26670=ORIENTED_EDGE('',*,*,#19276,.T.);
#26671=ORIENTED_EDGE('',*,*,#19277,.T.);
#26672=ORIENTED_EDGE('',*,*,#19278,.F.);
#26673=ORIENTED_EDGE('',*,*,#19279,.T.);
#26674=ORIENTED_EDGE('',*,*,#19280,.T.);
#26675=ORIENTED_EDGE('',*,*,#19281,.T.);
#26676=ORIENTED_EDGE('',*,*,#19282,.F.);
#26677=ORIENTED_EDGE('',*,*,#19283,.T.);
#26678=ORIENTED_EDGE('',*,*,#19284,.T.);
#26679=ORIENTED_EDGE('',*,*,#19285,.T.);
#26680=ORIENTED_EDGE('',*,*,#19286,.F.);
#26681=ORIENTED_EDGE('',*,*,#19287,.T.);
#26682=ORIENTED_EDGE('',*,*,#19288,.T.);
#26683=ORIENTED_EDGE('',*,*,#19289,.T.);
#26684=ORIENTED_EDGE('',*,*,#19290,.F.);
#26685=ORIENTED_EDGE('',*,*,#19291,.T.);
#26686=ORIENTED_EDGE('',*,*,#19292,.T.);
#26687=ORIENTED_EDGE('',*,*,#19293,.T.);
#26688=ORIENTED_EDGE('',*,*,#19294,.F.);
#26689=ORIENTED_EDGE('',*,*,#19295,.T.);
#26690=ORIENTED_EDGE('',*,*,#19296,.T.);
#26691=ORIENTED_EDGE('',*,*,#19297,.T.);
#26692=ORIENTED_EDGE('',*,*,#19298,.F.);
#26693=ORIENTED_EDGE('',*,*,#19299,.T.);
#26694=ORIENTED_EDGE('',*,*,#19300,.T.);
#26695=ORIENTED_EDGE('',*,*,#19301,.T.);
#26696=ORIENTED_EDGE('',*,*,#19302,.F.);
#26697=ORIENTED_EDGE('',*,*,#19303,.T.);
#26698=ORIENTED_EDGE('',*,*,#19304,.T.);
#26699=ORIENTED_EDGE('',*,*,#19305,.T.);
#26700=ORIENTED_EDGE('',*,*,#19306,.F.);
#26701=ORIENTED_EDGE('',*,*,#19307,.T.);
#26702=ORIENTED_EDGE('',*,*,#19308,.T.);
#26703=ORIENTED_EDGE('',*,*,#19309,.T.);
#26704=ORIENTED_EDGE('',*,*,#19310,.F.);
#26705=ORIENTED_EDGE('',*,*,#19311,.T.);
#26706=ORIENTED_EDGE('',*,*,#19312,.T.);
#26707=ORIENTED_EDGE('',*,*,#19313,.T.);
#26708=ORIENTED_EDGE('',*,*,#19314,.F.);
#26709=ORIENTED_EDGE('',*,*,#19315,.T.);
#26710=ORIENTED_EDGE('',*,*,#19316,.T.);
#26711=ORIENTED_EDGE('',*,*,#19317,.T.);
#26712=ORIENTED_EDGE('',*,*,#19318,.F.);
#26713=ORIENTED_EDGE('',*,*,#19319,.T.);
#26714=ORIENTED_EDGE('',*,*,#19320,.T.);
#26715=ORIENTED_EDGE('',*,*,#19321,.T.);
#26716=ORIENTED_EDGE('',*,*,#19322,.F.);
#26717=ORIENTED_EDGE('',*,*,#19323,.T.);
#26718=ORIENTED_EDGE('',*,*,#19324,.T.);
#26719=ORIENTED_EDGE('',*,*,#19325,.T.);
#26720=ORIENTED_EDGE('',*,*,#19326,.F.);
#26721=ORIENTED_EDGE('',*,*,#19327,.T.);
#26722=ORIENTED_EDGE('',*,*,#19328,.T.);
#26723=ORIENTED_EDGE('',*,*,#19329,.T.);
#26724=ORIENTED_EDGE('',*,*,#19330,.F.);
#26725=ORIENTED_EDGE('',*,*,#19331,.T.);
#26726=ORIENTED_EDGE('',*,*,#19332,.T.);
#26727=ORIENTED_EDGE('',*,*,#19333,.T.);
#26728=ORIENTED_EDGE('',*,*,#19334,.F.);
#26729=ORIENTED_EDGE('',*,*,#19335,.T.);
#26730=ORIENTED_EDGE('',*,*,#19336,.T.);
#26731=ORIENTED_EDGE('',*,*,#19337,.T.);
#26732=ORIENTED_EDGE('',*,*,#19338,.F.);
#26733=ORIENTED_EDGE('',*,*,#19339,.T.);
#26734=ORIENTED_EDGE('',*,*,#19340,.T.);
#26735=ORIENTED_EDGE('',*,*,#19341,.T.);
#26736=ORIENTED_EDGE('',*,*,#19342,.F.);
#26737=ORIENTED_EDGE('',*,*,#19343,.T.);
#26738=ORIENTED_EDGE('',*,*,#19344,.T.);
#26739=ORIENTED_EDGE('',*,*,#19345,.T.);
#26740=ORIENTED_EDGE('',*,*,#19346,.F.);
#26741=ORIENTED_EDGE('',*,*,#19347,.T.);
#26742=ORIENTED_EDGE('',*,*,#19348,.T.);
#26743=ORIENTED_EDGE('',*,*,#19349,.T.);
#26744=ORIENTED_EDGE('',*,*,#19350,.F.);
#26745=ORIENTED_EDGE('',*,*,#19351,.T.);
#26746=ORIENTED_EDGE('',*,*,#19352,.T.);
#26747=ORIENTED_EDGE('',*,*,#19353,.T.);
#26748=ORIENTED_EDGE('',*,*,#19354,.F.);
#26749=ORIENTED_EDGE('',*,*,#19355,.T.);
#26750=ORIENTED_EDGE('',*,*,#19356,.T.);
#26751=ORIENTED_EDGE('',*,*,#19357,.T.);
#26752=ORIENTED_EDGE('',*,*,#19358,.F.);
#26753=ORIENTED_EDGE('',*,*,#19359,.T.);
#26754=ORIENTED_EDGE('',*,*,#19360,.T.);
#26755=ORIENTED_EDGE('',*,*,#19361,.T.);
#26756=ORIENTED_EDGE('',*,*,#19362,.F.);
#26757=ORIENTED_EDGE('',*,*,#19363,.T.);
#26758=ORIENTED_EDGE('',*,*,#19364,.T.);
#26759=ORIENTED_EDGE('',*,*,#19365,.T.);
#26760=ORIENTED_EDGE('',*,*,#19366,.F.);
#26761=ORIENTED_EDGE('',*,*,#19367,.T.);
#26762=ORIENTED_EDGE('',*,*,#19368,.T.);
#26763=ORIENTED_EDGE('',*,*,#19369,.T.);
#26764=ORIENTED_EDGE('',*,*,#19370,.F.);
#26765=ORIENTED_EDGE('',*,*,#19371,.T.);
#26766=ORIENTED_EDGE('',*,*,#19372,.T.);
#26767=ORIENTED_EDGE('',*,*,#19373,.T.);
#26768=ORIENTED_EDGE('',*,*,#19374,.F.);
#26769=ORIENTED_EDGE('',*,*,#19375,.T.);
#26770=ORIENTED_EDGE('',*,*,#19376,.T.);
#26771=ORIENTED_EDGE('',*,*,#19377,.T.);
#26772=ORIENTED_EDGE('',*,*,#19378,.F.);
#26773=ORIENTED_EDGE('',*,*,#19379,.T.);
#26774=ORIENTED_EDGE('',*,*,#19380,.T.);
#26775=ORIENTED_EDGE('',*,*,#19381,.T.);
#26776=ORIENTED_EDGE('',*,*,#19382,.F.);
#26777=ORIENTED_EDGE('',*,*,#19383,.T.);
#26778=ORIENTED_EDGE('',*,*,#19384,.T.);
#26779=ORIENTED_EDGE('',*,*,#19385,.T.);
#26780=ORIENTED_EDGE('',*,*,#19386,.F.);
#26781=ORIENTED_EDGE('',*,*,#19387,.T.);
#26782=ORIENTED_EDGE('',*,*,#19388,.T.);
#26783=ORIENTED_EDGE('',*,*,#19389,.T.);
#26784=ORIENTED_EDGE('',*,*,#19390,.F.);
#26785=ORIENTED_EDGE('',*,*,#19391,.T.);
#26786=ORIENTED_EDGE('',*,*,#19392,.T.);
#26787=ORIENTED_EDGE('',*,*,#19393,.T.);
#26788=ORIENTED_EDGE('',*,*,#19394,.F.);
#26789=ORIENTED_EDGE('',*,*,#19201,.F.);
#26790=ORIENTED_EDGE('',*,*,#19395,.F.);
#26791=ORIENTED_EDGE('',*,*,#19396,.F.);
#26792=ORIENTED_EDGE('',*,*,#19198,.F.);
#26793=ORIENTED_EDGE('',*,*,#19397,.T.);
#26794=ORIENTED_EDGE('',*,*,#19398,.F.);
#26795=ORIENTED_EDGE('',*,*,#19397,.F.);
#26796=ORIENTED_EDGE('',*,*,#19197,.F.);
#26797=ORIENTED_EDGE('',*,*,#19399,.F.);
#26798=ORIENTED_EDGE('',*,*,#19400,.F.);
#26799=ORIENTED_EDGE('',*,*,#19399,.T.);
#26800=ORIENTED_EDGE('',*,*,#19200,.F.);
#26801=ORIENTED_EDGE('',*,*,#19401,.T.);
#26802=ORIENTED_EDGE('',*,*,#19402,.F.);
#26803=ORIENTED_EDGE('',*,*,#19401,.F.);
#26804=ORIENTED_EDGE('',*,*,#19199,.F.);
#26805=ORIENTED_EDGE('',*,*,#19396,.T.);
#26806=ORIENTED_EDGE('',*,*,#19204,.F.);
#26807=ORIENTED_EDGE('',*,*,#19403,.F.);
#26808=ORIENTED_EDGE('',*,*,#19404,.F.);
#26809=ORIENTED_EDGE('',*,*,#19405,.T.);
#26810=ORIENTED_EDGE('',*,*,#19205,.F.);
#26811=ORIENTED_EDGE('',*,*,#19405,.F.);
#26812=ORIENTED_EDGE('',*,*,#19406,.F.);
#26813=ORIENTED_EDGE('',*,*,#19407,.F.);
#26814=ORIENTED_EDGE('',*,*,#19203,.F.);
#26815=ORIENTED_EDGE('',*,*,#19408,.F.);
#26816=ORIENTED_EDGE('',*,*,#19409,.F.);
#26817=ORIENTED_EDGE('',*,*,#19403,.T.);
#26818=ORIENTED_EDGE('',*,*,#19208,.F.);
#26819=ORIENTED_EDGE('',*,*,#19410,.F.);
#26820=ORIENTED_EDGE('',*,*,#19411,.F.);
#26821=ORIENTED_EDGE('',*,*,#19412,.T.);
#26822=ORIENTED_EDGE('',*,*,#19209,.F.);
#26823=ORIENTED_EDGE('',*,*,#19412,.F.);
#26824=ORIENTED_EDGE('',*,*,#19413,.F.);
#26825=ORIENTED_EDGE('',*,*,#19414,.F.);
#26826=ORIENTED_EDGE('',*,*,#19207,.F.);
#26827=ORIENTED_EDGE('',*,*,#19415,.F.);
#26828=ORIENTED_EDGE('',*,*,#19416,.F.);
#26829=ORIENTED_EDGE('',*,*,#19410,.T.);
#26830=ORIENTED_EDGE('',*,*,#19212,.F.);
#26831=ORIENTED_EDGE('',*,*,#19417,.F.);
#26832=ORIENTED_EDGE('',*,*,#19418,.F.);
#26833=ORIENTED_EDGE('',*,*,#19419,.T.);
#26834=ORIENTED_EDGE('',*,*,#19213,.F.);
#26835=ORIENTED_EDGE('',*,*,#19419,.F.);
#26836=ORIENTED_EDGE('',*,*,#19420,.F.);
#26837=ORIENTED_EDGE('',*,*,#19421,.F.);
#26838=ORIENTED_EDGE('',*,*,#19211,.F.);
#26839=ORIENTED_EDGE('',*,*,#19422,.F.);
#26840=ORIENTED_EDGE('',*,*,#19423,.F.);
#26841=ORIENTED_EDGE('',*,*,#19417,.T.);
#26842=ORIENTED_EDGE('',*,*,#19216,.F.);
#26843=ORIENTED_EDGE('',*,*,#19424,.F.);
#26844=ORIENTED_EDGE('',*,*,#19425,.F.);
#26845=ORIENTED_EDGE('',*,*,#19426,.T.);
#26846=ORIENTED_EDGE('',*,*,#19217,.F.);
#26847=ORIENTED_EDGE('',*,*,#19426,.F.);
#26848=ORIENTED_EDGE('',*,*,#19427,.F.);
#26849=ORIENTED_EDGE('',*,*,#19428,.F.);
#26850=ORIENTED_EDGE('',*,*,#19215,.F.);
#26851=ORIENTED_EDGE('',*,*,#19429,.F.);
#26852=ORIENTED_EDGE('',*,*,#19430,.F.);
#26853=ORIENTED_EDGE('',*,*,#19424,.T.);
#26854=ORIENTED_EDGE('',*,*,#19220,.F.);
#26855=ORIENTED_EDGE('',*,*,#19431,.F.);
#26856=ORIENTED_EDGE('',*,*,#19432,.F.);
#26857=ORIENTED_EDGE('',*,*,#19433,.T.);
#26858=ORIENTED_EDGE('',*,*,#19221,.F.);
#26859=ORIENTED_EDGE('',*,*,#19433,.F.);
#26860=ORIENTED_EDGE('',*,*,#19434,.F.);
#26861=ORIENTED_EDGE('',*,*,#19435,.F.);
#26862=ORIENTED_EDGE('',*,*,#19219,.F.);
#26863=ORIENTED_EDGE('',*,*,#19436,.F.);
#26864=ORIENTED_EDGE('',*,*,#19437,.F.);
#26865=ORIENTED_EDGE('',*,*,#19431,.T.);
#26866=ORIENTED_EDGE('',*,*,#19224,.F.);
#26867=ORIENTED_EDGE('',*,*,#19438,.F.);
#26868=ORIENTED_EDGE('',*,*,#19439,.F.);
#26869=ORIENTED_EDGE('',*,*,#19440,.T.);
#26870=ORIENTED_EDGE('',*,*,#19225,.F.);
#26871=ORIENTED_EDGE('',*,*,#19440,.F.);
#26872=ORIENTED_EDGE('',*,*,#19441,.F.);
#26873=ORIENTED_EDGE('',*,*,#19442,.F.);
#26874=ORIENTED_EDGE('',*,*,#19223,.F.);
#26875=ORIENTED_EDGE('',*,*,#19443,.F.);
#26876=ORIENTED_EDGE('',*,*,#19444,.F.);
#26877=ORIENTED_EDGE('',*,*,#19438,.T.);
#26878=ORIENTED_EDGE('',*,*,#19228,.F.);
#26879=ORIENTED_EDGE('',*,*,#19445,.F.);
#26880=ORIENTED_EDGE('',*,*,#19446,.F.);
#26881=ORIENTED_EDGE('',*,*,#19447,.T.);
#26882=ORIENTED_EDGE('',*,*,#19229,.F.);
#26883=ORIENTED_EDGE('',*,*,#19447,.F.);
#26884=ORIENTED_EDGE('',*,*,#19448,.F.);
#26885=ORIENTED_EDGE('',*,*,#19449,.F.);
#26886=ORIENTED_EDGE('',*,*,#19227,.F.);
#26887=ORIENTED_EDGE('',*,*,#19450,.F.);
#26888=ORIENTED_EDGE('',*,*,#19451,.F.);
#26889=ORIENTED_EDGE('',*,*,#19445,.T.);
#26890=ORIENTED_EDGE('',*,*,#19232,.F.);
#26891=ORIENTED_EDGE('',*,*,#19452,.F.);
#26892=ORIENTED_EDGE('',*,*,#19453,.F.);
#26893=ORIENTED_EDGE('',*,*,#19454,.T.);
#26894=ORIENTED_EDGE('',*,*,#19233,.F.);
#26895=ORIENTED_EDGE('',*,*,#19454,.F.);
#26896=ORIENTED_EDGE('',*,*,#19455,.F.);
#26897=ORIENTED_EDGE('',*,*,#19456,.F.);
#26898=ORIENTED_EDGE('',*,*,#19231,.F.);
#26899=ORIENTED_EDGE('',*,*,#19457,.F.);
#26900=ORIENTED_EDGE('',*,*,#19458,.F.);
#26901=ORIENTED_EDGE('',*,*,#19452,.T.);
#26902=ORIENTED_EDGE('',*,*,#19236,.F.);
#26903=ORIENTED_EDGE('',*,*,#19459,.F.);
#26904=ORIENTED_EDGE('',*,*,#19460,.F.);
#26905=ORIENTED_EDGE('',*,*,#19461,.T.);
#26906=ORIENTED_EDGE('',*,*,#19237,.F.);
#26907=ORIENTED_EDGE('',*,*,#19461,.F.);
#26908=ORIENTED_EDGE('',*,*,#19462,.F.);
#26909=ORIENTED_EDGE('',*,*,#19463,.F.);
#26910=ORIENTED_EDGE('',*,*,#19235,.F.);
#26911=ORIENTED_EDGE('',*,*,#19464,.F.);
#26912=ORIENTED_EDGE('',*,*,#19465,.F.);
#26913=ORIENTED_EDGE('',*,*,#19459,.T.);
#26914=ORIENTED_EDGE('',*,*,#19240,.F.);
#26915=ORIENTED_EDGE('',*,*,#19466,.F.);
#26916=ORIENTED_EDGE('',*,*,#19467,.F.);
#26917=ORIENTED_EDGE('',*,*,#19468,.T.);
#26918=ORIENTED_EDGE('',*,*,#19241,.F.);
#26919=ORIENTED_EDGE('',*,*,#19468,.F.);
#26920=ORIENTED_EDGE('',*,*,#19469,.F.);
#26921=ORIENTED_EDGE('',*,*,#19470,.F.);
#26922=ORIENTED_EDGE('',*,*,#19239,.F.);
#26923=ORIENTED_EDGE('',*,*,#19471,.F.);
#26924=ORIENTED_EDGE('',*,*,#19472,.F.);
#26925=ORIENTED_EDGE('',*,*,#19466,.T.);
#26926=ORIENTED_EDGE('',*,*,#19244,.F.);
#26927=ORIENTED_EDGE('',*,*,#19473,.F.);
#26928=ORIENTED_EDGE('',*,*,#19474,.F.);
#26929=ORIENTED_EDGE('',*,*,#19475,.T.);
#26930=ORIENTED_EDGE('',*,*,#19245,.F.);
#26931=ORIENTED_EDGE('',*,*,#19475,.F.);
#26932=ORIENTED_EDGE('',*,*,#19476,.F.);
#26933=ORIENTED_EDGE('',*,*,#19477,.F.);
#26934=ORIENTED_EDGE('',*,*,#19243,.F.);
#26935=ORIENTED_EDGE('',*,*,#19478,.F.);
#26936=ORIENTED_EDGE('',*,*,#19479,.F.);
#26937=ORIENTED_EDGE('',*,*,#19473,.T.);
#26938=ORIENTED_EDGE('',*,*,#19248,.F.);
#26939=ORIENTED_EDGE('',*,*,#19480,.F.);
#26940=ORIENTED_EDGE('',*,*,#19481,.F.);
#26941=ORIENTED_EDGE('',*,*,#19482,.T.);
#26942=ORIENTED_EDGE('',*,*,#19249,.F.);
#26943=ORIENTED_EDGE('',*,*,#19482,.F.);
#26944=ORIENTED_EDGE('',*,*,#19483,.F.);
#26945=ORIENTED_EDGE('',*,*,#19484,.F.);
#26946=ORIENTED_EDGE('',*,*,#19247,.F.);
#26947=ORIENTED_EDGE('',*,*,#19485,.F.);
#26948=ORIENTED_EDGE('',*,*,#19486,.F.);
#26949=ORIENTED_EDGE('',*,*,#19480,.T.);
#26950=ORIENTED_EDGE('',*,*,#19252,.F.);
#26951=ORIENTED_EDGE('',*,*,#19487,.F.);
#26952=ORIENTED_EDGE('',*,*,#19488,.F.);
#26953=ORIENTED_EDGE('',*,*,#19489,.T.);
#26954=ORIENTED_EDGE('',*,*,#19253,.F.);
#26955=ORIENTED_EDGE('',*,*,#19489,.F.);
#26956=ORIENTED_EDGE('',*,*,#19490,.F.);
#26957=ORIENTED_EDGE('',*,*,#19491,.F.);
#26958=ORIENTED_EDGE('',*,*,#19251,.F.);
#26959=ORIENTED_EDGE('',*,*,#19492,.F.);
#26960=ORIENTED_EDGE('',*,*,#19493,.F.);
#26961=ORIENTED_EDGE('',*,*,#19487,.T.);
#26962=ORIENTED_EDGE('',*,*,#19256,.F.);
#26963=ORIENTED_EDGE('',*,*,#19494,.F.);
#26964=ORIENTED_EDGE('',*,*,#19495,.F.);
#26965=ORIENTED_EDGE('',*,*,#19496,.T.);
#26966=ORIENTED_EDGE('',*,*,#19257,.F.);
#26967=ORIENTED_EDGE('',*,*,#19496,.F.);
#26968=ORIENTED_EDGE('',*,*,#19497,.F.);
#26969=ORIENTED_EDGE('',*,*,#19498,.F.);
#26970=ORIENTED_EDGE('',*,*,#19255,.F.);
#26971=ORIENTED_EDGE('',*,*,#19499,.F.);
#26972=ORIENTED_EDGE('',*,*,#19500,.F.);
#26973=ORIENTED_EDGE('',*,*,#19494,.T.);
#26974=ORIENTED_EDGE('',*,*,#19260,.F.);
#26975=ORIENTED_EDGE('',*,*,#19501,.F.);
#26976=ORIENTED_EDGE('',*,*,#19502,.F.);
#26977=ORIENTED_EDGE('',*,*,#19503,.T.);
#26978=ORIENTED_EDGE('',*,*,#19261,.F.);
#26979=ORIENTED_EDGE('',*,*,#19503,.F.);
#26980=ORIENTED_EDGE('',*,*,#19504,.F.);
#26981=ORIENTED_EDGE('',*,*,#19505,.F.);
#26982=ORIENTED_EDGE('',*,*,#19259,.F.);
#26983=ORIENTED_EDGE('',*,*,#19506,.F.);
#26984=ORIENTED_EDGE('',*,*,#19507,.F.);
#26985=ORIENTED_EDGE('',*,*,#19501,.T.);
#26986=ORIENTED_EDGE('',*,*,#19264,.F.);
#26987=ORIENTED_EDGE('',*,*,#19508,.F.);
#26988=ORIENTED_EDGE('',*,*,#19509,.F.);
#26989=ORIENTED_EDGE('',*,*,#19510,.T.);
#26990=ORIENTED_EDGE('',*,*,#19265,.F.);
#26991=ORIENTED_EDGE('',*,*,#19510,.F.);
#26992=ORIENTED_EDGE('',*,*,#19511,.F.);
#26993=ORIENTED_EDGE('',*,*,#19512,.F.);
#26994=ORIENTED_EDGE('',*,*,#19263,.F.);
#26995=ORIENTED_EDGE('',*,*,#19513,.F.);
#26996=ORIENTED_EDGE('',*,*,#19514,.F.);
#26997=ORIENTED_EDGE('',*,*,#19508,.T.);
#26998=ORIENTED_EDGE('',*,*,#19268,.F.);
#26999=ORIENTED_EDGE('',*,*,#19515,.F.);
#27000=ORIENTED_EDGE('',*,*,#19516,.F.);
#27001=ORIENTED_EDGE('',*,*,#19517,.T.);
#27002=ORIENTED_EDGE('',*,*,#19269,.F.);
#27003=ORIENTED_EDGE('',*,*,#19517,.F.);
#27004=ORIENTED_EDGE('',*,*,#19518,.F.);
#27005=ORIENTED_EDGE('',*,*,#19519,.F.);
#27006=ORIENTED_EDGE('',*,*,#19267,.F.);
#27007=ORIENTED_EDGE('',*,*,#19520,.F.);
#27008=ORIENTED_EDGE('',*,*,#19521,.F.);
#27009=ORIENTED_EDGE('',*,*,#19515,.T.);
#27010=ORIENTED_EDGE('',*,*,#19272,.F.);
#27011=ORIENTED_EDGE('',*,*,#19522,.F.);
#27012=ORIENTED_EDGE('',*,*,#19523,.F.);
#27013=ORIENTED_EDGE('',*,*,#19524,.T.);
#27014=ORIENTED_EDGE('',*,*,#19273,.F.);
#27015=ORIENTED_EDGE('',*,*,#19524,.F.);
#27016=ORIENTED_EDGE('',*,*,#19525,.F.);
#27017=ORIENTED_EDGE('',*,*,#19526,.F.);
#27018=ORIENTED_EDGE('',*,*,#19271,.F.);
#27019=ORIENTED_EDGE('',*,*,#19527,.F.);
#27020=ORIENTED_EDGE('',*,*,#19528,.F.);
#27021=ORIENTED_EDGE('',*,*,#19522,.T.);
#27022=ORIENTED_EDGE('',*,*,#19276,.F.);
#27023=ORIENTED_EDGE('',*,*,#19529,.F.);
#27024=ORIENTED_EDGE('',*,*,#19530,.F.);
#27025=ORIENTED_EDGE('',*,*,#19531,.T.);
#27026=ORIENTED_EDGE('',*,*,#19277,.F.);
#27027=ORIENTED_EDGE('',*,*,#19531,.F.);
#27028=ORIENTED_EDGE('',*,*,#19532,.F.);
#27029=ORIENTED_EDGE('',*,*,#19533,.F.);
#27030=ORIENTED_EDGE('',*,*,#19275,.F.);
#27031=ORIENTED_EDGE('',*,*,#19534,.F.);
#27032=ORIENTED_EDGE('',*,*,#19535,.F.);
#27033=ORIENTED_EDGE('',*,*,#19529,.T.);
#27034=ORIENTED_EDGE('',*,*,#19280,.F.);
#27035=ORIENTED_EDGE('',*,*,#19536,.F.);
#27036=ORIENTED_EDGE('',*,*,#19537,.F.);
#27037=ORIENTED_EDGE('',*,*,#19538,.T.);
#27038=ORIENTED_EDGE('',*,*,#19281,.F.);
#27039=ORIENTED_EDGE('',*,*,#19538,.F.);
#27040=ORIENTED_EDGE('',*,*,#19539,.F.);
#27041=ORIENTED_EDGE('',*,*,#19540,.F.);
#27042=ORIENTED_EDGE('',*,*,#19279,.F.);
#27043=ORIENTED_EDGE('',*,*,#19541,.F.);
#27044=ORIENTED_EDGE('',*,*,#19542,.F.);
#27045=ORIENTED_EDGE('',*,*,#19536,.T.);
#27046=ORIENTED_EDGE('',*,*,#19284,.F.);
#27047=ORIENTED_EDGE('',*,*,#19543,.F.);
#27048=ORIENTED_EDGE('',*,*,#19544,.F.);
#27049=ORIENTED_EDGE('',*,*,#19545,.T.);
#27050=ORIENTED_EDGE('',*,*,#19285,.F.);
#27051=ORIENTED_EDGE('',*,*,#19545,.F.);
#27052=ORIENTED_EDGE('',*,*,#19546,.F.);
#27053=ORIENTED_EDGE('',*,*,#19547,.F.);
#27054=ORIENTED_EDGE('',*,*,#19283,.F.);
#27055=ORIENTED_EDGE('',*,*,#19548,.F.);
#27056=ORIENTED_EDGE('',*,*,#19549,.F.);
#27057=ORIENTED_EDGE('',*,*,#19543,.T.);
#27058=ORIENTED_EDGE('',*,*,#19288,.F.);
#27059=ORIENTED_EDGE('',*,*,#19550,.F.);
#27060=ORIENTED_EDGE('',*,*,#19551,.F.);
#27061=ORIENTED_EDGE('',*,*,#19552,.T.);
#27062=ORIENTED_EDGE('',*,*,#19289,.F.);
#27063=ORIENTED_EDGE('',*,*,#19552,.F.);
#27064=ORIENTED_EDGE('',*,*,#19553,.F.);
#27065=ORIENTED_EDGE('',*,*,#19554,.F.);
#27066=ORIENTED_EDGE('',*,*,#19287,.F.);
#27067=ORIENTED_EDGE('',*,*,#19555,.F.);
#27068=ORIENTED_EDGE('',*,*,#19556,.F.);
#27069=ORIENTED_EDGE('',*,*,#19550,.T.);
#27070=ORIENTED_EDGE('',*,*,#19292,.F.);
#27071=ORIENTED_EDGE('',*,*,#19557,.F.);
#27072=ORIENTED_EDGE('',*,*,#19558,.F.);
#27073=ORIENTED_EDGE('',*,*,#19559,.T.);
#27074=ORIENTED_EDGE('',*,*,#19293,.F.);
#27075=ORIENTED_EDGE('',*,*,#19559,.F.);
#27076=ORIENTED_EDGE('',*,*,#19560,.F.);
#27077=ORIENTED_EDGE('',*,*,#19561,.F.);
#27078=ORIENTED_EDGE('',*,*,#19291,.F.);
#27079=ORIENTED_EDGE('',*,*,#19562,.F.);
#27080=ORIENTED_EDGE('',*,*,#19563,.F.);
#27081=ORIENTED_EDGE('',*,*,#19557,.T.);
#27082=ORIENTED_EDGE('',*,*,#19296,.F.);
#27083=ORIENTED_EDGE('',*,*,#19564,.F.);
#27084=ORIENTED_EDGE('',*,*,#19565,.F.);
#27085=ORIENTED_EDGE('',*,*,#19566,.T.);
#27086=ORIENTED_EDGE('',*,*,#19297,.F.);
#27087=ORIENTED_EDGE('',*,*,#19566,.F.);
#27088=ORIENTED_EDGE('',*,*,#19567,.F.);
#27089=ORIENTED_EDGE('',*,*,#19568,.F.);
#27090=ORIENTED_EDGE('',*,*,#19295,.F.);
#27091=ORIENTED_EDGE('',*,*,#19569,.F.);
#27092=ORIENTED_EDGE('',*,*,#19570,.F.);
#27093=ORIENTED_EDGE('',*,*,#19564,.T.);
#27094=ORIENTED_EDGE('',*,*,#19300,.F.);
#27095=ORIENTED_EDGE('',*,*,#19571,.F.);
#27096=ORIENTED_EDGE('',*,*,#19572,.F.);
#27097=ORIENTED_EDGE('',*,*,#19573,.T.);
#27098=ORIENTED_EDGE('',*,*,#19301,.F.);
#27099=ORIENTED_EDGE('',*,*,#19573,.F.);
#27100=ORIENTED_EDGE('',*,*,#19574,.F.);
#27101=ORIENTED_EDGE('',*,*,#19575,.F.);
#27102=ORIENTED_EDGE('',*,*,#19299,.F.);
#27103=ORIENTED_EDGE('',*,*,#19576,.F.);
#27104=ORIENTED_EDGE('',*,*,#19577,.F.);
#27105=ORIENTED_EDGE('',*,*,#19571,.T.);
#27106=ORIENTED_EDGE('',*,*,#19304,.F.);
#27107=ORIENTED_EDGE('',*,*,#19578,.F.);
#27108=ORIENTED_EDGE('',*,*,#19579,.F.);
#27109=ORIENTED_EDGE('',*,*,#19580,.T.);
#27110=ORIENTED_EDGE('',*,*,#19305,.F.);
#27111=ORIENTED_EDGE('',*,*,#19580,.F.);
#27112=ORIENTED_EDGE('',*,*,#19581,.F.);
#27113=ORIENTED_EDGE('',*,*,#19582,.F.);
#27114=ORIENTED_EDGE('',*,*,#19303,.F.);
#27115=ORIENTED_EDGE('',*,*,#19583,.F.);
#27116=ORIENTED_EDGE('',*,*,#19584,.F.);
#27117=ORIENTED_EDGE('',*,*,#19578,.T.);
#27118=ORIENTED_EDGE('',*,*,#19308,.F.);
#27119=ORIENTED_EDGE('',*,*,#19585,.F.);
#27120=ORIENTED_EDGE('',*,*,#19586,.F.);
#27121=ORIENTED_EDGE('',*,*,#19587,.T.);
#27122=ORIENTED_EDGE('',*,*,#19309,.F.);
#27123=ORIENTED_EDGE('',*,*,#19587,.F.);
#27124=ORIENTED_EDGE('',*,*,#19588,.F.);
#27125=ORIENTED_EDGE('',*,*,#19589,.F.);
#27126=ORIENTED_EDGE('',*,*,#19307,.F.);
#27127=ORIENTED_EDGE('',*,*,#19590,.F.);
#27128=ORIENTED_EDGE('',*,*,#19591,.F.);
#27129=ORIENTED_EDGE('',*,*,#19585,.T.);
#27130=ORIENTED_EDGE('',*,*,#19312,.F.);
#27131=ORIENTED_EDGE('',*,*,#19592,.F.);
#27132=ORIENTED_EDGE('',*,*,#19593,.F.);
#27133=ORIENTED_EDGE('',*,*,#19594,.T.);
#27134=ORIENTED_EDGE('',*,*,#19313,.F.);
#27135=ORIENTED_EDGE('',*,*,#19594,.F.);
#27136=ORIENTED_EDGE('',*,*,#19595,.F.);
#27137=ORIENTED_EDGE('',*,*,#19596,.F.);
#27138=ORIENTED_EDGE('',*,*,#19311,.F.);
#27139=ORIENTED_EDGE('',*,*,#19597,.F.);
#27140=ORIENTED_EDGE('',*,*,#19598,.F.);
#27141=ORIENTED_EDGE('',*,*,#19592,.T.);
#27142=ORIENTED_EDGE('',*,*,#19316,.F.);
#27143=ORIENTED_EDGE('',*,*,#19599,.F.);
#27144=ORIENTED_EDGE('',*,*,#19600,.F.);
#27145=ORIENTED_EDGE('',*,*,#19601,.T.);
#27146=ORIENTED_EDGE('',*,*,#19317,.F.);
#27147=ORIENTED_EDGE('',*,*,#19601,.F.);
#27148=ORIENTED_EDGE('',*,*,#19602,.F.);
#27149=ORIENTED_EDGE('',*,*,#19603,.F.);
#27150=ORIENTED_EDGE('',*,*,#19315,.F.);
#27151=ORIENTED_EDGE('',*,*,#19604,.F.);
#27152=ORIENTED_EDGE('',*,*,#19605,.F.);
#27153=ORIENTED_EDGE('',*,*,#19599,.T.);
#27154=ORIENTED_EDGE('',*,*,#19320,.F.);
#27155=ORIENTED_EDGE('',*,*,#19606,.F.);
#27156=ORIENTED_EDGE('',*,*,#19607,.F.);
#27157=ORIENTED_EDGE('',*,*,#19608,.T.);
#27158=ORIENTED_EDGE('',*,*,#19321,.F.);
#27159=ORIENTED_EDGE('',*,*,#19608,.F.);
#27160=ORIENTED_EDGE('',*,*,#19609,.F.);
#27161=ORIENTED_EDGE('',*,*,#19610,.F.);
#27162=ORIENTED_EDGE('',*,*,#19319,.F.);
#27163=ORIENTED_EDGE('',*,*,#19611,.F.);
#27164=ORIENTED_EDGE('',*,*,#19612,.F.);
#27165=ORIENTED_EDGE('',*,*,#19606,.T.);
#27166=ORIENTED_EDGE('',*,*,#19324,.F.);
#27167=ORIENTED_EDGE('',*,*,#19613,.F.);
#27168=ORIENTED_EDGE('',*,*,#19614,.F.);
#27169=ORIENTED_EDGE('',*,*,#19615,.T.);
#27170=ORIENTED_EDGE('',*,*,#19325,.F.);
#27171=ORIENTED_EDGE('',*,*,#19615,.F.);
#27172=ORIENTED_EDGE('',*,*,#19616,.F.);
#27173=ORIENTED_EDGE('',*,*,#19617,.F.);
#27174=ORIENTED_EDGE('',*,*,#19323,.F.);
#27175=ORIENTED_EDGE('',*,*,#19618,.F.);
#27176=ORIENTED_EDGE('',*,*,#19619,.F.);
#27177=ORIENTED_EDGE('',*,*,#19613,.T.);
#27178=ORIENTED_EDGE('',*,*,#19328,.F.);
#27179=ORIENTED_EDGE('',*,*,#19620,.F.);
#27180=ORIENTED_EDGE('',*,*,#19621,.F.);
#27181=ORIENTED_EDGE('',*,*,#19622,.T.);
#27182=ORIENTED_EDGE('',*,*,#19329,.F.);
#27183=ORIENTED_EDGE('',*,*,#19622,.F.);
#27184=ORIENTED_EDGE('',*,*,#19623,.F.);
#27185=ORIENTED_EDGE('',*,*,#19624,.F.);
#27186=ORIENTED_EDGE('',*,*,#19327,.F.);
#27187=ORIENTED_EDGE('',*,*,#19625,.F.);
#27188=ORIENTED_EDGE('',*,*,#19626,.F.);
#27189=ORIENTED_EDGE('',*,*,#19620,.T.);
#27190=ORIENTED_EDGE('',*,*,#19332,.F.);
#27191=ORIENTED_EDGE('',*,*,#19627,.F.);
#27192=ORIENTED_EDGE('',*,*,#19628,.F.);
#27193=ORIENTED_EDGE('',*,*,#19629,.T.);
#27194=ORIENTED_EDGE('',*,*,#19333,.F.);
#27195=ORIENTED_EDGE('',*,*,#19629,.F.);
#27196=ORIENTED_EDGE('',*,*,#19630,.F.);
#27197=ORIENTED_EDGE('',*,*,#19631,.F.);
#27198=ORIENTED_EDGE('',*,*,#19331,.F.);
#27199=ORIENTED_EDGE('',*,*,#19632,.F.);
#27200=ORIENTED_EDGE('',*,*,#19633,.F.);
#27201=ORIENTED_EDGE('',*,*,#19627,.T.);
#27202=ORIENTED_EDGE('',*,*,#19336,.F.);
#27203=ORIENTED_EDGE('',*,*,#19634,.F.);
#27204=ORIENTED_EDGE('',*,*,#19635,.F.);
#27205=ORIENTED_EDGE('',*,*,#19636,.T.);
#27206=ORIENTED_EDGE('',*,*,#19337,.F.);
#27207=ORIENTED_EDGE('',*,*,#19636,.F.);
#27208=ORIENTED_EDGE('',*,*,#19637,.F.);
#27209=ORIENTED_EDGE('',*,*,#19638,.F.);
#27210=ORIENTED_EDGE('',*,*,#19335,.F.);
#27211=ORIENTED_EDGE('',*,*,#19639,.F.);
#27212=ORIENTED_EDGE('',*,*,#19640,.F.);
#27213=ORIENTED_EDGE('',*,*,#19634,.T.);
#27214=ORIENTED_EDGE('',*,*,#19340,.F.);
#27215=ORIENTED_EDGE('',*,*,#19641,.F.);
#27216=ORIENTED_EDGE('',*,*,#19642,.F.);
#27217=ORIENTED_EDGE('',*,*,#19643,.T.);
#27218=ORIENTED_EDGE('',*,*,#19341,.F.);
#27219=ORIENTED_EDGE('',*,*,#19643,.F.);
#27220=ORIENTED_EDGE('',*,*,#19644,.F.);
#27221=ORIENTED_EDGE('',*,*,#19645,.F.);
#27222=ORIENTED_EDGE('',*,*,#19339,.F.);
#27223=ORIENTED_EDGE('',*,*,#19646,.F.);
#27224=ORIENTED_EDGE('',*,*,#19647,.F.);
#27225=ORIENTED_EDGE('',*,*,#19641,.T.);
#27226=ORIENTED_EDGE('',*,*,#19344,.F.);
#27227=ORIENTED_EDGE('',*,*,#19648,.F.);
#27228=ORIENTED_EDGE('',*,*,#19649,.F.);
#27229=ORIENTED_EDGE('',*,*,#19650,.T.);
#27230=ORIENTED_EDGE('',*,*,#19345,.F.);
#27231=ORIENTED_EDGE('',*,*,#19650,.F.);
#27232=ORIENTED_EDGE('',*,*,#19651,.F.);
#27233=ORIENTED_EDGE('',*,*,#19652,.F.);
#27234=ORIENTED_EDGE('',*,*,#19343,.F.);
#27235=ORIENTED_EDGE('',*,*,#19653,.F.);
#27236=ORIENTED_EDGE('',*,*,#19654,.F.);
#27237=ORIENTED_EDGE('',*,*,#19648,.T.);
#27238=ORIENTED_EDGE('',*,*,#19348,.F.);
#27239=ORIENTED_EDGE('',*,*,#19655,.F.);
#27240=ORIENTED_EDGE('',*,*,#19656,.F.);
#27241=ORIENTED_EDGE('',*,*,#19657,.T.);
#27242=ORIENTED_EDGE('',*,*,#19349,.F.);
#27243=ORIENTED_EDGE('',*,*,#19657,.F.);
#27244=ORIENTED_EDGE('',*,*,#19658,.F.);
#27245=ORIENTED_EDGE('',*,*,#19659,.F.);
#27246=ORIENTED_EDGE('',*,*,#19347,.F.);
#27247=ORIENTED_EDGE('',*,*,#19660,.F.);
#27248=ORIENTED_EDGE('',*,*,#19661,.F.);
#27249=ORIENTED_EDGE('',*,*,#19655,.T.);
#27250=ORIENTED_EDGE('',*,*,#19352,.F.);
#27251=ORIENTED_EDGE('',*,*,#19662,.F.);
#27252=ORIENTED_EDGE('',*,*,#19663,.F.);
#27253=ORIENTED_EDGE('',*,*,#19664,.T.);
#27254=ORIENTED_EDGE('',*,*,#19353,.F.);
#27255=ORIENTED_EDGE('',*,*,#19664,.F.);
#27256=ORIENTED_EDGE('',*,*,#19665,.F.);
#27257=ORIENTED_EDGE('',*,*,#19666,.F.);
#27258=ORIENTED_EDGE('',*,*,#19351,.F.);
#27259=ORIENTED_EDGE('',*,*,#19667,.F.);
#27260=ORIENTED_EDGE('',*,*,#19668,.F.);
#27261=ORIENTED_EDGE('',*,*,#19662,.T.);
#27262=ORIENTED_EDGE('',*,*,#19356,.F.);
#27263=ORIENTED_EDGE('',*,*,#19669,.F.);
#27264=ORIENTED_EDGE('',*,*,#19670,.F.);
#27265=ORIENTED_EDGE('',*,*,#19671,.T.);
#27266=ORIENTED_EDGE('',*,*,#19357,.F.);
#27267=ORIENTED_EDGE('',*,*,#19671,.F.);
#27268=ORIENTED_EDGE('',*,*,#19672,.F.);
#27269=ORIENTED_EDGE('',*,*,#19673,.F.);
#27270=ORIENTED_EDGE('',*,*,#19355,.F.);
#27271=ORIENTED_EDGE('',*,*,#19674,.F.);
#27272=ORIENTED_EDGE('',*,*,#19675,.F.);
#27273=ORIENTED_EDGE('',*,*,#19669,.T.);
#27274=ORIENTED_EDGE('',*,*,#19360,.F.);
#27275=ORIENTED_EDGE('',*,*,#19676,.F.);
#27276=ORIENTED_EDGE('',*,*,#19677,.F.);
#27277=ORIENTED_EDGE('',*,*,#19678,.T.);
#27278=ORIENTED_EDGE('',*,*,#19361,.F.);
#27279=ORIENTED_EDGE('',*,*,#19678,.F.);
#27280=ORIENTED_EDGE('',*,*,#19679,.F.);
#27281=ORIENTED_EDGE('',*,*,#19680,.F.);
#27282=ORIENTED_EDGE('',*,*,#19359,.F.);
#27283=ORIENTED_EDGE('',*,*,#19681,.F.);
#27284=ORIENTED_EDGE('',*,*,#19682,.F.);
#27285=ORIENTED_EDGE('',*,*,#19676,.T.);
#27286=ORIENTED_EDGE('',*,*,#19364,.F.);
#27287=ORIENTED_EDGE('',*,*,#19683,.F.);
#27288=ORIENTED_EDGE('',*,*,#19684,.F.);
#27289=ORIENTED_EDGE('',*,*,#19685,.T.);
#27290=ORIENTED_EDGE('',*,*,#19365,.F.);
#27291=ORIENTED_EDGE('',*,*,#19685,.F.);
#27292=ORIENTED_EDGE('',*,*,#19686,.F.);
#27293=ORIENTED_EDGE('',*,*,#19687,.F.);
#27294=ORIENTED_EDGE('',*,*,#19363,.F.);
#27295=ORIENTED_EDGE('',*,*,#19688,.F.);
#27296=ORIENTED_EDGE('',*,*,#19689,.F.);
#27297=ORIENTED_EDGE('',*,*,#19683,.T.);
#27298=ORIENTED_EDGE('',*,*,#19368,.F.);
#27299=ORIENTED_EDGE('',*,*,#19690,.F.);
#27300=ORIENTED_EDGE('',*,*,#19691,.F.);
#27301=ORIENTED_EDGE('',*,*,#19692,.T.);
#27302=ORIENTED_EDGE('',*,*,#19369,.F.);
#27303=ORIENTED_EDGE('',*,*,#19692,.F.);
#27304=ORIENTED_EDGE('',*,*,#19693,.F.);
#27305=ORIENTED_EDGE('',*,*,#19694,.F.);
#27306=ORIENTED_EDGE('',*,*,#19367,.F.);
#27307=ORIENTED_EDGE('',*,*,#19695,.F.);
#27308=ORIENTED_EDGE('',*,*,#19696,.F.);
#27309=ORIENTED_EDGE('',*,*,#19690,.T.);
#27310=ORIENTED_EDGE('',*,*,#19372,.F.);
#27311=ORIENTED_EDGE('',*,*,#19697,.F.);
#27312=ORIENTED_EDGE('',*,*,#19698,.F.);
#27313=ORIENTED_EDGE('',*,*,#19699,.T.);
#27314=ORIENTED_EDGE('',*,*,#19373,.F.);
#27315=ORIENTED_EDGE('',*,*,#19699,.F.);
#27316=ORIENTED_EDGE('',*,*,#19700,.F.);
#27317=ORIENTED_EDGE('',*,*,#19701,.F.);
#27318=ORIENTED_EDGE('',*,*,#19371,.F.);
#27319=ORIENTED_EDGE('',*,*,#19702,.F.);
#27320=ORIENTED_EDGE('',*,*,#19703,.F.);
#27321=ORIENTED_EDGE('',*,*,#19697,.T.);
#27322=ORIENTED_EDGE('',*,*,#19376,.F.);
#27323=ORIENTED_EDGE('',*,*,#19704,.F.);
#27324=ORIENTED_EDGE('',*,*,#19705,.F.);
#27325=ORIENTED_EDGE('',*,*,#19706,.T.);
#27326=ORIENTED_EDGE('',*,*,#19377,.F.);
#27327=ORIENTED_EDGE('',*,*,#19706,.F.);
#27328=ORIENTED_EDGE('',*,*,#19707,.F.);
#27329=ORIENTED_EDGE('',*,*,#19708,.F.);
#27330=ORIENTED_EDGE('',*,*,#19375,.F.);
#27331=ORIENTED_EDGE('',*,*,#19709,.F.);
#27332=ORIENTED_EDGE('',*,*,#19710,.F.);
#27333=ORIENTED_EDGE('',*,*,#19704,.T.);
#27334=ORIENTED_EDGE('',*,*,#19380,.F.);
#27335=ORIENTED_EDGE('',*,*,#19711,.F.);
#27336=ORIENTED_EDGE('',*,*,#19712,.F.);
#27337=ORIENTED_EDGE('',*,*,#19713,.T.);
#27338=ORIENTED_EDGE('',*,*,#19381,.F.);
#27339=ORIENTED_EDGE('',*,*,#19713,.F.);
#27340=ORIENTED_EDGE('',*,*,#19714,.F.);
#27341=ORIENTED_EDGE('',*,*,#19715,.F.);
#27342=ORIENTED_EDGE('',*,*,#19379,.F.);
#27343=ORIENTED_EDGE('',*,*,#19716,.F.);
#27344=ORIENTED_EDGE('',*,*,#19717,.F.);
#27345=ORIENTED_EDGE('',*,*,#19711,.T.);
#27346=ORIENTED_EDGE('',*,*,#19384,.F.);
#27347=ORIENTED_EDGE('',*,*,#19718,.F.);
#27348=ORIENTED_EDGE('',*,*,#19719,.F.);
#27349=ORIENTED_EDGE('',*,*,#19720,.T.);
#27350=ORIENTED_EDGE('',*,*,#19385,.F.);
#27351=ORIENTED_EDGE('',*,*,#19720,.F.);
#27352=ORIENTED_EDGE('',*,*,#19721,.F.);
#27353=ORIENTED_EDGE('',*,*,#19722,.F.);
#27354=ORIENTED_EDGE('',*,*,#19383,.F.);
#27355=ORIENTED_EDGE('',*,*,#19723,.F.);
#27356=ORIENTED_EDGE('',*,*,#19724,.F.);
#27357=ORIENTED_EDGE('',*,*,#19718,.T.);
#27358=ORIENTED_EDGE('',*,*,#19388,.F.);
#27359=ORIENTED_EDGE('',*,*,#19725,.F.);
#27360=ORIENTED_EDGE('',*,*,#19726,.F.);
#27361=ORIENTED_EDGE('',*,*,#19727,.T.);
#27362=ORIENTED_EDGE('',*,*,#19389,.F.);
#27363=ORIENTED_EDGE('',*,*,#19727,.F.);
#27364=ORIENTED_EDGE('',*,*,#19728,.F.);
#27365=ORIENTED_EDGE('',*,*,#19729,.F.);
#27366=ORIENTED_EDGE('',*,*,#19387,.F.);
#27367=ORIENTED_EDGE('',*,*,#19730,.F.);
#27368=ORIENTED_EDGE('',*,*,#19731,.F.);
#27369=ORIENTED_EDGE('',*,*,#19725,.T.);
#27370=ORIENTED_EDGE('',*,*,#19729,.T.);
#27371=ORIENTED_EDGE('',*,*,#19732,.F.);
#27372=ORIENTED_EDGE('',*,*,#19733,.T.);
#27373=ORIENTED_EDGE('',*,*,#19390,.T.);
#27374=ORIENTED_EDGE('',*,*,#19722,.T.);
#27375=ORIENTED_EDGE('',*,*,#19734,.F.);
#27376=ORIENTED_EDGE('',*,*,#19730,.T.);
#27377=ORIENTED_EDGE('',*,*,#19386,.T.);
#27378=ORIENTED_EDGE('',*,*,#19715,.T.);
#27379=ORIENTED_EDGE('',*,*,#19735,.F.);
#27380=ORIENTED_EDGE('',*,*,#19723,.T.);
#27381=ORIENTED_EDGE('',*,*,#19382,.T.);
#27382=ORIENTED_EDGE('',*,*,#19708,.T.);
#27383=ORIENTED_EDGE('',*,*,#19736,.F.);
#27384=ORIENTED_EDGE('',*,*,#19716,.T.);
#27385=ORIENTED_EDGE('',*,*,#19378,.T.);
#27386=ORIENTED_EDGE('',*,*,#19701,.T.);
#27387=ORIENTED_EDGE('',*,*,#19737,.F.);
#27388=ORIENTED_EDGE('',*,*,#19709,.T.);
#27389=ORIENTED_EDGE('',*,*,#19374,.T.);
#27390=ORIENTED_EDGE('',*,*,#19694,.T.);
#27391=ORIENTED_EDGE('',*,*,#19738,.F.);
#27392=ORIENTED_EDGE('',*,*,#19702,.T.);
#27393=ORIENTED_EDGE('',*,*,#19370,.T.);
#27394=ORIENTED_EDGE('',*,*,#19687,.T.);
#27395=ORIENTED_EDGE('',*,*,#19739,.F.);
#27396=ORIENTED_EDGE('',*,*,#19695,.T.);
#27397=ORIENTED_EDGE('',*,*,#19366,.T.);
#27398=ORIENTED_EDGE('',*,*,#19680,.T.);
#27399=ORIENTED_EDGE('',*,*,#19740,.F.);
#27400=ORIENTED_EDGE('',*,*,#19688,.T.);
#27401=ORIENTED_EDGE('',*,*,#19362,.T.);
#27402=ORIENTED_EDGE('',*,*,#19673,.T.);
#27403=ORIENTED_EDGE('',*,*,#19741,.F.);
#27404=ORIENTED_EDGE('',*,*,#19681,.T.);
#27405=ORIENTED_EDGE('',*,*,#19358,.T.);
#27406=ORIENTED_EDGE('',*,*,#19666,.T.);
#27407=ORIENTED_EDGE('',*,*,#19742,.F.);
#27408=ORIENTED_EDGE('',*,*,#19674,.T.);
#27409=ORIENTED_EDGE('',*,*,#19354,.T.);
#27410=ORIENTED_EDGE('',*,*,#19659,.T.);
#27411=ORIENTED_EDGE('',*,*,#19743,.F.);
#27412=ORIENTED_EDGE('',*,*,#19667,.T.);
#27413=ORIENTED_EDGE('',*,*,#19350,.T.);
#27414=ORIENTED_EDGE('',*,*,#19652,.T.);
#27415=ORIENTED_EDGE('',*,*,#19744,.F.);
#27416=ORIENTED_EDGE('',*,*,#19660,.T.);
#27417=ORIENTED_EDGE('',*,*,#19346,.T.);
#27418=ORIENTED_EDGE('',*,*,#19645,.T.);
#27419=ORIENTED_EDGE('',*,*,#19745,.F.);
#27420=ORIENTED_EDGE('',*,*,#19653,.T.);
#27421=ORIENTED_EDGE('',*,*,#19342,.T.);
#27422=ORIENTED_EDGE('',*,*,#19638,.T.);
#27423=ORIENTED_EDGE('',*,*,#19746,.F.);
#27424=ORIENTED_EDGE('',*,*,#19646,.T.);
#27425=ORIENTED_EDGE('',*,*,#19338,.T.);
#27426=ORIENTED_EDGE('',*,*,#19631,.T.);
#27427=ORIENTED_EDGE('',*,*,#19747,.F.);
#27428=ORIENTED_EDGE('',*,*,#19639,.T.);
#27429=ORIENTED_EDGE('',*,*,#19334,.T.);
#27430=ORIENTED_EDGE('',*,*,#19624,.T.);
#27431=ORIENTED_EDGE('',*,*,#19748,.F.);
#27432=ORIENTED_EDGE('',*,*,#19632,.T.);
#27433=ORIENTED_EDGE('',*,*,#19330,.T.);
#27434=ORIENTED_EDGE('',*,*,#19617,.T.);
#27435=ORIENTED_EDGE('',*,*,#19749,.F.);
#27436=ORIENTED_EDGE('',*,*,#19625,.T.);
#27437=ORIENTED_EDGE('',*,*,#19326,.T.);
#27438=ORIENTED_EDGE('',*,*,#19610,.T.);
#27439=ORIENTED_EDGE('',*,*,#19750,.F.);
#27440=ORIENTED_EDGE('',*,*,#19618,.T.);
#27441=ORIENTED_EDGE('',*,*,#19322,.T.);
#27442=ORIENTED_EDGE('',*,*,#19603,.T.);
#27443=ORIENTED_EDGE('',*,*,#19751,.F.);
#27444=ORIENTED_EDGE('',*,*,#19611,.T.);
#27445=ORIENTED_EDGE('',*,*,#19318,.T.);
#27446=ORIENTED_EDGE('',*,*,#19596,.T.);
#27447=ORIENTED_EDGE('',*,*,#19752,.F.);
#27448=ORIENTED_EDGE('',*,*,#19604,.T.);
#27449=ORIENTED_EDGE('',*,*,#19314,.T.);
#27450=ORIENTED_EDGE('',*,*,#19589,.T.);
#27451=ORIENTED_EDGE('',*,*,#19753,.F.);
#27452=ORIENTED_EDGE('',*,*,#19597,.T.);
#27453=ORIENTED_EDGE('',*,*,#19310,.T.);
#27454=ORIENTED_EDGE('',*,*,#19582,.T.);
#27455=ORIENTED_EDGE('',*,*,#19754,.F.);
#27456=ORIENTED_EDGE('',*,*,#19590,.T.);
#27457=ORIENTED_EDGE('',*,*,#19306,.T.);
#27458=ORIENTED_EDGE('',*,*,#19575,.T.);
#27459=ORIENTED_EDGE('',*,*,#19755,.F.);
#27460=ORIENTED_EDGE('',*,*,#19583,.T.);
#27461=ORIENTED_EDGE('',*,*,#19302,.T.);
#27462=ORIENTED_EDGE('',*,*,#19568,.T.);
#27463=ORIENTED_EDGE('',*,*,#19756,.F.);
#27464=ORIENTED_EDGE('',*,*,#19576,.T.);
#27465=ORIENTED_EDGE('',*,*,#19298,.T.);
#27466=ORIENTED_EDGE('',*,*,#19561,.T.);
#27467=ORIENTED_EDGE('',*,*,#19757,.F.);
#27468=ORIENTED_EDGE('',*,*,#19569,.T.);
#27469=ORIENTED_EDGE('',*,*,#19294,.T.);
#27470=ORIENTED_EDGE('',*,*,#19554,.T.);
#27471=ORIENTED_EDGE('',*,*,#19758,.F.);
#27472=ORIENTED_EDGE('',*,*,#19562,.T.);
#27473=ORIENTED_EDGE('',*,*,#19290,.T.);
#27474=ORIENTED_EDGE('',*,*,#19547,.T.);
#27475=ORIENTED_EDGE('',*,*,#19759,.F.);
#27476=ORIENTED_EDGE('',*,*,#19555,.T.);
#27477=ORIENTED_EDGE('',*,*,#19286,.T.);
#27478=ORIENTED_EDGE('',*,*,#19540,.T.);
#27479=ORIENTED_EDGE('',*,*,#19760,.F.);
#27480=ORIENTED_EDGE('',*,*,#19548,.T.);
#27481=ORIENTED_EDGE('',*,*,#19282,.T.);
#27482=ORIENTED_EDGE('',*,*,#19533,.T.);
#27483=ORIENTED_EDGE('',*,*,#19761,.F.);
#27484=ORIENTED_EDGE('',*,*,#19541,.T.);
#27485=ORIENTED_EDGE('',*,*,#19278,.T.);
#27486=ORIENTED_EDGE('',*,*,#19526,.T.);
#27487=ORIENTED_EDGE('',*,*,#19762,.F.);
#27488=ORIENTED_EDGE('',*,*,#19534,.T.);
#27489=ORIENTED_EDGE('',*,*,#19274,.T.);
#27490=ORIENTED_EDGE('',*,*,#19519,.T.);
#27491=ORIENTED_EDGE('',*,*,#19763,.F.);
#27492=ORIENTED_EDGE('',*,*,#19527,.T.);
#27493=ORIENTED_EDGE('',*,*,#19270,.T.);
#27494=ORIENTED_EDGE('',*,*,#19512,.T.);
#27495=ORIENTED_EDGE('',*,*,#19764,.F.);
#27496=ORIENTED_EDGE('',*,*,#19520,.T.);
#27497=ORIENTED_EDGE('',*,*,#19266,.T.);
#27498=ORIENTED_EDGE('',*,*,#19505,.T.);
#27499=ORIENTED_EDGE('',*,*,#19765,.F.);
#27500=ORIENTED_EDGE('',*,*,#19513,.T.);
#27501=ORIENTED_EDGE('',*,*,#19262,.T.);
#27502=ORIENTED_EDGE('',*,*,#19498,.T.);
#27503=ORIENTED_EDGE('',*,*,#19766,.F.);
#27504=ORIENTED_EDGE('',*,*,#19506,.T.);
#27505=ORIENTED_EDGE('',*,*,#19258,.T.);
#27506=ORIENTED_EDGE('',*,*,#19491,.T.);
#27507=ORIENTED_EDGE('',*,*,#19767,.F.);
#27508=ORIENTED_EDGE('',*,*,#19499,.T.);
#27509=ORIENTED_EDGE('',*,*,#19254,.T.);
#27510=ORIENTED_EDGE('',*,*,#19484,.T.);
#27511=ORIENTED_EDGE('',*,*,#19768,.F.);
#27512=ORIENTED_EDGE('',*,*,#19492,.T.);
#27513=ORIENTED_EDGE('',*,*,#19250,.T.);
#27514=ORIENTED_EDGE('',*,*,#19477,.T.);
#27515=ORIENTED_EDGE('',*,*,#19769,.F.);
#27516=ORIENTED_EDGE('',*,*,#19485,.T.);
#27517=ORIENTED_EDGE('',*,*,#19246,.T.);
#27518=ORIENTED_EDGE('',*,*,#19470,.T.);
#27519=ORIENTED_EDGE('',*,*,#19770,.F.);
#27520=ORIENTED_EDGE('',*,*,#19478,.T.);
#27521=ORIENTED_EDGE('',*,*,#19242,.T.);
#27522=ORIENTED_EDGE('',*,*,#19463,.T.);
#27523=ORIENTED_EDGE('',*,*,#19771,.F.);
#27524=ORIENTED_EDGE('',*,*,#19471,.T.);
#27525=ORIENTED_EDGE('',*,*,#19238,.T.);
#27526=ORIENTED_EDGE('',*,*,#19456,.T.);
#27527=ORIENTED_EDGE('',*,*,#19772,.F.);
#27528=ORIENTED_EDGE('',*,*,#19464,.T.);
#27529=ORIENTED_EDGE('',*,*,#19234,.T.);
#27530=ORIENTED_EDGE('',*,*,#19449,.T.);
#27531=ORIENTED_EDGE('',*,*,#19773,.F.);
#27532=ORIENTED_EDGE('',*,*,#19457,.T.);
#27533=ORIENTED_EDGE('',*,*,#19230,.T.);
#27534=ORIENTED_EDGE('',*,*,#19442,.T.);
#27535=ORIENTED_EDGE('',*,*,#19774,.F.);
#27536=ORIENTED_EDGE('',*,*,#19450,.T.);
#27537=ORIENTED_EDGE('',*,*,#19226,.T.);
#27538=ORIENTED_EDGE('',*,*,#19435,.T.);
#27539=ORIENTED_EDGE('',*,*,#19775,.F.);
#27540=ORIENTED_EDGE('',*,*,#19443,.T.);
#27541=ORIENTED_EDGE('',*,*,#19222,.T.);
#27542=ORIENTED_EDGE('',*,*,#19428,.T.);
#27543=ORIENTED_EDGE('',*,*,#19776,.F.);
#27544=ORIENTED_EDGE('',*,*,#19436,.T.);
#27545=ORIENTED_EDGE('',*,*,#19218,.T.);
#27546=ORIENTED_EDGE('',*,*,#19421,.T.);
#27547=ORIENTED_EDGE('',*,*,#19777,.F.);
#27548=ORIENTED_EDGE('',*,*,#19429,.T.);
#27549=ORIENTED_EDGE('',*,*,#19214,.T.);
#27550=ORIENTED_EDGE('',*,*,#19414,.T.);
#27551=ORIENTED_EDGE('',*,*,#19778,.F.);
#27552=ORIENTED_EDGE('',*,*,#19422,.T.);
#27553=ORIENTED_EDGE('',*,*,#19210,.T.);
#27554=ORIENTED_EDGE('',*,*,#19407,.T.);
#27555=ORIENTED_EDGE('',*,*,#19779,.F.);
#27556=ORIENTED_EDGE('',*,*,#19415,.T.);
#27557=ORIENTED_EDGE('',*,*,#19206,.T.);
#27558=ORIENTED_EDGE('',*,*,#19392,.F.);
#27559=ORIENTED_EDGE('',*,*,#19780,.F.);
#27560=ORIENTED_EDGE('',*,*,#19781,.F.);
#27561=ORIENTED_EDGE('',*,*,#19782,.T.);
#27562=ORIENTED_EDGE('',*,*,#19393,.F.);
#27563=ORIENTED_EDGE('',*,*,#19782,.F.);
#27564=ORIENTED_EDGE('',*,*,#19783,.F.);
#27565=ORIENTED_EDGE('',*,*,#19784,.F.);
#27566=ORIENTED_EDGE('',*,*,#19391,.F.);
#27567=ORIENTED_EDGE('',*,*,#19733,.F.);
#27568=ORIENTED_EDGE('',*,*,#19785,.F.);
#27569=ORIENTED_EDGE('',*,*,#19780,.T.);
#27570=ORIENTED_EDGE('',*,*,#19408,.T.);
#27571=ORIENTED_EDGE('',*,*,#19394,.T.);
#27572=ORIENTED_EDGE('',*,*,#19784,.T.);
#27573=ORIENTED_EDGE('',*,*,#19786,.F.);
#27574=ORIENTED_EDGE('',*,*,#19409,.T.);
#27575=ORIENTED_EDGE('',*,*,#19786,.T.);
#27576=ORIENTED_EDGE('',*,*,#19783,.T.);
#27577=ORIENTED_EDGE('',*,*,#19781,.T.);
#27578=ORIENTED_EDGE('',*,*,#19785,.T.);
#27579=ORIENTED_EDGE('',*,*,#19732,.T.);
#27580=ORIENTED_EDGE('',*,*,#19728,.T.);
#27581=ORIENTED_EDGE('',*,*,#19726,.T.);
#27582=ORIENTED_EDGE('',*,*,#19731,.T.);
#27583=ORIENTED_EDGE('',*,*,#19734,.T.);
#27584=ORIENTED_EDGE('',*,*,#19721,.T.);
#27585=ORIENTED_EDGE('',*,*,#19719,.T.);
#27586=ORIENTED_EDGE('',*,*,#19724,.T.);
#27587=ORIENTED_EDGE('',*,*,#19735,.T.);
#27588=ORIENTED_EDGE('',*,*,#19714,.T.);
#27589=ORIENTED_EDGE('',*,*,#19712,.T.);
#27590=ORIENTED_EDGE('',*,*,#19717,.T.);
#27591=ORIENTED_EDGE('',*,*,#19736,.T.);
#27592=ORIENTED_EDGE('',*,*,#19707,.T.);
#27593=ORIENTED_EDGE('',*,*,#19705,.T.);
#27594=ORIENTED_EDGE('',*,*,#19710,.T.);
#27595=ORIENTED_EDGE('',*,*,#19737,.T.);
#27596=ORIENTED_EDGE('',*,*,#19700,.T.);
#27597=ORIENTED_EDGE('',*,*,#19698,.T.);
#27598=ORIENTED_EDGE('',*,*,#19703,.T.);
#27599=ORIENTED_EDGE('',*,*,#19738,.T.);
#27600=ORIENTED_EDGE('',*,*,#19693,.T.);
#27601=ORIENTED_EDGE('',*,*,#19691,.T.);
#27602=ORIENTED_EDGE('',*,*,#19696,.T.);
#27603=ORIENTED_EDGE('',*,*,#19739,.T.);
#27604=ORIENTED_EDGE('',*,*,#19686,.T.);
#27605=ORIENTED_EDGE('',*,*,#19684,.T.);
#27606=ORIENTED_EDGE('',*,*,#19689,.T.);
#27607=ORIENTED_EDGE('',*,*,#19740,.T.);
#27608=ORIENTED_EDGE('',*,*,#19679,.T.);
#27609=ORIENTED_EDGE('',*,*,#19677,.T.);
#27610=ORIENTED_EDGE('',*,*,#19682,.T.);
#27611=ORIENTED_EDGE('',*,*,#19741,.T.);
#27612=ORIENTED_EDGE('',*,*,#19672,.T.);
#27613=ORIENTED_EDGE('',*,*,#19670,.T.);
#27614=ORIENTED_EDGE('',*,*,#19675,.T.);
#27615=ORIENTED_EDGE('',*,*,#19742,.T.);
#27616=ORIENTED_EDGE('',*,*,#19665,.T.);
#27617=ORIENTED_EDGE('',*,*,#19663,.T.);
#27618=ORIENTED_EDGE('',*,*,#19668,.T.);
#27619=ORIENTED_EDGE('',*,*,#19743,.T.);
#27620=ORIENTED_EDGE('',*,*,#19658,.T.);
#27621=ORIENTED_EDGE('',*,*,#19656,.T.);
#27622=ORIENTED_EDGE('',*,*,#19661,.T.);
#27623=ORIENTED_EDGE('',*,*,#19744,.T.);
#27624=ORIENTED_EDGE('',*,*,#19651,.T.);
#27625=ORIENTED_EDGE('',*,*,#19649,.T.);
#27626=ORIENTED_EDGE('',*,*,#19654,.T.);
#27627=ORIENTED_EDGE('',*,*,#19745,.T.);
#27628=ORIENTED_EDGE('',*,*,#19644,.T.);
#27629=ORIENTED_EDGE('',*,*,#19642,.T.);
#27630=ORIENTED_EDGE('',*,*,#19647,.T.);
#27631=ORIENTED_EDGE('',*,*,#19746,.T.);
#27632=ORIENTED_EDGE('',*,*,#19637,.T.);
#27633=ORIENTED_EDGE('',*,*,#19635,.T.);
#27634=ORIENTED_EDGE('',*,*,#19640,.T.);
#27635=ORIENTED_EDGE('',*,*,#19747,.T.);
#27636=ORIENTED_EDGE('',*,*,#19630,.T.);
#27637=ORIENTED_EDGE('',*,*,#19628,.T.);
#27638=ORIENTED_EDGE('',*,*,#19633,.T.);
#27639=ORIENTED_EDGE('',*,*,#19748,.T.);
#27640=ORIENTED_EDGE('',*,*,#19623,.T.);
#27641=ORIENTED_EDGE('',*,*,#19621,.T.);
#27642=ORIENTED_EDGE('',*,*,#19626,.T.);
#27643=ORIENTED_EDGE('',*,*,#19749,.T.);
#27644=ORIENTED_EDGE('',*,*,#19616,.T.);
#27645=ORIENTED_EDGE('',*,*,#19614,.T.);
#27646=ORIENTED_EDGE('',*,*,#19619,.T.);
#27647=ORIENTED_EDGE('',*,*,#19750,.T.);
#27648=ORIENTED_EDGE('',*,*,#19609,.T.);
#27649=ORIENTED_EDGE('',*,*,#19607,.T.);
#27650=ORIENTED_EDGE('',*,*,#19612,.T.);
#27651=ORIENTED_EDGE('',*,*,#19751,.T.);
#27652=ORIENTED_EDGE('',*,*,#19602,.T.);
#27653=ORIENTED_EDGE('',*,*,#19600,.T.);
#27654=ORIENTED_EDGE('',*,*,#19605,.T.);
#27655=ORIENTED_EDGE('',*,*,#19752,.T.);
#27656=ORIENTED_EDGE('',*,*,#19595,.T.);
#27657=ORIENTED_EDGE('',*,*,#19593,.T.);
#27658=ORIENTED_EDGE('',*,*,#19598,.T.);
#27659=ORIENTED_EDGE('',*,*,#19753,.T.);
#27660=ORIENTED_EDGE('',*,*,#19588,.T.);
#27661=ORIENTED_EDGE('',*,*,#19586,.T.);
#27662=ORIENTED_EDGE('',*,*,#19591,.T.);
#27663=ORIENTED_EDGE('',*,*,#19754,.T.);
#27664=ORIENTED_EDGE('',*,*,#19581,.T.);
#27665=ORIENTED_EDGE('',*,*,#19579,.T.);
#27666=ORIENTED_EDGE('',*,*,#19584,.T.);
#27667=ORIENTED_EDGE('',*,*,#19755,.T.);
#27668=ORIENTED_EDGE('',*,*,#19574,.T.);
#27669=ORIENTED_EDGE('',*,*,#19572,.T.);
#27670=ORIENTED_EDGE('',*,*,#19577,.T.);
#27671=ORIENTED_EDGE('',*,*,#19756,.T.);
#27672=ORIENTED_EDGE('',*,*,#19567,.T.);
#27673=ORIENTED_EDGE('',*,*,#19565,.T.);
#27674=ORIENTED_EDGE('',*,*,#19570,.T.);
#27675=ORIENTED_EDGE('',*,*,#19757,.T.);
#27676=ORIENTED_EDGE('',*,*,#19560,.T.);
#27677=ORIENTED_EDGE('',*,*,#19558,.T.);
#27678=ORIENTED_EDGE('',*,*,#19563,.T.);
#27679=ORIENTED_EDGE('',*,*,#19758,.T.);
#27680=ORIENTED_EDGE('',*,*,#19553,.T.);
#27681=ORIENTED_EDGE('',*,*,#19551,.T.);
#27682=ORIENTED_EDGE('',*,*,#19556,.T.);
#27683=ORIENTED_EDGE('',*,*,#19759,.T.);
#27684=ORIENTED_EDGE('',*,*,#19546,.T.);
#27685=ORIENTED_EDGE('',*,*,#19544,.T.);
#27686=ORIENTED_EDGE('',*,*,#19549,.T.);
#27687=ORIENTED_EDGE('',*,*,#19760,.T.);
#27688=ORIENTED_EDGE('',*,*,#19539,.T.);
#27689=ORIENTED_EDGE('',*,*,#19537,.T.);
#27690=ORIENTED_EDGE('',*,*,#19542,.T.);
#27691=ORIENTED_EDGE('',*,*,#19761,.T.);
#27692=ORIENTED_EDGE('',*,*,#19532,.T.);
#27693=ORIENTED_EDGE('',*,*,#19530,.T.);
#27694=ORIENTED_EDGE('',*,*,#19535,.T.);
#27695=ORIENTED_EDGE('',*,*,#19762,.T.);
#27696=ORIENTED_EDGE('',*,*,#19525,.T.);
#27697=ORIENTED_EDGE('',*,*,#19523,.T.);
#27698=ORIENTED_EDGE('',*,*,#19528,.T.);
#27699=ORIENTED_EDGE('',*,*,#19763,.T.);
#27700=ORIENTED_EDGE('',*,*,#19518,.T.);
#27701=ORIENTED_EDGE('',*,*,#19516,.T.);
#27702=ORIENTED_EDGE('',*,*,#19521,.T.);
#27703=ORIENTED_EDGE('',*,*,#19764,.T.);
#27704=ORIENTED_EDGE('',*,*,#19511,.T.);
#27705=ORIENTED_EDGE('',*,*,#19509,.T.);
#27706=ORIENTED_EDGE('',*,*,#19514,.T.);
#27707=ORIENTED_EDGE('',*,*,#19765,.T.);
#27708=ORIENTED_EDGE('',*,*,#19504,.T.);
#27709=ORIENTED_EDGE('',*,*,#19502,.T.);
#27710=ORIENTED_EDGE('',*,*,#19507,.T.);
#27711=ORIENTED_EDGE('',*,*,#19766,.T.);
#27712=ORIENTED_EDGE('',*,*,#19497,.T.);
#27713=ORIENTED_EDGE('',*,*,#19495,.T.);
#27714=ORIENTED_EDGE('',*,*,#19500,.T.);
#27715=ORIENTED_EDGE('',*,*,#19767,.T.);
#27716=ORIENTED_EDGE('',*,*,#19490,.T.);
#27717=ORIENTED_EDGE('',*,*,#19488,.T.);
#27718=ORIENTED_EDGE('',*,*,#19493,.T.);
#27719=ORIENTED_EDGE('',*,*,#19768,.T.);
#27720=ORIENTED_EDGE('',*,*,#19483,.T.);
#27721=ORIENTED_EDGE('',*,*,#19481,.T.);
#27722=ORIENTED_EDGE('',*,*,#19486,.T.);
#27723=ORIENTED_EDGE('',*,*,#19769,.T.);
#27724=ORIENTED_EDGE('',*,*,#19476,.T.);
#27725=ORIENTED_EDGE('',*,*,#19474,.T.);
#27726=ORIENTED_EDGE('',*,*,#19479,.T.);
#27727=ORIENTED_EDGE('',*,*,#19770,.T.);
#27728=ORIENTED_EDGE('',*,*,#19469,.T.);
#27729=ORIENTED_EDGE('',*,*,#19467,.T.);
#27730=ORIENTED_EDGE('',*,*,#19472,.T.);
#27731=ORIENTED_EDGE('',*,*,#19771,.T.);
#27732=ORIENTED_EDGE('',*,*,#19462,.T.);
#27733=ORIENTED_EDGE('',*,*,#19460,.T.);
#27734=ORIENTED_EDGE('',*,*,#19465,.T.);
#27735=ORIENTED_EDGE('',*,*,#19772,.T.);
#27736=ORIENTED_EDGE('',*,*,#19455,.T.);
#27737=ORIENTED_EDGE('',*,*,#19453,.T.);
#27738=ORIENTED_EDGE('',*,*,#19458,.T.);
#27739=ORIENTED_EDGE('',*,*,#19773,.T.);
#27740=ORIENTED_EDGE('',*,*,#19448,.T.);
#27741=ORIENTED_EDGE('',*,*,#19446,.T.);
#27742=ORIENTED_EDGE('',*,*,#19451,.T.);
#27743=ORIENTED_EDGE('',*,*,#19774,.T.);
#27744=ORIENTED_EDGE('',*,*,#19441,.T.);
#27745=ORIENTED_EDGE('',*,*,#19439,.T.);
#27746=ORIENTED_EDGE('',*,*,#19444,.T.);
#27747=ORIENTED_EDGE('',*,*,#19775,.T.);
#27748=ORIENTED_EDGE('',*,*,#19434,.T.);
#27749=ORIENTED_EDGE('',*,*,#19432,.T.);
#27750=ORIENTED_EDGE('',*,*,#19437,.T.);
#27751=ORIENTED_EDGE('',*,*,#19776,.T.);
#27752=ORIENTED_EDGE('',*,*,#19427,.T.);
#27753=ORIENTED_EDGE('',*,*,#19425,.T.);
#27754=ORIENTED_EDGE('',*,*,#19430,.T.);
#27755=ORIENTED_EDGE('',*,*,#19777,.T.);
#27756=ORIENTED_EDGE('',*,*,#19420,.T.);
#27757=ORIENTED_EDGE('',*,*,#19418,.T.);
#27758=ORIENTED_EDGE('',*,*,#19423,.T.);
#27759=ORIENTED_EDGE('',*,*,#19778,.T.);
#27760=ORIENTED_EDGE('',*,*,#19413,.T.);
#27761=ORIENTED_EDGE('',*,*,#19411,.T.);
#27762=ORIENTED_EDGE('',*,*,#19416,.T.);
#27763=ORIENTED_EDGE('',*,*,#19779,.T.);
#27764=ORIENTED_EDGE('',*,*,#19406,.T.);
#27765=ORIENTED_EDGE('',*,*,#19404,.T.);
#27766=ORIENTED_EDGE('',*,*,#19400,.T.);
#27767=ORIENTED_EDGE('',*,*,#19402,.T.);
#27768=ORIENTED_EDGE('',*,*,#19395,.T.);
#27769=ORIENTED_EDGE('',*,*,#19398,.T.);
#27770=ORIENTED_EDGE('',*,*,#19787,.T.);
#27771=ORIENTED_EDGE('',*,*,#19788,.T.);
#27772=ORIENTED_EDGE('',*,*,#19789,.T.);
#27773=ORIENTED_EDGE('',*,*,#19790,.T.);
#27774=ORIENTED_EDGE('',*,*,#19788,.F.);
#27775=ORIENTED_EDGE('',*,*,#19790,.F.);
#27776=ORIENTED_EDGE('',*,*,#19791,.T.);
#27777=ORIENTED_EDGE('',*,*,#19792,.F.);
#27778=ORIENTED_EDGE('',*,*,#19791,.F.);
#27779=ORIENTED_EDGE('',*,*,#19789,.F.);
#27780=ORIENTED_EDGE('',*,*,#19787,.F.);
#27781=ORIENTED_EDGE('',*,*,#19793,.T.);
#27782=ORIENTED_EDGE('',*,*,#19794,.T.);
#27783=ORIENTED_EDGE('',*,*,#19795,.T.);
#27784=ORIENTED_EDGE('',*,*,#19796,.T.);
#27785=ORIENTED_EDGE('',*,*,#19797,.T.);
#27786=ORIENTED_EDGE('',*,*,#19798,.T.);
#27787=ORIENTED_EDGE('',*,*,#19792,.T.);
#27788=ORIENTED_EDGE('',*,*,#19798,.F.);
#27789=ORIENTED_EDGE('',*,*,#19799,.T.);
#27790=ORIENTED_EDGE('',*,*,#19800,.T.);
#27791=ORIENTED_EDGE('',*,*,#19801,.T.);
#27792=ORIENTED_EDGE('',*,*,#19802,.F.);
#27793=ORIENTED_EDGE('',*,*,#19803,.T.);
#27794=ORIENTED_EDGE('',*,*,#19804,.T.);
#27795=ORIENTED_EDGE('',*,*,#19805,.T.);
#27796=ORIENTED_EDGE('',*,*,#19806,.F.);
#27797=ORIENTED_EDGE('',*,*,#19807,.T.);
#27798=ORIENTED_EDGE('',*,*,#19808,.T.);
#27799=ORIENTED_EDGE('',*,*,#19809,.T.);
#27800=ORIENTED_EDGE('',*,*,#19810,.F.);
#27801=ORIENTED_EDGE('',*,*,#19811,.T.);
#27802=ORIENTED_EDGE('',*,*,#19812,.T.);
#27803=ORIENTED_EDGE('',*,*,#19813,.T.);
#27804=ORIENTED_EDGE('',*,*,#19814,.F.);
#27805=ORIENTED_EDGE('',*,*,#19815,.T.);
#27806=ORIENTED_EDGE('',*,*,#19816,.T.);
#27807=ORIENTED_EDGE('',*,*,#19817,.T.);
#27808=ORIENTED_EDGE('',*,*,#19818,.F.);
#27809=ORIENTED_EDGE('',*,*,#19819,.T.);
#27810=ORIENTED_EDGE('',*,*,#19820,.T.);
#27811=ORIENTED_EDGE('',*,*,#19821,.T.);
#27812=ORIENTED_EDGE('',*,*,#19822,.F.);
#27813=ORIENTED_EDGE('',*,*,#19823,.T.);
#27814=ORIENTED_EDGE('',*,*,#19824,.T.);
#27815=ORIENTED_EDGE('',*,*,#19825,.T.);
#27816=ORIENTED_EDGE('',*,*,#19826,.F.);
#27817=ORIENTED_EDGE('',*,*,#19827,.T.);
#27818=ORIENTED_EDGE('',*,*,#19828,.T.);
#27819=ORIENTED_EDGE('',*,*,#19829,.T.);
#27820=ORIENTED_EDGE('',*,*,#19830,.F.);
#27821=ORIENTED_EDGE('',*,*,#19831,.T.);
#27822=ORIENTED_EDGE('',*,*,#19832,.T.);
#27823=ORIENTED_EDGE('',*,*,#19833,.T.);
#27824=ORIENTED_EDGE('',*,*,#19834,.F.);
#27825=ORIENTED_EDGE('',*,*,#19835,.T.);
#27826=ORIENTED_EDGE('',*,*,#19836,.T.);
#27827=ORIENTED_EDGE('',*,*,#19837,.T.);
#27828=ORIENTED_EDGE('',*,*,#19838,.F.);
#27829=ORIENTED_EDGE('',*,*,#19839,.T.);
#27830=ORIENTED_EDGE('',*,*,#19840,.T.);
#27831=ORIENTED_EDGE('',*,*,#19841,.T.);
#27832=ORIENTED_EDGE('',*,*,#19842,.F.);
#27833=ORIENTED_EDGE('',*,*,#19843,.T.);
#27834=ORIENTED_EDGE('',*,*,#19844,.T.);
#27835=ORIENTED_EDGE('',*,*,#19845,.T.);
#27836=ORIENTED_EDGE('',*,*,#19846,.F.);
#27837=ORIENTED_EDGE('',*,*,#19847,.T.);
#27838=ORIENTED_EDGE('',*,*,#19848,.T.);
#27839=ORIENTED_EDGE('',*,*,#19849,.T.);
#27840=ORIENTED_EDGE('',*,*,#19850,.F.);
#27841=ORIENTED_EDGE('',*,*,#19851,.T.);
#27842=ORIENTED_EDGE('',*,*,#19852,.T.);
#27843=ORIENTED_EDGE('',*,*,#19853,.T.);
#27844=ORIENTED_EDGE('',*,*,#19854,.F.);
#27845=ORIENTED_EDGE('',*,*,#19855,.T.);
#27846=ORIENTED_EDGE('',*,*,#19856,.T.);
#27847=ORIENTED_EDGE('',*,*,#19857,.T.);
#27848=ORIENTED_EDGE('',*,*,#19858,.F.);
#27849=ORIENTED_EDGE('',*,*,#19859,.T.);
#27850=ORIENTED_EDGE('',*,*,#19860,.T.);
#27851=ORIENTED_EDGE('',*,*,#19861,.T.);
#27852=ORIENTED_EDGE('',*,*,#19862,.F.);
#27853=ORIENTED_EDGE('',*,*,#19863,.T.);
#27854=ORIENTED_EDGE('',*,*,#19864,.T.);
#27855=ORIENTED_EDGE('',*,*,#19865,.T.);
#27856=ORIENTED_EDGE('',*,*,#19866,.F.);
#27857=ORIENTED_EDGE('',*,*,#19867,.T.);
#27858=ORIENTED_EDGE('',*,*,#19868,.T.);
#27859=ORIENTED_EDGE('',*,*,#19869,.T.);
#27860=ORIENTED_EDGE('',*,*,#19870,.F.);
#27861=ORIENTED_EDGE('',*,*,#19871,.T.);
#27862=ORIENTED_EDGE('',*,*,#19872,.T.);
#27863=ORIENTED_EDGE('',*,*,#19873,.T.);
#27864=ORIENTED_EDGE('',*,*,#19874,.F.);
#27865=ORIENTED_EDGE('',*,*,#19875,.T.);
#27866=ORIENTED_EDGE('',*,*,#19876,.T.);
#27867=ORIENTED_EDGE('',*,*,#19877,.T.);
#27868=ORIENTED_EDGE('',*,*,#19878,.F.);
#27869=ORIENTED_EDGE('',*,*,#19879,.T.);
#27870=ORIENTED_EDGE('',*,*,#19880,.T.);
#27871=ORIENTED_EDGE('',*,*,#19881,.T.);
#27872=ORIENTED_EDGE('',*,*,#19882,.F.);
#27873=ORIENTED_EDGE('',*,*,#19883,.T.);
#27874=ORIENTED_EDGE('',*,*,#19884,.T.);
#27875=ORIENTED_EDGE('',*,*,#19885,.T.);
#27876=ORIENTED_EDGE('',*,*,#19886,.F.);
#27877=ORIENTED_EDGE('',*,*,#19887,.T.);
#27878=ORIENTED_EDGE('',*,*,#19888,.T.);
#27879=ORIENTED_EDGE('',*,*,#19889,.T.);
#27880=ORIENTED_EDGE('',*,*,#19890,.F.);
#27881=ORIENTED_EDGE('',*,*,#19891,.T.);
#27882=ORIENTED_EDGE('',*,*,#19892,.T.);
#27883=ORIENTED_EDGE('',*,*,#19893,.T.);
#27884=ORIENTED_EDGE('',*,*,#19894,.F.);
#27885=ORIENTED_EDGE('',*,*,#19895,.T.);
#27886=ORIENTED_EDGE('',*,*,#19896,.T.);
#27887=ORIENTED_EDGE('',*,*,#19897,.T.);
#27888=ORIENTED_EDGE('',*,*,#19898,.F.);
#27889=ORIENTED_EDGE('',*,*,#19899,.T.);
#27890=ORIENTED_EDGE('',*,*,#19900,.T.);
#27891=ORIENTED_EDGE('',*,*,#19901,.T.);
#27892=ORIENTED_EDGE('',*,*,#19902,.F.);
#27893=ORIENTED_EDGE('',*,*,#19903,.T.);
#27894=ORIENTED_EDGE('',*,*,#19904,.T.);
#27895=ORIENTED_EDGE('',*,*,#19905,.T.);
#27896=ORIENTED_EDGE('',*,*,#19906,.F.);
#27897=ORIENTED_EDGE('',*,*,#19907,.T.);
#27898=ORIENTED_EDGE('',*,*,#19908,.T.);
#27899=ORIENTED_EDGE('',*,*,#19909,.T.);
#27900=ORIENTED_EDGE('',*,*,#19910,.F.);
#27901=ORIENTED_EDGE('',*,*,#19911,.T.);
#27902=ORIENTED_EDGE('',*,*,#19912,.T.);
#27903=ORIENTED_EDGE('',*,*,#19913,.T.);
#27904=ORIENTED_EDGE('',*,*,#19914,.F.);
#27905=ORIENTED_EDGE('',*,*,#19915,.T.);
#27906=ORIENTED_EDGE('',*,*,#19916,.T.);
#27907=ORIENTED_EDGE('',*,*,#19917,.T.);
#27908=ORIENTED_EDGE('',*,*,#19918,.F.);
#27909=ORIENTED_EDGE('',*,*,#19919,.T.);
#27910=ORIENTED_EDGE('',*,*,#19920,.T.);
#27911=ORIENTED_EDGE('',*,*,#19921,.T.);
#27912=ORIENTED_EDGE('',*,*,#19922,.F.);
#27913=ORIENTED_EDGE('',*,*,#19923,.T.);
#27914=ORIENTED_EDGE('',*,*,#19924,.T.);
#27915=ORIENTED_EDGE('',*,*,#19925,.T.);
#27916=ORIENTED_EDGE('',*,*,#19926,.F.);
#27917=ORIENTED_EDGE('',*,*,#19927,.T.);
#27918=ORIENTED_EDGE('',*,*,#19928,.T.);
#27919=ORIENTED_EDGE('',*,*,#19929,.T.);
#27920=ORIENTED_EDGE('',*,*,#19930,.F.);
#27921=ORIENTED_EDGE('',*,*,#19931,.T.);
#27922=ORIENTED_EDGE('',*,*,#19932,.T.);
#27923=ORIENTED_EDGE('',*,*,#19933,.T.);
#27924=ORIENTED_EDGE('',*,*,#19934,.F.);
#27925=ORIENTED_EDGE('',*,*,#19935,.T.);
#27926=ORIENTED_EDGE('',*,*,#19936,.T.);
#27927=ORIENTED_EDGE('',*,*,#19937,.T.);
#27928=ORIENTED_EDGE('',*,*,#19938,.F.);
#27929=ORIENTED_EDGE('',*,*,#19939,.T.);
#27930=ORIENTED_EDGE('',*,*,#19940,.T.);
#27931=ORIENTED_EDGE('',*,*,#19941,.T.);
#27932=ORIENTED_EDGE('',*,*,#19942,.F.);
#27933=ORIENTED_EDGE('',*,*,#19943,.T.);
#27934=ORIENTED_EDGE('',*,*,#19944,.T.);
#27935=ORIENTED_EDGE('',*,*,#19945,.T.);
#27936=ORIENTED_EDGE('',*,*,#19946,.F.);
#27937=ORIENTED_EDGE('',*,*,#19947,.T.);
#27938=ORIENTED_EDGE('',*,*,#19948,.T.);
#27939=ORIENTED_EDGE('',*,*,#19949,.T.);
#27940=ORIENTED_EDGE('',*,*,#19950,.F.);
#27941=ORIENTED_EDGE('',*,*,#19951,.T.);
#27942=ORIENTED_EDGE('',*,*,#19952,.T.);
#27943=ORIENTED_EDGE('',*,*,#19953,.T.);
#27944=ORIENTED_EDGE('',*,*,#19954,.F.);
#27945=ORIENTED_EDGE('',*,*,#19955,.T.);
#27946=ORIENTED_EDGE('',*,*,#19956,.T.);
#27947=ORIENTED_EDGE('',*,*,#19957,.T.);
#27948=ORIENTED_EDGE('',*,*,#19958,.F.);
#27949=ORIENTED_EDGE('',*,*,#19797,.F.);
#27950=ORIENTED_EDGE('',*,*,#19959,.F.);
#27951=ORIENTED_EDGE('',*,*,#19960,.F.);
#27952=ORIENTED_EDGE('',*,*,#19794,.F.);
#27953=ORIENTED_EDGE('',*,*,#19961,.T.);
#27954=ORIENTED_EDGE('',*,*,#19962,.F.);
#27955=ORIENTED_EDGE('',*,*,#19961,.F.);
#27956=ORIENTED_EDGE('',*,*,#19793,.F.);
#27957=ORIENTED_EDGE('',*,*,#19963,.F.);
#27958=ORIENTED_EDGE('',*,*,#19964,.F.);
#27959=ORIENTED_EDGE('',*,*,#19963,.T.);
#27960=ORIENTED_EDGE('',*,*,#19796,.F.);
#27961=ORIENTED_EDGE('',*,*,#19965,.T.);
#27962=ORIENTED_EDGE('',*,*,#19966,.F.);
#27963=ORIENTED_EDGE('',*,*,#19965,.F.);
#27964=ORIENTED_EDGE('',*,*,#19795,.F.);
#27965=ORIENTED_EDGE('',*,*,#19960,.T.);
#27966=ORIENTED_EDGE('',*,*,#19800,.F.);
#27967=ORIENTED_EDGE('',*,*,#19967,.F.);
#27968=ORIENTED_EDGE('',*,*,#19968,.F.);
#27969=ORIENTED_EDGE('',*,*,#19969,.T.);
#27970=ORIENTED_EDGE('',*,*,#19801,.F.);
#27971=ORIENTED_EDGE('',*,*,#19969,.F.);
#27972=ORIENTED_EDGE('',*,*,#19970,.F.);
#27973=ORIENTED_EDGE('',*,*,#19971,.F.);
#27974=ORIENTED_EDGE('',*,*,#19799,.F.);
#27975=ORIENTED_EDGE('',*,*,#19972,.F.);
#27976=ORIENTED_EDGE('',*,*,#19973,.F.);
#27977=ORIENTED_EDGE('',*,*,#19967,.T.);
#27978=ORIENTED_EDGE('',*,*,#19804,.F.);
#27979=ORIENTED_EDGE('',*,*,#19974,.F.);
#27980=ORIENTED_EDGE('',*,*,#19975,.F.);
#27981=ORIENTED_EDGE('',*,*,#19976,.T.);
#27982=ORIENTED_EDGE('',*,*,#19805,.F.);
#27983=ORIENTED_EDGE('',*,*,#19976,.F.);
#27984=ORIENTED_EDGE('',*,*,#19977,.F.);
#27985=ORIENTED_EDGE('',*,*,#19978,.F.);
#27986=ORIENTED_EDGE('',*,*,#19803,.F.);
#27987=ORIENTED_EDGE('',*,*,#19979,.F.);
#27988=ORIENTED_EDGE('',*,*,#19980,.F.);
#27989=ORIENTED_EDGE('',*,*,#19974,.T.);
#27990=ORIENTED_EDGE('',*,*,#19808,.F.);
#27991=ORIENTED_EDGE('',*,*,#19981,.F.);
#27992=ORIENTED_EDGE('',*,*,#19982,.F.);
#27993=ORIENTED_EDGE('',*,*,#19983,.T.);
#27994=ORIENTED_EDGE('',*,*,#19809,.F.);
#27995=ORIENTED_EDGE('',*,*,#19983,.F.);
#27996=ORIENTED_EDGE('',*,*,#19984,.F.);
#27997=ORIENTED_EDGE('',*,*,#19985,.F.);
#27998=ORIENTED_EDGE('',*,*,#19807,.F.);
#27999=ORIENTED_EDGE('',*,*,#19986,.F.);
#28000=ORIENTED_EDGE('',*,*,#19987,.F.);
#28001=ORIENTED_EDGE('',*,*,#19981,.T.);
#28002=ORIENTED_EDGE('',*,*,#19812,.F.);
#28003=ORIENTED_EDGE('',*,*,#19988,.F.);
#28004=ORIENTED_EDGE('',*,*,#19989,.F.);
#28005=ORIENTED_EDGE('',*,*,#19990,.T.);
#28006=ORIENTED_EDGE('',*,*,#19813,.F.);
#28007=ORIENTED_EDGE('',*,*,#19990,.F.);
#28008=ORIENTED_EDGE('',*,*,#19991,.F.);
#28009=ORIENTED_EDGE('',*,*,#19992,.F.);
#28010=ORIENTED_EDGE('',*,*,#19811,.F.);
#28011=ORIENTED_EDGE('',*,*,#19993,.F.);
#28012=ORIENTED_EDGE('',*,*,#19994,.F.);
#28013=ORIENTED_EDGE('',*,*,#19988,.T.);
#28014=ORIENTED_EDGE('',*,*,#19816,.F.);
#28015=ORIENTED_EDGE('',*,*,#19995,.F.);
#28016=ORIENTED_EDGE('',*,*,#19996,.F.);
#28017=ORIENTED_EDGE('',*,*,#19997,.T.);
#28018=ORIENTED_EDGE('',*,*,#19817,.F.);
#28019=ORIENTED_EDGE('',*,*,#19997,.F.);
#28020=ORIENTED_EDGE('',*,*,#19998,.F.);
#28021=ORIENTED_EDGE('',*,*,#19999,.F.);
#28022=ORIENTED_EDGE('',*,*,#19815,.F.);
#28023=ORIENTED_EDGE('',*,*,#20000,.F.);
#28024=ORIENTED_EDGE('',*,*,#20001,.F.);
#28025=ORIENTED_EDGE('',*,*,#19995,.T.);
#28026=ORIENTED_EDGE('',*,*,#19820,.F.);
#28027=ORIENTED_EDGE('',*,*,#20002,.F.);
#28028=ORIENTED_EDGE('',*,*,#20003,.F.);
#28029=ORIENTED_EDGE('',*,*,#20004,.T.);
#28030=ORIENTED_EDGE('',*,*,#19821,.F.);
#28031=ORIENTED_EDGE('',*,*,#20004,.F.);
#28032=ORIENTED_EDGE('',*,*,#20005,.F.);
#28033=ORIENTED_EDGE('',*,*,#20006,.F.);
#28034=ORIENTED_EDGE('',*,*,#19819,.F.);
#28035=ORIENTED_EDGE('',*,*,#20007,.F.);
#28036=ORIENTED_EDGE('',*,*,#20008,.F.);
#28037=ORIENTED_EDGE('',*,*,#20002,.T.);
#28038=ORIENTED_EDGE('',*,*,#19824,.F.);
#28039=ORIENTED_EDGE('',*,*,#20009,.F.);
#28040=ORIENTED_EDGE('',*,*,#20010,.F.);
#28041=ORIENTED_EDGE('',*,*,#20011,.T.);
#28042=ORIENTED_EDGE('',*,*,#19825,.F.);
#28043=ORIENTED_EDGE('',*,*,#20011,.F.);
#28044=ORIENTED_EDGE('',*,*,#20012,.F.);
#28045=ORIENTED_EDGE('',*,*,#20013,.F.);
#28046=ORIENTED_EDGE('',*,*,#19823,.F.);
#28047=ORIENTED_EDGE('',*,*,#20014,.F.);
#28048=ORIENTED_EDGE('',*,*,#20015,.F.);
#28049=ORIENTED_EDGE('',*,*,#20009,.T.);
#28050=ORIENTED_EDGE('',*,*,#19828,.F.);
#28051=ORIENTED_EDGE('',*,*,#20016,.F.);
#28052=ORIENTED_EDGE('',*,*,#20017,.F.);
#28053=ORIENTED_EDGE('',*,*,#20018,.T.);
#28054=ORIENTED_EDGE('',*,*,#19829,.F.);
#28055=ORIENTED_EDGE('',*,*,#20018,.F.);
#28056=ORIENTED_EDGE('',*,*,#20019,.F.);
#28057=ORIENTED_EDGE('',*,*,#20020,.F.);
#28058=ORIENTED_EDGE('',*,*,#19827,.F.);
#28059=ORIENTED_EDGE('',*,*,#20021,.F.);
#28060=ORIENTED_EDGE('',*,*,#20022,.F.);
#28061=ORIENTED_EDGE('',*,*,#20016,.T.);
#28062=ORIENTED_EDGE('',*,*,#19832,.F.);
#28063=ORIENTED_EDGE('',*,*,#20023,.F.);
#28064=ORIENTED_EDGE('',*,*,#20024,.F.);
#28065=ORIENTED_EDGE('',*,*,#20025,.T.);
#28066=ORIENTED_EDGE('',*,*,#19833,.F.);
#28067=ORIENTED_EDGE('',*,*,#20025,.F.);
#28068=ORIENTED_EDGE('',*,*,#20026,.F.);
#28069=ORIENTED_EDGE('',*,*,#20027,.F.);
#28070=ORIENTED_EDGE('',*,*,#19831,.F.);
#28071=ORIENTED_EDGE('',*,*,#20028,.F.);
#28072=ORIENTED_EDGE('',*,*,#20029,.F.);
#28073=ORIENTED_EDGE('',*,*,#20023,.T.);
#28074=ORIENTED_EDGE('',*,*,#19836,.F.);
#28075=ORIENTED_EDGE('',*,*,#20030,.F.);
#28076=ORIENTED_EDGE('',*,*,#20031,.F.);
#28077=ORIENTED_EDGE('',*,*,#20032,.T.);
#28078=ORIENTED_EDGE('',*,*,#19837,.F.);
#28079=ORIENTED_EDGE('',*,*,#20032,.F.);
#28080=ORIENTED_EDGE('',*,*,#20033,.F.);
#28081=ORIENTED_EDGE('',*,*,#20034,.F.);
#28082=ORIENTED_EDGE('',*,*,#19835,.F.);
#28083=ORIENTED_EDGE('',*,*,#20035,.F.);
#28084=ORIENTED_EDGE('',*,*,#20036,.F.);
#28085=ORIENTED_EDGE('',*,*,#20030,.T.);
#28086=ORIENTED_EDGE('',*,*,#19840,.F.);
#28087=ORIENTED_EDGE('',*,*,#20037,.F.);
#28088=ORIENTED_EDGE('',*,*,#20038,.F.);
#28089=ORIENTED_EDGE('',*,*,#20039,.T.);
#28090=ORIENTED_EDGE('',*,*,#19841,.F.);
#28091=ORIENTED_EDGE('',*,*,#20039,.F.);
#28092=ORIENTED_EDGE('',*,*,#20040,.F.);
#28093=ORIENTED_EDGE('',*,*,#20041,.F.);
#28094=ORIENTED_EDGE('',*,*,#19839,.F.);
#28095=ORIENTED_EDGE('',*,*,#20042,.F.);
#28096=ORIENTED_EDGE('',*,*,#20043,.F.);
#28097=ORIENTED_EDGE('',*,*,#20037,.T.);
#28098=ORIENTED_EDGE('',*,*,#19844,.F.);
#28099=ORIENTED_EDGE('',*,*,#20044,.F.);
#28100=ORIENTED_EDGE('',*,*,#20045,.F.);
#28101=ORIENTED_EDGE('',*,*,#20046,.T.);
#28102=ORIENTED_EDGE('',*,*,#19845,.F.);
#28103=ORIENTED_EDGE('',*,*,#20046,.F.);
#28104=ORIENTED_EDGE('',*,*,#20047,.F.);
#28105=ORIENTED_EDGE('',*,*,#20048,.F.);
#28106=ORIENTED_EDGE('',*,*,#19843,.F.);
#28107=ORIENTED_EDGE('',*,*,#20049,.F.);
#28108=ORIENTED_EDGE('',*,*,#20050,.F.);
#28109=ORIENTED_EDGE('',*,*,#20044,.T.);
#28110=ORIENTED_EDGE('',*,*,#19848,.F.);
#28111=ORIENTED_EDGE('',*,*,#20051,.F.);
#28112=ORIENTED_EDGE('',*,*,#20052,.F.);
#28113=ORIENTED_EDGE('',*,*,#20053,.T.);
#28114=ORIENTED_EDGE('',*,*,#19849,.F.);
#28115=ORIENTED_EDGE('',*,*,#20053,.F.);
#28116=ORIENTED_EDGE('',*,*,#20054,.F.);
#28117=ORIENTED_EDGE('',*,*,#20055,.F.);
#28118=ORIENTED_EDGE('',*,*,#19847,.F.);
#28119=ORIENTED_EDGE('',*,*,#20056,.F.);
#28120=ORIENTED_EDGE('',*,*,#20057,.F.);
#28121=ORIENTED_EDGE('',*,*,#20051,.T.);
#28122=ORIENTED_EDGE('',*,*,#19852,.F.);
#28123=ORIENTED_EDGE('',*,*,#20058,.F.);
#28124=ORIENTED_EDGE('',*,*,#20059,.F.);
#28125=ORIENTED_EDGE('',*,*,#20060,.T.);
#28126=ORIENTED_EDGE('',*,*,#19853,.F.);
#28127=ORIENTED_EDGE('',*,*,#20060,.F.);
#28128=ORIENTED_EDGE('',*,*,#20061,.F.);
#28129=ORIENTED_EDGE('',*,*,#20062,.F.);
#28130=ORIENTED_EDGE('',*,*,#19851,.F.);
#28131=ORIENTED_EDGE('',*,*,#20063,.F.);
#28132=ORIENTED_EDGE('',*,*,#20064,.F.);
#28133=ORIENTED_EDGE('',*,*,#20058,.T.);
#28134=ORIENTED_EDGE('',*,*,#19856,.F.);
#28135=ORIENTED_EDGE('',*,*,#20065,.F.);
#28136=ORIENTED_EDGE('',*,*,#20066,.F.);
#28137=ORIENTED_EDGE('',*,*,#20067,.T.);
#28138=ORIENTED_EDGE('',*,*,#19857,.F.);
#28139=ORIENTED_EDGE('',*,*,#20067,.F.);
#28140=ORIENTED_EDGE('',*,*,#20068,.F.);
#28141=ORIENTED_EDGE('',*,*,#20069,.F.);
#28142=ORIENTED_EDGE('',*,*,#19855,.F.);
#28143=ORIENTED_EDGE('',*,*,#20070,.F.);
#28144=ORIENTED_EDGE('',*,*,#20071,.F.);
#28145=ORIENTED_EDGE('',*,*,#20065,.T.);
#28146=ORIENTED_EDGE('',*,*,#19860,.F.);
#28147=ORIENTED_EDGE('',*,*,#20072,.F.);
#28148=ORIENTED_EDGE('',*,*,#20073,.F.);
#28149=ORIENTED_EDGE('',*,*,#20074,.T.);
#28150=ORIENTED_EDGE('',*,*,#19861,.F.);
#28151=ORIENTED_EDGE('',*,*,#20074,.F.);
#28152=ORIENTED_EDGE('',*,*,#20075,.F.);
#28153=ORIENTED_EDGE('',*,*,#20076,.F.);
#28154=ORIENTED_EDGE('',*,*,#19859,.F.);
#28155=ORIENTED_EDGE('',*,*,#20077,.F.);
#28156=ORIENTED_EDGE('',*,*,#20078,.F.);
#28157=ORIENTED_EDGE('',*,*,#20072,.T.);
#28158=ORIENTED_EDGE('',*,*,#19864,.F.);
#28159=ORIENTED_EDGE('',*,*,#20079,.F.);
#28160=ORIENTED_EDGE('',*,*,#20080,.F.);
#28161=ORIENTED_EDGE('',*,*,#20081,.T.);
#28162=ORIENTED_EDGE('',*,*,#19865,.F.);
#28163=ORIENTED_EDGE('',*,*,#20081,.F.);
#28164=ORIENTED_EDGE('',*,*,#20082,.F.);
#28165=ORIENTED_EDGE('',*,*,#20083,.F.);
#28166=ORIENTED_EDGE('',*,*,#19863,.F.);
#28167=ORIENTED_EDGE('',*,*,#20084,.F.);
#28168=ORIENTED_EDGE('',*,*,#20085,.F.);
#28169=ORIENTED_EDGE('',*,*,#20079,.T.);
#28170=ORIENTED_EDGE('',*,*,#19868,.F.);
#28171=ORIENTED_EDGE('',*,*,#20086,.F.);
#28172=ORIENTED_EDGE('',*,*,#20087,.F.);
#28173=ORIENTED_EDGE('',*,*,#20088,.T.);
#28174=ORIENTED_EDGE('',*,*,#19869,.F.);
#28175=ORIENTED_EDGE('',*,*,#20088,.F.);
#28176=ORIENTED_EDGE('',*,*,#20089,.F.);
#28177=ORIENTED_EDGE('',*,*,#20090,.F.);
#28178=ORIENTED_EDGE('',*,*,#19867,.F.);
#28179=ORIENTED_EDGE('',*,*,#20091,.F.);
#28180=ORIENTED_EDGE('',*,*,#20092,.F.);
#28181=ORIENTED_EDGE('',*,*,#20086,.T.);
#28182=ORIENTED_EDGE('',*,*,#19872,.F.);
#28183=ORIENTED_EDGE('',*,*,#20093,.F.);
#28184=ORIENTED_EDGE('',*,*,#20094,.F.);
#28185=ORIENTED_EDGE('',*,*,#20095,.T.);
#28186=ORIENTED_EDGE('',*,*,#19873,.F.);
#28187=ORIENTED_EDGE('',*,*,#20095,.F.);
#28188=ORIENTED_EDGE('',*,*,#20096,.F.);
#28189=ORIENTED_EDGE('',*,*,#20097,.F.);
#28190=ORIENTED_EDGE('',*,*,#19871,.F.);
#28191=ORIENTED_EDGE('',*,*,#20098,.F.);
#28192=ORIENTED_EDGE('',*,*,#20099,.F.);
#28193=ORIENTED_EDGE('',*,*,#20093,.T.);
#28194=ORIENTED_EDGE('',*,*,#19876,.F.);
#28195=ORIENTED_EDGE('',*,*,#20100,.F.);
#28196=ORIENTED_EDGE('',*,*,#20101,.F.);
#28197=ORIENTED_EDGE('',*,*,#20102,.T.);
#28198=ORIENTED_EDGE('',*,*,#19877,.F.);
#28199=ORIENTED_EDGE('',*,*,#20102,.F.);
#28200=ORIENTED_EDGE('',*,*,#20103,.F.);
#28201=ORIENTED_EDGE('',*,*,#20104,.F.);
#28202=ORIENTED_EDGE('',*,*,#19875,.F.);
#28203=ORIENTED_EDGE('',*,*,#20105,.F.);
#28204=ORIENTED_EDGE('',*,*,#20106,.F.);
#28205=ORIENTED_EDGE('',*,*,#20100,.T.);
#28206=ORIENTED_EDGE('',*,*,#19880,.F.);
#28207=ORIENTED_EDGE('',*,*,#20107,.F.);
#28208=ORIENTED_EDGE('',*,*,#20108,.F.);
#28209=ORIENTED_EDGE('',*,*,#20109,.T.);
#28210=ORIENTED_EDGE('',*,*,#19881,.F.);
#28211=ORIENTED_EDGE('',*,*,#20109,.F.);
#28212=ORIENTED_EDGE('',*,*,#20110,.F.);
#28213=ORIENTED_EDGE('',*,*,#20111,.F.);
#28214=ORIENTED_EDGE('',*,*,#19879,.F.);
#28215=ORIENTED_EDGE('',*,*,#20112,.F.);
#28216=ORIENTED_EDGE('',*,*,#20113,.F.);
#28217=ORIENTED_EDGE('',*,*,#20107,.T.);
#28218=ORIENTED_EDGE('',*,*,#19884,.F.);
#28219=ORIENTED_EDGE('',*,*,#20114,.F.);
#28220=ORIENTED_EDGE('',*,*,#20115,.F.);
#28221=ORIENTED_EDGE('',*,*,#20116,.T.);
#28222=ORIENTED_EDGE('',*,*,#19885,.F.);
#28223=ORIENTED_EDGE('',*,*,#20116,.F.);
#28224=ORIENTED_EDGE('',*,*,#20117,.F.);
#28225=ORIENTED_EDGE('',*,*,#20118,.F.);
#28226=ORIENTED_EDGE('',*,*,#19883,.F.);
#28227=ORIENTED_EDGE('',*,*,#20119,.F.);
#28228=ORIENTED_EDGE('',*,*,#20120,.F.);
#28229=ORIENTED_EDGE('',*,*,#20114,.T.);
#28230=ORIENTED_EDGE('',*,*,#19888,.F.);
#28231=ORIENTED_EDGE('',*,*,#20121,.F.);
#28232=ORIENTED_EDGE('',*,*,#20122,.F.);
#28233=ORIENTED_EDGE('',*,*,#20123,.T.);
#28234=ORIENTED_EDGE('',*,*,#19889,.F.);
#28235=ORIENTED_EDGE('',*,*,#20123,.F.);
#28236=ORIENTED_EDGE('',*,*,#20124,.F.);
#28237=ORIENTED_EDGE('',*,*,#20125,.F.);
#28238=ORIENTED_EDGE('',*,*,#19887,.F.);
#28239=ORIENTED_EDGE('',*,*,#20126,.F.);
#28240=ORIENTED_EDGE('',*,*,#20127,.F.);
#28241=ORIENTED_EDGE('',*,*,#20121,.T.);
#28242=ORIENTED_EDGE('',*,*,#19892,.F.);
#28243=ORIENTED_EDGE('',*,*,#20128,.F.);
#28244=ORIENTED_EDGE('',*,*,#20129,.F.);
#28245=ORIENTED_EDGE('',*,*,#20130,.T.);
#28246=ORIENTED_EDGE('',*,*,#19893,.F.);
#28247=ORIENTED_EDGE('',*,*,#20130,.F.);
#28248=ORIENTED_EDGE('',*,*,#20131,.F.);
#28249=ORIENTED_EDGE('',*,*,#20132,.F.);
#28250=ORIENTED_EDGE('',*,*,#19891,.F.);
#28251=ORIENTED_EDGE('',*,*,#20133,.F.);
#28252=ORIENTED_EDGE('',*,*,#20134,.F.);
#28253=ORIENTED_EDGE('',*,*,#20128,.T.);
#28254=ORIENTED_EDGE('',*,*,#19896,.F.);
#28255=ORIENTED_EDGE('',*,*,#20135,.F.);
#28256=ORIENTED_EDGE('',*,*,#20136,.F.);
#28257=ORIENTED_EDGE('',*,*,#20137,.T.);
#28258=ORIENTED_EDGE('',*,*,#19897,.F.);
#28259=ORIENTED_EDGE('',*,*,#20137,.F.);
#28260=ORIENTED_EDGE('',*,*,#20138,.F.);
#28261=ORIENTED_EDGE('',*,*,#20139,.F.);
#28262=ORIENTED_EDGE('',*,*,#19895,.F.);
#28263=ORIENTED_EDGE('',*,*,#20140,.F.);
#28264=ORIENTED_EDGE('',*,*,#20141,.F.);
#28265=ORIENTED_EDGE('',*,*,#20135,.T.);
#28266=ORIENTED_EDGE('',*,*,#19900,.F.);
#28267=ORIENTED_EDGE('',*,*,#20142,.F.);
#28268=ORIENTED_EDGE('',*,*,#20143,.F.);
#28269=ORIENTED_EDGE('',*,*,#20144,.T.);
#28270=ORIENTED_EDGE('',*,*,#19901,.F.);
#28271=ORIENTED_EDGE('',*,*,#20144,.F.);
#28272=ORIENTED_EDGE('',*,*,#20145,.F.);
#28273=ORIENTED_EDGE('',*,*,#20146,.F.);
#28274=ORIENTED_EDGE('',*,*,#19899,.F.);
#28275=ORIENTED_EDGE('',*,*,#20147,.F.);
#28276=ORIENTED_EDGE('',*,*,#20148,.F.);
#28277=ORIENTED_EDGE('',*,*,#20142,.T.);
#28278=ORIENTED_EDGE('',*,*,#19904,.F.);
#28279=ORIENTED_EDGE('',*,*,#20149,.F.);
#28280=ORIENTED_EDGE('',*,*,#20150,.F.);
#28281=ORIENTED_EDGE('',*,*,#20151,.T.);
#28282=ORIENTED_EDGE('',*,*,#19905,.F.);
#28283=ORIENTED_EDGE('',*,*,#20151,.F.);
#28284=ORIENTED_EDGE('',*,*,#20152,.F.);
#28285=ORIENTED_EDGE('',*,*,#20153,.F.);
#28286=ORIENTED_EDGE('',*,*,#19903,.F.);
#28287=ORIENTED_EDGE('',*,*,#20154,.F.);
#28288=ORIENTED_EDGE('',*,*,#20155,.F.);
#28289=ORIENTED_EDGE('',*,*,#20149,.T.);
#28290=ORIENTED_EDGE('',*,*,#19908,.F.);
#28291=ORIENTED_EDGE('',*,*,#20156,.F.);
#28292=ORIENTED_EDGE('',*,*,#20157,.F.);
#28293=ORIENTED_EDGE('',*,*,#20158,.T.);
#28294=ORIENTED_EDGE('',*,*,#19909,.F.);
#28295=ORIENTED_EDGE('',*,*,#20158,.F.);
#28296=ORIENTED_EDGE('',*,*,#20159,.F.);
#28297=ORIENTED_EDGE('',*,*,#20160,.F.);
#28298=ORIENTED_EDGE('',*,*,#19907,.F.);
#28299=ORIENTED_EDGE('',*,*,#20161,.F.);
#28300=ORIENTED_EDGE('',*,*,#20162,.F.);
#28301=ORIENTED_EDGE('',*,*,#20156,.T.);
#28302=ORIENTED_EDGE('',*,*,#19912,.F.);
#28303=ORIENTED_EDGE('',*,*,#20163,.F.);
#28304=ORIENTED_EDGE('',*,*,#20164,.F.);
#28305=ORIENTED_EDGE('',*,*,#20165,.T.);
#28306=ORIENTED_EDGE('',*,*,#19913,.F.);
#28307=ORIENTED_EDGE('',*,*,#20165,.F.);
#28308=ORIENTED_EDGE('',*,*,#20166,.F.);
#28309=ORIENTED_EDGE('',*,*,#20167,.F.);
#28310=ORIENTED_EDGE('',*,*,#19911,.F.);
#28311=ORIENTED_EDGE('',*,*,#20168,.F.);
#28312=ORIENTED_EDGE('',*,*,#20169,.F.);
#28313=ORIENTED_EDGE('',*,*,#20163,.T.);
#28314=ORIENTED_EDGE('',*,*,#19916,.F.);
#28315=ORIENTED_EDGE('',*,*,#20170,.F.);
#28316=ORIENTED_EDGE('',*,*,#20171,.F.);
#28317=ORIENTED_EDGE('',*,*,#20172,.T.);
#28318=ORIENTED_EDGE('',*,*,#19917,.F.);
#28319=ORIENTED_EDGE('',*,*,#20172,.F.);
#28320=ORIENTED_EDGE('',*,*,#20173,.F.);
#28321=ORIENTED_EDGE('',*,*,#20174,.F.);
#28322=ORIENTED_EDGE('',*,*,#19915,.F.);
#28323=ORIENTED_EDGE('',*,*,#20175,.F.);
#28324=ORIENTED_EDGE('',*,*,#20176,.F.);
#28325=ORIENTED_EDGE('',*,*,#20170,.T.);
#28326=ORIENTED_EDGE('',*,*,#19920,.F.);
#28327=ORIENTED_EDGE('',*,*,#20177,.F.);
#28328=ORIENTED_EDGE('',*,*,#20178,.F.);
#28329=ORIENTED_EDGE('',*,*,#20179,.T.);
#28330=ORIENTED_EDGE('',*,*,#19921,.F.);
#28331=ORIENTED_EDGE('',*,*,#20179,.F.);
#28332=ORIENTED_EDGE('',*,*,#20180,.F.);
#28333=ORIENTED_EDGE('',*,*,#20181,.F.);
#28334=ORIENTED_EDGE('',*,*,#19919,.F.);
#28335=ORIENTED_EDGE('',*,*,#20182,.F.);
#28336=ORIENTED_EDGE('',*,*,#20183,.F.);
#28337=ORIENTED_EDGE('',*,*,#20177,.T.);
#28338=ORIENTED_EDGE('',*,*,#19924,.F.);
#28339=ORIENTED_EDGE('',*,*,#20184,.F.);
#28340=ORIENTED_EDGE('',*,*,#20185,.F.);
#28341=ORIENTED_EDGE('',*,*,#20186,.T.);
#28342=ORIENTED_EDGE('',*,*,#19925,.F.);
#28343=ORIENTED_EDGE('',*,*,#20186,.F.);
#28344=ORIENTED_EDGE('',*,*,#20187,.F.);
#28345=ORIENTED_EDGE('',*,*,#20188,.F.);
#28346=ORIENTED_EDGE('',*,*,#19923,.F.);
#28347=ORIENTED_EDGE('',*,*,#20189,.F.);
#28348=ORIENTED_EDGE('',*,*,#20190,.F.);
#28349=ORIENTED_EDGE('',*,*,#20184,.T.);
#28350=ORIENTED_EDGE('',*,*,#19928,.F.);
#28351=ORIENTED_EDGE('',*,*,#20191,.F.);
#28352=ORIENTED_EDGE('',*,*,#20192,.F.);
#28353=ORIENTED_EDGE('',*,*,#20193,.T.);
#28354=ORIENTED_EDGE('',*,*,#19929,.F.);
#28355=ORIENTED_EDGE('',*,*,#20193,.F.);
#28356=ORIENTED_EDGE('',*,*,#20194,.F.);
#28357=ORIENTED_EDGE('',*,*,#20195,.F.);
#28358=ORIENTED_EDGE('',*,*,#19927,.F.);
#28359=ORIENTED_EDGE('',*,*,#20196,.F.);
#28360=ORIENTED_EDGE('',*,*,#20197,.F.);
#28361=ORIENTED_EDGE('',*,*,#20191,.T.);
#28362=ORIENTED_EDGE('',*,*,#19932,.F.);
#28363=ORIENTED_EDGE('',*,*,#20198,.F.);
#28364=ORIENTED_EDGE('',*,*,#20199,.F.);
#28365=ORIENTED_EDGE('',*,*,#20200,.T.);
#28366=ORIENTED_EDGE('',*,*,#19933,.F.);
#28367=ORIENTED_EDGE('',*,*,#20200,.F.);
#28368=ORIENTED_EDGE('',*,*,#20201,.F.);
#28369=ORIENTED_EDGE('',*,*,#20202,.F.);
#28370=ORIENTED_EDGE('',*,*,#19931,.F.);
#28371=ORIENTED_EDGE('',*,*,#20203,.F.);
#28372=ORIENTED_EDGE('',*,*,#20204,.F.);
#28373=ORIENTED_EDGE('',*,*,#20198,.T.);
#28374=ORIENTED_EDGE('',*,*,#19936,.F.);
#28375=ORIENTED_EDGE('',*,*,#20205,.F.);
#28376=ORIENTED_EDGE('',*,*,#20206,.F.);
#28377=ORIENTED_EDGE('',*,*,#20207,.T.);
#28378=ORIENTED_EDGE('',*,*,#19937,.F.);
#28379=ORIENTED_EDGE('',*,*,#20207,.F.);
#28380=ORIENTED_EDGE('',*,*,#20208,.F.);
#28381=ORIENTED_EDGE('',*,*,#20209,.F.);
#28382=ORIENTED_EDGE('',*,*,#19935,.F.);
#28383=ORIENTED_EDGE('',*,*,#20210,.F.);
#28384=ORIENTED_EDGE('',*,*,#20211,.F.);
#28385=ORIENTED_EDGE('',*,*,#20205,.T.);
#28386=ORIENTED_EDGE('',*,*,#19940,.F.);
#28387=ORIENTED_EDGE('',*,*,#20212,.F.);
#28388=ORIENTED_EDGE('',*,*,#20213,.F.);
#28389=ORIENTED_EDGE('',*,*,#20214,.T.);
#28390=ORIENTED_EDGE('',*,*,#19941,.F.);
#28391=ORIENTED_EDGE('',*,*,#20214,.F.);
#28392=ORIENTED_EDGE('',*,*,#20215,.F.);
#28393=ORIENTED_EDGE('',*,*,#20216,.F.);
#28394=ORIENTED_EDGE('',*,*,#19939,.F.);
#28395=ORIENTED_EDGE('',*,*,#20217,.F.);
#28396=ORIENTED_EDGE('',*,*,#20218,.F.);
#28397=ORIENTED_EDGE('',*,*,#20212,.T.);
#28398=ORIENTED_EDGE('',*,*,#19944,.F.);
#28399=ORIENTED_EDGE('',*,*,#20219,.F.);
#28400=ORIENTED_EDGE('',*,*,#20220,.F.);
#28401=ORIENTED_EDGE('',*,*,#20221,.T.);
#28402=ORIENTED_EDGE('',*,*,#19945,.F.);
#28403=ORIENTED_EDGE('',*,*,#20221,.F.);
#28404=ORIENTED_EDGE('',*,*,#20222,.F.);
#28405=ORIENTED_EDGE('',*,*,#20223,.F.);
#28406=ORIENTED_EDGE('',*,*,#19943,.F.);
#28407=ORIENTED_EDGE('',*,*,#20224,.F.);
#28408=ORIENTED_EDGE('',*,*,#20225,.F.);
#28409=ORIENTED_EDGE('',*,*,#20219,.T.);
#28410=ORIENTED_EDGE('',*,*,#19948,.F.);
#28411=ORIENTED_EDGE('',*,*,#20226,.F.);
#28412=ORIENTED_EDGE('',*,*,#20227,.F.);
#28413=ORIENTED_EDGE('',*,*,#20228,.T.);
#28414=ORIENTED_EDGE('',*,*,#19949,.F.);
#28415=ORIENTED_EDGE('',*,*,#20228,.F.);
#28416=ORIENTED_EDGE('',*,*,#20229,.F.);
#28417=ORIENTED_EDGE('',*,*,#20230,.F.);
#28418=ORIENTED_EDGE('',*,*,#19947,.F.);
#28419=ORIENTED_EDGE('',*,*,#20231,.F.);
#28420=ORIENTED_EDGE('',*,*,#20232,.F.);
#28421=ORIENTED_EDGE('',*,*,#20226,.T.);
#28422=ORIENTED_EDGE('',*,*,#19952,.F.);
#28423=ORIENTED_EDGE('',*,*,#20233,.F.);
#28424=ORIENTED_EDGE('',*,*,#20234,.F.);
#28425=ORIENTED_EDGE('',*,*,#20235,.T.);
#28426=ORIENTED_EDGE('',*,*,#19953,.F.);
#28427=ORIENTED_EDGE('',*,*,#20235,.F.);
#28428=ORIENTED_EDGE('',*,*,#20236,.F.);
#28429=ORIENTED_EDGE('',*,*,#20237,.F.);
#28430=ORIENTED_EDGE('',*,*,#19951,.F.);
#28431=ORIENTED_EDGE('',*,*,#20238,.F.);
#28432=ORIENTED_EDGE('',*,*,#20239,.F.);
#28433=ORIENTED_EDGE('',*,*,#20233,.T.);
#28434=ORIENTED_EDGE('',*,*,#20237,.T.);
#28435=ORIENTED_EDGE('',*,*,#20240,.F.);
#28436=ORIENTED_EDGE('',*,*,#20241,.T.);
#28437=ORIENTED_EDGE('',*,*,#19954,.T.);
#28438=ORIENTED_EDGE('',*,*,#20230,.T.);
#28439=ORIENTED_EDGE('',*,*,#20242,.F.);
#28440=ORIENTED_EDGE('',*,*,#20238,.T.);
#28441=ORIENTED_EDGE('',*,*,#19950,.T.);
#28442=ORIENTED_EDGE('',*,*,#20223,.T.);
#28443=ORIENTED_EDGE('',*,*,#20243,.F.);
#28444=ORIENTED_EDGE('',*,*,#20231,.T.);
#28445=ORIENTED_EDGE('',*,*,#19946,.T.);
#28446=ORIENTED_EDGE('',*,*,#20216,.T.);
#28447=ORIENTED_EDGE('',*,*,#20244,.F.);
#28448=ORIENTED_EDGE('',*,*,#20224,.T.);
#28449=ORIENTED_EDGE('',*,*,#19942,.T.);
#28450=ORIENTED_EDGE('',*,*,#20209,.T.);
#28451=ORIENTED_EDGE('',*,*,#20245,.F.);
#28452=ORIENTED_EDGE('',*,*,#20217,.T.);
#28453=ORIENTED_EDGE('',*,*,#19938,.T.);
#28454=ORIENTED_EDGE('',*,*,#20202,.T.);
#28455=ORIENTED_EDGE('',*,*,#20246,.F.);
#28456=ORIENTED_EDGE('',*,*,#20210,.T.);
#28457=ORIENTED_EDGE('',*,*,#19934,.T.);
#28458=ORIENTED_EDGE('',*,*,#20195,.T.);
#28459=ORIENTED_EDGE('',*,*,#20247,.F.);
#28460=ORIENTED_EDGE('',*,*,#20203,.T.);
#28461=ORIENTED_EDGE('',*,*,#19930,.T.);
#28462=ORIENTED_EDGE('',*,*,#20188,.T.);
#28463=ORIENTED_EDGE('',*,*,#20248,.F.);
#28464=ORIENTED_EDGE('',*,*,#20196,.T.);
#28465=ORIENTED_EDGE('',*,*,#19926,.T.);
#28466=ORIENTED_EDGE('',*,*,#20181,.T.);
#28467=ORIENTED_EDGE('',*,*,#20249,.F.);
#28468=ORIENTED_EDGE('',*,*,#20189,.T.);
#28469=ORIENTED_EDGE('',*,*,#19922,.T.);
#28470=ORIENTED_EDGE('',*,*,#20174,.T.);
#28471=ORIENTED_EDGE('',*,*,#20250,.F.);
#28472=ORIENTED_EDGE('',*,*,#20182,.T.);
#28473=ORIENTED_EDGE('',*,*,#19918,.T.);
#28474=ORIENTED_EDGE('',*,*,#20167,.T.);
#28475=ORIENTED_EDGE('',*,*,#20251,.F.);
#28476=ORIENTED_EDGE('',*,*,#20175,.T.);
#28477=ORIENTED_EDGE('',*,*,#19914,.T.);
#28478=ORIENTED_EDGE('',*,*,#20160,.T.);
#28479=ORIENTED_EDGE('',*,*,#20252,.F.);
#28480=ORIENTED_EDGE('',*,*,#20168,.T.);
#28481=ORIENTED_EDGE('',*,*,#19910,.T.);
#28482=ORIENTED_EDGE('',*,*,#20153,.T.);
#28483=ORIENTED_EDGE('',*,*,#20253,.F.);
#28484=ORIENTED_EDGE('',*,*,#20161,.T.);
#28485=ORIENTED_EDGE('',*,*,#19906,.T.);
#28486=ORIENTED_EDGE('',*,*,#20146,.T.);
#28487=ORIENTED_EDGE('',*,*,#20254,.F.);
#28488=ORIENTED_EDGE('',*,*,#20154,.T.);
#28489=ORIENTED_EDGE('',*,*,#19902,.T.);
#28490=ORIENTED_EDGE('',*,*,#20139,.T.);
#28491=ORIENTED_EDGE('',*,*,#20255,.F.);
#28492=ORIENTED_EDGE('',*,*,#20147,.T.);
#28493=ORIENTED_EDGE('',*,*,#19898,.T.);
#28494=ORIENTED_EDGE('',*,*,#20132,.T.);
#28495=ORIENTED_EDGE('',*,*,#20256,.F.);
#28496=ORIENTED_EDGE('',*,*,#20140,.T.);
#28497=ORIENTED_EDGE('',*,*,#19894,.T.);
#28498=ORIENTED_EDGE('',*,*,#20125,.T.);
#28499=ORIENTED_EDGE('',*,*,#20257,.F.);
#28500=ORIENTED_EDGE('',*,*,#20133,.T.);
#28501=ORIENTED_EDGE('',*,*,#19890,.T.);
#28502=ORIENTED_EDGE('',*,*,#20118,.T.);
#28503=ORIENTED_EDGE('',*,*,#20258,.F.);
#28504=ORIENTED_EDGE('',*,*,#20126,.T.);
#28505=ORIENTED_EDGE('',*,*,#19886,.T.);
#28506=ORIENTED_EDGE('',*,*,#20111,.T.);
#28507=ORIENTED_EDGE('',*,*,#20259,.F.);
#28508=ORIENTED_EDGE('',*,*,#20119,.T.);
#28509=ORIENTED_EDGE('',*,*,#19882,.T.);
#28510=ORIENTED_EDGE('',*,*,#20104,.T.);
#28511=ORIENTED_EDGE('',*,*,#20260,.F.);
#28512=ORIENTED_EDGE('',*,*,#20112,.T.);
#28513=ORIENTED_EDGE('',*,*,#19878,.T.);
#28514=ORIENTED_EDGE('',*,*,#20097,.T.);
#28515=ORIENTED_EDGE('',*,*,#20261,.F.);
#28516=ORIENTED_EDGE('',*,*,#20105,.T.);
#28517=ORIENTED_EDGE('',*,*,#19874,.T.);
#28518=ORIENTED_EDGE('',*,*,#20090,.T.);
#28519=ORIENTED_EDGE('',*,*,#20262,.F.);
#28520=ORIENTED_EDGE('',*,*,#20098,.T.);
#28521=ORIENTED_EDGE('',*,*,#19870,.T.);
#28522=ORIENTED_EDGE('',*,*,#20083,.T.);
#28523=ORIENTED_EDGE('',*,*,#20263,.F.);
#28524=ORIENTED_EDGE('',*,*,#20091,.T.);
#28525=ORIENTED_EDGE('',*,*,#19866,.T.);
#28526=ORIENTED_EDGE('',*,*,#20076,.T.);
#28527=ORIENTED_EDGE('',*,*,#20264,.F.);
#28528=ORIENTED_EDGE('',*,*,#20084,.T.);
#28529=ORIENTED_EDGE('',*,*,#19862,.T.);
#28530=ORIENTED_EDGE('',*,*,#20069,.T.);
#28531=ORIENTED_EDGE('',*,*,#20265,.F.);
#28532=ORIENTED_EDGE('',*,*,#20077,.T.);
#28533=ORIENTED_EDGE('',*,*,#19858,.T.);
#28534=ORIENTED_EDGE('',*,*,#20062,.T.);
#28535=ORIENTED_EDGE('',*,*,#20266,.F.);
#28536=ORIENTED_EDGE('',*,*,#20070,.T.);
#28537=ORIENTED_EDGE('',*,*,#19854,.T.);
#28538=ORIENTED_EDGE('',*,*,#20055,.T.);
#28539=ORIENTED_EDGE('',*,*,#20267,.F.);
#28540=ORIENTED_EDGE('',*,*,#20063,.T.);
#28541=ORIENTED_EDGE('',*,*,#19850,.T.);
#28542=ORIENTED_EDGE('',*,*,#20048,.T.);
#28543=ORIENTED_EDGE('',*,*,#20268,.F.);
#28544=ORIENTED_EDGE('',*,*,#20056,.T.);
#28545=ORIENTED_EDGE('',*,*,#19846,.T.);
#28546=ORIENTED_EDGE('',*,*,#20041,.T.);
#28547=ORIENTED_EDGE('',*,*,#20269,.F.);
#28548=ORIENTED_EDGE('',*,*,#20049,.T.);
#28549=ORIENTED_EDGE('',*,*,#19842,.T.);
#28550=ORIENTED_EDGE('',*,*,#20034,.T.);
#28551=ORIENTED_EDGE('',*,*,#20270,.F.);
#28552=ORIENTED_EDGE('',*,*,#20042,.T.);
#28553=ORIENTED_EDGE('',*,*,#19838,.T.);
#28554=ORIENTED_EDGE('',*,*,#20027,.T.);
#28555=ORIENTED_EDGE('',*,*,#20271,.F.);
#28556=ORIENTED_EDGE('',*,*,#20035,.T.);
#28557=ORIENTED_EDGE('',*,*,#19834,.T.);
#28558=ORIENTED_EDGE('',*,*,#20020,.T.);
#28559=ORIENTED_EDGE('',*,*,#20272,.F.);
#28560=ORIENTED_EDGE('',*,*,#20028,.T.);
#28561=ORIENTED_EDGE('',*,*,#19830,.T.);
#28562=ORIENTED_EDGE('',*,*,#20013,.T.);
#28563=ORIENTED_EDGE('',*,*,#20273,.F.);
#28564=ORIENTED_EDGE('',*,*,#20021,.T.);
#28565=ORIENTED_EDGE('',*,*,#19826,.T.);
#28566=ORIENTED_EDGE('',*,*,#20006,.T.);
#28567=ORIENTED_EDGE('',*,*,#20274,.F.);
#28568=ORIENTED_EDGE('',*,*,#20014,.T.);
#28569=ORIENTED_EDGE('',*,*,#19822,.T.);
#28570=ORIENTED_EDGE('',*,*,#19999,.T.);
#28571=ORIENTED_EDGE('',*,*,#20275,.F.);
#28572=ORIENTED_EDGE('',*,*,#20007,.T.);
#28573=ORIENTED_EDGE('',*,*,#19818,.T.);
#28574=ORIENTED_EDGE('',*,*,#19992,.T.);
#28575=ORIENTED_EDGE('',*,*,#20276,.F.);
#28576=ORIENTED_EDGE('',*,*,#20000,.T.);
#28577=ORIENTED_EDGE('',*,*,#19814,.T.);
#28578=ORIENTED_EDGE('',*,*,#19985,.T.);
#28579=ORIENTED_EDGE('',*,*,#20277,.F.);
#28580=ORIENTED_EDGE('',*,*,#19993,.T.);
#28581=ORIENTED_EDGE('',*,*,#19810,.T.);
#28582=ORIENTED_EDGE('',*,*,#19978,.T.);
#28583=ORIENTED_EDGE('',*,*,#20278,.F.);
#28584=ORIENTED_EDGE('',*,*,#19986,.T.);
#28585=ORIENTED_EDGE('',*,*,#19806,.T.);
#28586=ORIENTED_EDGE('',*,*,#19971,.T.);
#28587=ORIENTED_EDGE('',*,*,#20279,.F.);
#28588=ORIENTED_EDGE('',*,*,#19979,.T.);
#28589=ORIENTED_EDGE('',*,*,#19802,.T.);
#28590=ORIENTED_EDGE('',*,*,#19956,.F.);
#28591=ORIENTED_EDGE('',*,*,#20280,.F.);
#28592=ORIENTED_EDGE('',*,*,#20281,.F.);
#28593=ORIENTED_EDGE('',*,*,#20282,.T.);
#28594=ORIENTED_EDGE('',*,*,#19957,.F.);
#28595=ORIENTED_EDGE('',*,*,#20282,.F.);
#28596=ORIENTED_EDGE('',*,*,#20283,.F.);
#28597=ORIENTED_EDGE('',*,*,#20284,.F.);
#28598=ORIENTED_EDGE('',*,*,#19955,.F.);
#28599=ORIENTED_EDGE('',*,*,#20241,.F.);
#28600=ORIENTED_EDGE('',*,*,#20285,.F.);
#28601=ORIENTED_EDGE('',*,*,#20280,.T.);
#28602=ORIENTED_EDGE('',*,*,#19972,.T.);
#28603=ORIENTED_EDGE('',*,*,#19958,.T.);
#28604=ORIENTED_EDGE('',*,*,#20284,.T.);
#28605=ORIENTED_EDGE('',*,*,#20286,.F.);
#28606=ORIENTED_EDGE('',*,*,#19973,.T.);
#28607=ORIENTED_EDGE('',*,*,#20286,.T.);
#28608=ORIENTED_EDGE('',*,*,#20283,.T.);
#28609=ORIENTED_EDGE('',*,*,#20281,.T.);
#28610=ORIENTED_EDGE('',*,*,#20285,.T.);
#28611=ORIENTED_EDGE('',*,*,#20240,.T.);
#28612=ORIENTED_EDGE('',*,*,#20236,.T.);
#28613=ORIENTED_EDGE('',*,*,#20234,.T.);
#28614=ORIENTED_EDGE('',*,*,#20239,.T.);
#28615=ORIENTED_EDGE('',*,*,#20242,.T.);
#28616=ORIENTED_EDGE('',*,*,#20229,.T.);
#28617=ORIENTED_EDGE('',*,*,#20227,.T.);
#28618=ORIENTED_EDGE('',*,*,#20232,.T.);
#28619=ORIENTED_EDGE('',*,*,#20243,.T.);
#28620=ORIENTED_EDGE('',*,*,#20222,.T.);
#28621=ORIENTED_EDGE('',*,*,#20220,.T.);
#28622=ORIENTED_EDGE('',*,*,#20225,.T.);
#28623=ORIENTED_EDGE('',*,*,#20244,.T.);
#28624=ORIENTED_EDGE('',*,*,#20215,.T.);
#28625=ORIENTED_EDGE('',*,*,#20213,.T.);
#28626=ORIENTED_EDGE('',*,*,#20218,.T.);
#28627=ORIENTED_EDGE('',*,*,#20245,.T.);
#28628=ORIENTED_EDGE('',*,*,#20208,.T.);
#28629=ORIENTED_EDGE('',*,*,#20206,.T.);
#28630=ORIENTED_EDGE('',*,*,#20211,.T.);
#28631=ORIENTED_EDGE('',*,*,#20246,.T.);
#28632=ORIENTED_EDGE('',*,*,#20201,.T.);
#28633=ORIENTED_EDGE('',*,*,#20199,.T.);
#28634=ORIENTED_EDGE('',*,*,#20204,.T.);
#28635=ORIENTED_EDGE('',*,*,#20247,.T.);
#28636=ORIENTED_EDGE('',*,*,#20194,.T.);
#28637=ORIENTED_EDGE('',*,*,#20192,.T.);
#28638=ORIENTED_EDGE('',*,*,#20197,.T.);
#28639=ORIENTED_EDGE('',*,*,#20248,.T.);
#28640=ORIENTED_EDGE('',*,*,#20187,.T.);
#28641=ORIENTED_EDGE('',*,*,#20185,.T.);
#28642=ORIENTED_EDGE('',*,*,#20190,.T.);
#28643=ORIENTED_EDGE('',*,*,#20249,.T.);
#28644=ORIENTED_EDGE('',*,*,#20180,.T.);
#28645=ORIENTED_EDGE('',*,*,#20178,.T.);
#28646=ORIENTED_EDGE('',*,*,#20183,.T.);
#28647=ORIENTED_EDGE('',*,*,#20250,.T.);
#28648=ORIENTED_EDGE('',*,*,#20173,.T.);
#28649=ORIENTED_EDGE('',*,*,#20171,.T.);
#28650=ORIENTED_EDGE('',*,*,#20176,.T.);
#28651=ORIENTED_EDGE('',*,*,#20251,.T.);
#28652=ORIENTED_EDGE('',*,*,#20166,.T.);
#28653=ORIENTED_EDGE('',*,*,#20164,.T.);
#28654=ORIENTED_EDGE('',*,*,#20169,.T.);
#28655=ORIENTED_EDGE('',*,*,#20252,.T.);
#28656=ORIENTED_EDGE('',*,*,#20159,.T.);
#28657=ORIENTED_EDGE('',*,*,#20157,.T.);
#28658=ORIENTED_EDGE('',*,*,#20162,.T.);
#28659=ORIENTED_EDGE('',*,*,#20253,.T.);
#28660=ORIENTED_EDGE('',*,*,#20152,.T.);
#28661=ORIENTED_EDGE('',*,*,#20150,.T.);
#28662=ORIENTED_EDGE('',*,*,#20155,.T.);
#28663=ORIENTED_EDGE('',*,*,#20254,.T.);
#28664=ORIENTED_EDGE('',*,*,#20145,.T.);
#28665=ORIENTED_EDGE('',*,*,#20143,.T.);
#28666=ORIENTED_EDGE('',*,*,#20148,.T.);
#28667=ORIENTED_EDGE('',*,*,#20255,.T.);
#28668=ORIENTED_EDGE('',*,*,#20138,.T.);
#28669=ORIENTED_EDGE('',*,*,#20136,.T.);
#28670=ORIENTED_EDGE('',*,*,#20141,.T.);
#28671=ORIENTED_EDGE('',*,*,#20256,.T.);
#28672=ORIENTED_EDGE('',*,*,#20131,.T.);
#28673=ORIENTED_EDGE('',*,*,#20129,.T.);
#28674=ORIENTED_EDGE('',*,*,#20134,.T.);
#28675=ORIENTED_EDGE('',*,*,#20257,.T.);
#28676=ORIENTED_EDGE('',*,*,#20124,.T.);
#28677=ORIENTED_EDGE('',*,*,#20122,.T.);
#28678=ORIENTED_EDGE('',*,*,#20127,.T.);
#28679=ORIENTED_EDGE('',*,*,#20258,.T.);
#28680=ORIENTED_EDGE('',*,*,#20117,.T.);
#28681=ORIENTED_EDGE('',*,*,#20115,.T.);
#28682=ORIENTED_EDGE('',*,*,#20120,.T.);
#28683=ORIENTED_EDGE('',*,*,#20259,.T.);
#28684=ORIENTED_EDGE('',*,*,#20110,.T.);
#28685=ORIENTED_EDGE('',*,*,#20108,.T.);
#28686=ORIENTED_EDGE('',*,*,#20113,.T.);
#28687=ORIENTED_EDGE('',*,*,#20260,.T.);
#28688=ORIENTED_EDGE('',*,*,#20103,.T.);
#28689=ORIENTED_EDGE('',*,*,#20101,.T.);
#28690=ORIENTED_EDGE('',*,*,#20106,.T.);
#28691=ORIENTED_EDGE('',*,*,#20261,.T.);
#28692=ORIENTED_EDGE('',*,*,#20096,.T.);
#28693=ORIENTED_EDGE('',*,*,#20094,.T.);
#28694=ORIENTED_EDGE('',*,*,#20099,.T.);
#28695=ORIENTED_EDGE('',*,*,#20262,.T.);
#28696=ORIENTED_EDGE('',*,*,#20089,.T.);
#28697=ORIENTED_EDGE('',*,*,#20087,.T.);
#28698=ORIENTED_EDGE('',*,*,#20092,.T.);
#28699=ORIENTED_EDGE('',*,*,#20263,.T.);
#28700=ORIENTED_EDGE('',*,*,#20082,.T.);
#28701=ORIENTED_EDGE('',*,*,#20080,.T.);
#28702=ORIENTED_EDGE('',*,*,#20085,.T.);
#28703=ORIENTED_EDGE('',*,*,#20264,.T.);
#28704=ORIENTED_EDGE('',*,*,#20075,.T.);
#28705=ORIENTED_EDGE('',*,*,#20073,.T.);
#28706=ORIENTED_EDGE('',*,*,#20078,.T.);
#28707=ORIENTED_EDGE('',*,*,#20265,.T.);
#28708=ORIENTED_EDGE('',*,*,#20068,.T.);
#28709=ORIENTED_EDGE('',*,*,#20066,.T.);
#28710=ORIENTED_EDGE('',*,*,#20071,.T.);
#28711=ORIENTED_EDGE('',*,*,#20266,.T.);
#28712=ORIENTED_EDGE('',*,*,#20061,.T.);
#28713=ORIENTED_EDGE('',*,*,#20059,.T.);
#28714=ORIENTED_EDGE('',*,*,#20064,.T.);
#28715=ORIENTED_EDGE('',*,*,#20267,.T.);
#28716=ORIENTED_EDGE('',*,*,#20054,.T.);
#28717=ORIENTED_EDGE('',*,*,#20052,.T.);
#28718=ORIENTED_EDGE('',*,*,#20057,.T.);
#28719=ORIENTED_EDGE('',*,*,#20268,.T.);
#28720=ORIENTED_EDGE('',*,*,#20047,.T.);
#28721=ORIENTED_EDGE('',*,*,#20045,.T.);
#28722=ORIENTED_EDGE('',*,*,#20050,.T.);
#28723=ORIENTED_EDGE('',*,*,#20269,.T.);
#28724=ORIENTED_EDGE('',*,*,#20040,.T.);
#28725=ORIENTED_EDGE('',*,*,#20038,.T.);
#28726=ORIENTED_EDGE('',*,*,#20043,.T.);
#28727=ORIENTED_EDGE('',*,*,#20270,.T.);
#28728=ORIENTED_EDGE('',*,*,#20033,.T.);
#28729=ORIENTED_EDGE('',*,*,#20031,.T.);
#28730=ORIENTED_EDGE('',*,*,#20036,.T.);
#28731=ORIENTED_EDGE('',*,*,#20271,.T.);
#28732=ORIENTED_EDGE('',*,*,#20026,.T.);
#28733=ORIENTED_EDGE('',*,*,#20024,.T.);
#28734=ORIENTED_EDGE('',*,*,#20029,.T.);
#28735=ORIENTED_EDGE('',*,*,#20272,.T.);
#28736=ORIENTED_EDGE('',*,*,#20019,.T.);
#28737=ORIENTED_EDGE('',*,*,#20017,.T.);
#28738=ORIENTED_EDGE('',*,*,#20022,.T.);
#28739=ORIENTED_EDGE('',*,*,#20273,.T.);
#28740=ORIENTED_EDGE('',*,*,#20012,.T.);
#28741=ORIENTED_EDGE('',*,*,#20010,.T.);
#28742=ORIENTED_EDGE('',*,*,#20015,.T.);
#28743=ORIENTED_EDGE('',*,*,#20274,.T.);
#28744=ORIENTED_EDGE('',*,*,#20005,.T.);
#28745=ORIENTED_EDGE('',*,*,#20003,.T.);
#28746=ORIENTED_EDGE('',*,*,#20008,.T.);
#28747=ORIENTED_EDGE('',*,*,#20275,.T.);
#28748=ORIENTED_EDGE('',*,*,#19998,.T.);
#28749=ORIENTED_EDGE('',*,*,#19996,.T.);
#28750=ORIENTED_EDGE('',*,*,#20001,.T.);
#28751=ORIENTED_EDGE('',*,*,#20276,.T.);
#28752=ORIENTED_EDGE('',*,*,#19991,.T.);
#28753=ORIENTED_EDGE('',*,*,#19989,.T.);
#28754=ORIENTED_EDGE('',*,*,#19994,.T.);
#28755=ORIENTED_EDGE('',*,*,#20277,.T.);
#28756=ORIENTED_EDGE('',*,*,#19984,.T.);
#28757=ORIENTED_EDGE('',*,*,#19982,.T.);
#28758=ORIENTED_EDGE('',*,*,#19987,.T.);
#28759=ORIENTED_EDGE('',*,*,#20278,.T.);
#28760=ORIENTED_EDGE('',*,*,#19977,.T.);
#28761=ORIENTED_EDGE('',*,*,#19975,.T.);
#28762=ORIENTED_EDGE('',*,*,#19980,.T.);
#28763=ORIENTED_EDGE('',*,*,#20279,.T.);
#28764=ORIENTED_EDGE('',*,*,#19970,.T.);
#28765=ORIENTED_EDGE('',*,*,#19968,.T.);
#28766=ORIENTED_EDGE('',*,*,#19964,.T.);
#28767=ORIENTED_EDGE('',*,*,#19966,.T.);
#28768=ORIENTED_EDGE('',*,*,#19959,.T.);
#28769=ORIENTED_EDGE('',*,*,#19962,.T.);
#28770=ORIENTED_EDGE('',*,*,#20287,.F.);
#28771=ORIENTED_EDGE('',*,*,#20288,.F.);
#28772=ORIENTED_EDGE('',*,*,#20289,.T.);
#28773=ORIENTED_EDGE('',*,*,#20290,.F.);
#28774=ORIENTED_EDGE('',*,*,#20289,.F.);
#28775=ORIENTED_EDGE('',*,*,#20290,.T.);
#28776=ORIENTED_EDGE('',*,*,#20291,.T.);
#28777=ORIENTED_EDGE('',*,*,#20292,.F.);
#28778=ORIENTED_EDGE('',*,*,#20293,.F.);
#28779=ORIENTED_EDGE('',*,*,#20291,.F.);
#28780=ORIENTED_EDGE('',*,*,#20293,.T.);
#28781=ORIENTED_EDGE('',*,*,#20294,.T.);
#28782=ORIENTED_EDGE('',*,*,#20287,.T.);
#28783=ORIENTED_EDGE('',*,*,#20288,.T.);
#28784=ORIENTED_EDGE('',*,*,#20294,.F.);
#28785=ORIENTED_EDGE('',*,*,#20292,.T.);
#28786=ORIENTED_EDGE('',*,*,#20295,.T.);
#28787=ORIENTED_EDGE('',*,*,#20296,.T.);
#28788=ORIENTED_EDGE('',*,*,#20297,.F.);
#28789=ORIENTED_EDGE('',*,*,#20296,.F.);
#28790=ORIENTED_EDGE('',*,*,#20298,.T.);
#28791=ORIENTED_EDGE('',*,*,#20295,.F.);
#28792=ORIENTED_EDGE('',*,*,#20299,.T.);
#28793=ORIENTED_EDGE('',*,*,#20297,.T.);
#28794=ORIENTED_EDGE('',*,*,#20298,.F.);
#28795=ORIENTED_EDGE('',*,*,#20300,.T.);
#28796=ORIENTED_EDGE('',*,*,#20299,.F.);
#28797=ORIENTED_EDGE('',*,*,#20300,.F.);
#28798=ORIENTED_EDGE('',*,*,#20301,.F.);
#28799=ORIENTED_EDGE('',*,*,#20302,.F.);
#28800=ORIENTED_EDGE('',*,*,#20303,.T.);
#28801=ORIENTED_EDGE('',*,*,#20304,.F.);
#28802=ORIENTED_EDGE('',*,*,#20303,.F.);
#28803=ORIENTED_EDGE('',*,*,#20304,.T.);
#28804=ORIENTED_EDGE('',*,*,#20305,.T.);
#28805=ORIENTED_EDGE('',*,*,#20306,.F.);
#28806=ORIENTED_EDGE('',*,*,#20307,.F.);
#28807=ORIENTED_EDGE('',*,*,#20305,.F.);
#28808=ORIENTED_EDGE('',*,*,#20307,.T.);
#28809=ORIENTED_EDGE('',*,*,#20308,.T.);
#28810=ORIENTED_EDGE('',*,*,#20301,.T.);
#28811=ORIENTED_EDGE('',*,*,#20302,.T.);
#28812=ORIENTED_EDGE('',*,*,#20308,.F.);
#28813=ORIENTED_EDGE('',*,*,#20306,.T.);
#28814=ORIENTED_EDGE('',*,*,#20309,.T.);
#28815=ORIENTED_EDGE('',*,*,#20310,.T.);
#28816=ORIENTED_EDGE('',*,*,#20311,.F.);
#28817=ORIENTED_EDGE('',*,*,#20310,.F.);
#28818=ORIENTED_EDGE('',*,*,#20312,.T.);
#28819=ORIENTED_EDGE('',*,*,#20309,.F.);
#28820=ORIENTED_EDGE('',*,*,#20313,.T.);
#28821=ORIENTED_EDGE('',*,*,#20311,.T.);
#28822=ORIENTED_EDGE('',*,*,#20312,.F.);
#28823=ORIENTED_EDGE('',*,*,#20314,.T.);
#28824=ORIENTED_EDGE('',*,*,#20313,.F.);
#28825=ORIENTED_EDGE('',*,*,#20314,.F.);
#28826=ORIENTED_EDGE('',*,*,#20315,.F.);
#28827=ORIENTED_EDGE('',*,*,#20316,.T.);
#28828=ORIENTED_EDGE('',*,*,#20317,.F.);
#28829=ORIENTED_EDGE('',*,*,#20316,.F.);
#28830=ORIENTED_EDGE('',*,*,#20318,.F.);
#28831=ORIENTED_EDGE('',*,*,#20317,.T.);
#28832=ORIENTED_EDGE('',*,*,#20319,.T.);
#28833=ORIENTED_EDGE('',*,*,#20320,.T.);
#28834=ORIENTED_EDGE('',*,*,#20321,.T.);
#28835=ORIENTED_EDGE('',*,*,#20318,.T.);
#28836=ORIENTED_EDGE('',*,*,#20315,.T.);
#28837=ORIENTED_EDGE('',*,*,#20321,.F.);
#28838=ORIENTED_EDGE('',*,*,#20322,.T.);
#28839=ORIENTED_EDGE('',*,*,#20319,.F.);
#28840=ORIENTED_EDGE('',*,*,#20320,.F.);
#28841=ORIENTED_EDGE('',*,*,#20322,.F.);
#28842=ORIENTED_EDGE('',*,*,#20323,.T.);
#28843=ORIENTED_EDGE('',*,*,#20324,.T.);
#28844=ORIENTED_EDGE('',*,*,#20325,.F.);
#28845=ORIENTED_EDGE('',*,*,#20324,.F.);
#28846=ORIENTED_EDGE('',*,*,#20326,.T.);
#28847=ORIENTED_EDGE('',*,*,#20323,.F.);
#28848=ORIENTED_EDGE('',*,*,#20327,.F.);
#28849=ORIENTED_EDGE('',*,*,#20328,.T.);
#28850=ORIENTED_EDGE('',*,*,#20326,.F.);
#28851=ORIENTED_EDGE('',*,*,#20328,.F.);
#28852=ORIENTED_EDGE('',*,*,#20327,.T.);
#28853=ORIENTED_EDGE('',*,*,#20325,.T.);
#28854=ORIENTED_EDGE('',*,*,#20329,.T.);
#28855=ORIENTED_EDGE('',*,*,#20330,.T.);
#28856=ORIENTED_EDGE('',*,*,#20331,.F.);
#28857=ORIENTED_EDGE('',*,*,#20330,.F.);
#28858=ORIENTED_EDGE('',*,*,#20332,.T.);
#28859=ORIENTED_EDGE('',*,*,#20329,.F.);
#28860=ORIENTED_EDGE('',*,*,#20332,.F.);
#28861=ORIENTED_EDGE('',*,*,#20333,.T.);
#28862=ORIENTED_EDGE('',*,*,#20334,.F.);
#28863=ORIENTED_EDGE('',*,*,#20333,.F.);
#28864=ORIENTED_EDGE('',*,*,#20334,.T.);
#28865=ORIENTED_EDGE('',*,*,#20331,.T.);
#28866=ORIENTED_EDGE('',*,*,#20335,.F.);
#28867=ORIENTED_EDGE('',*,*,#20336,.F.);
#28868=ORIENTED_EDGE('',*,*,#20337,.T.);
#28869=ORIENTED_EDGE('',*,*,#20338,.F.);
#28870=ORIENTED_EDGE('',*,*,#20337,.F.);
#28871=ORIENTED_EDGE('',*,*,#20338,.T.);
#28872=ORIENTED_EDGE('',*,*,#20339,.T.);
#28873=ORIENTED_EDGE('',*,*,#20340,.T.);
#28874=ORIENTED_EDGE('',*,*,#20341,.T.);
#28875=ORIENTED_EDGE('',*,*,#20335,.T.);
#28876=ORIENTED_EDGE('',*,*,#20336,.T.);
#28877=ORIENTED_EDGE('',*,*,#20341,.F.);
#28878=ORIENTED_EDGE('',*,*,#20342,.T.);
#28879=ORIENTED_EDGE('',*,*,#20339,.F.);
#28880=ORIENTED_EDGE('',*,*,#20340,.F.);
#28881=ORIENTED_EDGE('',*,*,#20342,.F.);
#28882=ORIENTED_EDGE('',*,*,#20343,.T.);
#28883=ORIENTED_EDGE('',*,*,#20344,.T.);
#28884=ORIENTED_EDGE('',*,*,#20345,.F.);
#28885=ORIENTED_EDGE('',*,*,#20344,.F.);
#28886=ORIENTED_EDGE('',*,*,#20346,.T.);
#28887=ORIENTED_EDGE('',*,*,#20343,.F.);
#28888=ORIENTED_EDGE('',*,*,#20346,.F.);
#28889=ORIENTED_EDGE('',*,*,#20347,.T.);
#28890=ORIENTED_EDGE('',*,*,#20348,.F.);
#28891=ORIENTED_EDGE('',*,*,#20347,.F.);
#28892=ORIENTED_EDGE('',*,*,#20348,.T.);
#28893=ORIENTED_EDGE('',*,*,#20345,.T.);
#28894=ORIENTED_EDGE('',*,*,#20349,.F.);
#28895=ORIENTED_EDGE('',*,*,#20350,.F.);
#28896=ORIENTED_EDGE('',*,*,#20351,.T.);
#28897=ORIENTED_EDGE('',*,*,#20352,.F.);
#28898=ORIENTED_EDGE('',*,*,#20351,.F.);
#28899=ORIENTED_EDGE('',*,*,#20352,.T.);
#28900=ORIENTED_EDGE('',*,*,#20353,.T.);
#28901=ORIENTED_EDGE('',*,*,#20354,.T.);
#28902=ORIENTED_EDGE('',*,*,#20355,.T.);
#28903=ORIENTED_EDGE('',*,*,#20349,.T.);
#28904=ORIENTED_EDGE('',*,*,#20350,.T.);
#28905=ORIENTED_EDGE('',*,*,#20355,.F.);
#28906=ORIENTED_EDGE('',*,*,#20356,.T.);
#28907=ORIENTED_EDGE('',*,*,#20353,.F.);
#28908=ORIENTED_EDGE('',*,*,#20354,.F.);
#28909=ORIENTED_EDGE('',*,*,#20356,.F.);
#28910=ORIENTED_EDGE('',*,*,#20357,.F.);
#28911=ORIENTED_EDGE('',*,*,#20358,.T.);
#28912=ORIENTED_EDGE('',*,*,#20359,.T.);
#28913=ORIENTED_EDGE('',*,*,#20360,.F.);
#28914=ORIENTED_EDGE('',*,*,#20361,.F.);
#28915=ORIENTED_EDGE('',*,*,#20362,.F.);
#28916=ORIENTED_EDGE('',*,*,#20363,.F.);
#28917=ORIENTED_EDGE('',*,*,#20364,.F.);
#28918=ORIENTED_EDGE('',*,*,#20365,.F.);
#28919=ORIENTED_EDGE('',*,*,#20366,.F.);
#28920=ORIENTED_EDGE('',*,*,#20367,.F.);
#28921=ORIENTED_EDGE('',*,*,#20368,.F.);
#28922=ORIENTED_EDGE('',*,*,#20369,.F.);
#28923=ORIENTED_EDGE('',*,*,#20370,.F.);
#28924=ORIENTED_EDGE('',*,*,#20371,.F.);
#28925=ORIENTED_EDGE('',*,*,#20372,.F.);
#28926=ORIENTED_EDGE('',*,*,#20373,.T.);
#28927=ORIENTED_EDGE('',*,*,#20374,.T.);
#28928=ORIENTED_EDGE('',*,*,#20375,.T.);
#28929=ORIENTED_EDGE('',*,*,#20376,.T.);
#28930=ORIENTED_EDGE('',*,*,#20376,.F.);
#28931=ORIENTED_EDGE('',*,*,#20377,.T.);
#28932=ORIENTED_EDGE('',*,*,#20378,.T.);
#28933=ORIENTED_EDGE('',*,*,#20379,.T.);
#28934=ORIENTED_EDGE('',*,*,#20380,.T.);
#28935=ORIENTED_EDGE('',*,*,#20381,.T.);
#28936=ORIENTED_EDGE('',*,*,#20382,.T.);
#28937=ORIENTED_EDGE('',*,*,#20383,.T.);
#28938=ORIENTED_EDGE('',*,*,#20383,.F.);
#28939=ORIENTED_EDGE('',*,*,#20384,.T.);
#28940=ORIENTED_EDGE('',*,*,#20385,.T.);
#28941=ORIENTED_EDGE('',*,*,#20386,.T.);
#28942=ORIENTED_EDGE('',*,*,#20387,.T.);
#28943=ORIENTED_EDGE('',*,*,#20388,.T.);
#28944=ORIENTED_EDGE('',*,*,#20374,.F.);
#28945=ORIENTED_EDGE('',*,*,#20389,.T.);
#28946=ORIENTED_EDGE('',*,*,#20390,.F.);
#28947=ORIENTED_EDGE('',*,*,#20370,.T.);
#28948=ORIENTED_EDGE('',*,*,#20391,.T.);
#28949=ORIENTED_EDGE('',*,*,#20392,.T.);
#28950=ORIENTED_EDGE('',*,*,#20375,.F.);
#28951=ORIENTED_EDGE('',*,*,#20392,.F.);
#28952=ORIENTED_EDGE('',*,*,#20393,.T.);
#28953=ORIENTED_EDGE('',*,*,#20394,.T.);
#28954=ORIENTED_EDGE('',*,*,#20395,.F.);
#28955=ORIENTED_EDGE('',*,*,#20362,.T.);
#28956=ORIENTED_EDGE('',*,*,#20396,.F.);
#28957=ORIENTED_EDGE('',*,*,#20377,.F.);
#28958=ORIENTED_EDGE('',*,*,#20382,.F.);
#28959=ORIENTED_EDGE('',*,*,#20397,.F.);
#28960=ORIENTED_EDGE('',*,*,#20398,.F.);
#28961=ORIENTED_EDGE('',*,*,#20399,.T.);
#28962=ORIENTED_EDGE('',*,*,#20400,.F.);
#28963=ORIENTED_EDGE('',*,*,#20401,.F.);
#28964=ORIENTED_EDGE('',*,*,#20402,.T.);
#28965=ORIENTED_EDGE('',*,*,#20384,.F.);
#28966=ORIENTED_EDGE('',*,*,#20381,.F.);
#28967=ORIENTED_EDGE('',*,*,#20403,.T.);
#28968=ORIENTED_EDGE('',*,*,#20404,.F.);
#28969=ORIENTED_EDGE('',*,*,#20397,.T.);
#28970=ORIENTED_EDGE('',*,*,#20373,.F.);
#28971=ORIENTED_EDGE('',*,*,#20379,.F.);
#28972=ORIENTED_EDGE('',*,*,#20405,.F.);
#28973=ORIENTED_EDGE('',*,*,#20406,.F.);
#28974=ORIENTED_EDGE('',*,*,#20407,.F.);
#28975=ORIENTED_EDGE('',*,*,#20408,.F.);
#28976=ORIENTED_EDGE('',*,*,#20409,.F.);
#28977=ORIENTED_EDGE('',*,*,#20403,.F.);
#28978=ORIENTED_EDGE('',*,*,#20380,.F.);
#28979=ORIENTED_EDGE('',*,*,#20388,.F.);
#28980=ORIENTED_EDGE('',*,*,#20410,.F.);
#28981=ORIENTED_EDGE('',*,*,#20411,.F.);
#28982=ORIENTED_EDGE('',*,*,#20412,.F.);
#28983=ORIENTED_EDGE('',*,*,#20413,.F.);
#28984=ORIENTED_EDGE('',*,*,#20414,.F.);
#28985=ORIENTED_EDGE('',*,*,#20389,.F.);
#28986=ORIENTED_EDGE('',*,*,#20415,.F.);
#28987=ORIENTED_EDGE('',*,*,#20416,.F.);
#28988=ORIENTED_EDGE('',*,*,#20417,.T.);
#28989=ORIENTED_EDGE('',*,*,#20418,.F.);
#28990=ORIENTED_EDGE('',*,*,#20419,.F.);
#28991=ORIENTED_EDGE('',*,*,#20417,.F.);
#28992=ORIENTED_EDGE('',*,*,#20406,.T.);
#28993=ORIENTED_EDGE('',*,*,#20420,.F.);
#28994=ORIENTED_EDGE('',*,*,#20360,.T.);
#28995=ORIENTED_EDGE('',*,*,#20421,.F.);
#28996=ORIENTED_EDGE('',*,*,#20421,.T.);
#28997=ORIENTED_EDGE('',*,*,#20359,.F.);
#28998=ORIENTED_EDGE('',*,*,#20422,.T.);
#28999=ORIENTED_EDGE('',*,*,#20423,.F.);
#29000=ORIENTED_EDGE('',*,*,#20424,.F.);
#29001=ORIENTED_EDGE('',*,*,#20425,.T.);
#29002=ORIENTED_EDGE('',*,*,#20426,.F.);
#29003=ORIENTED_EDGE('',*,*,#20427,.F.);
#29004=ORIENTED_EDGE('',*,*,#20407,.T.);
#29005=ORIENTED_EDGE('',*,*,#20416,.T.);
#29006=ORIENTED_EDGE('',*,*,#20428,.T.);
#29007=ORIENTED_EDGE('',*,*,#20429,.T.);
#29008=ORIENTED_EDGE('',*,*,#20430,.T.);
#29009=ORIENTED_EDGE('',*,*,#20428,.F.);
#29010=ORIENTED_EDGE('',*,*,#20431,.T.);
#29011=ORIENTED_EDGE('',*,*,#20432,.F.);
#29012=ORIENTED_EDGE('',*,*,#20433,.F.);
#29013=ORIENTED_EDGE('',*,*,#20431,.F.);
#29014=ORIENTED_EDGE('',*,*,#20434,.F.);
#29015=ORIENTED_EDGE('',*,*,#20435,.F.);
#29016=ORIENTED_EDGE('',*,*,#20408,.T.);
#29017=ORIENTED_EDGE('',*,*,#20427,.T.);
#29018=ORIENTED_EDGE('',*,*,#20436,.T.);
#29019=ORIENTED_EDGE('',*,*,#20424,.T.);
#29020=ORIENTED_EDGE('',*,*,#20437,.F.);
#29021=ORIENTED_EDGE('',*,*,#20438,.F.);
#29022=ORIENTED_EDGE('',*,*,#20439,.F.);
#29023=ORIENTED_EDGE('',*,*,#20440,.F.);
#29024=ORIENTED_EDGE('',*,*,#20441,.F.);
#29025=ORIENTED_EDGE('',*,*,#20442,.F.);
#29026=ORIENTED_EDGE('',*,*,#20443,.F.);
#29027=ORIENTED_EDGE('',*,*,#20444,.F.);
#29028=ORIENTED_EDGE('',*,*,#20445,.F.);
#29029=ORIENTED_EDGE('',*,*,#20430,.F.);
#29030=ORIENTED_EDGE('',*,*,#20446,.T.);
#29031=ORIENTED_EDGE('',*,*,#20447,.F.);
#29032=ORIENTED_EDGE('',*,*,#20448,.F.);
#29033=ORIENTED_EDGE('',*,*,#20446,.F.);
#29034=ORIENTED_EDGE('',*,*,#20436,.F.);
#29035=ORIENTED_EDGE('',*,*,#20449,.F.);
#29036=ORIENTED_EDGE('',*,*,#20450,.T.);
#29037=ORIENTED_EDGE('',*,*,#20425,.F.);
#29038=ORIENTED_EDGE('',*,*,#20358,.F.);
#29039=ORIENTED_EDGE('',*,*,#20451,.F.);
#29040=ORIENTED_EDGE('',*,*,#20452,.T.);
#29041=ORIENTED_EDGE('',*,*,#20422,.F.);
#29042=ORIENTED_EDGE('',*,*,#20429,.F.);
#29043=ORIENTED_EDGE('',*,*,#20453,.T.);
#29044=ORIENTED_EDGE('',*,*,#20454,.F.);
#29045=ORIENTED_EDGE('',*,*,#20455,.F.);
#29046=ORIENTED_EDGE('',*,*,#20453,.F.);
#29047=ORIENTED_EDGE('',*,*,#20452,.F.);
#29048=ORIENTED_EDGE('',*,*,#20456,.F.);
#29049=ORIENTED_EDGE('',*,*,#20457,.F.);
#29050=ORIENTED_EDGE('',*,*,#20458,.F.);
#29051=ORIENTED_EDGE('',*,*,#20459,.F.);
#29052=ORIENTED_EDGE('',*,*,#20441,.T.);
#29053=ORIENTED_EDGE('',*,*,#20460,.F.);
#29054=ORIENTED_EDGE('',*,*,#20439,.T.);
#29055=ORIENTED_EDGE('',*,*,#20461,.F.);
#29056=ORIENTED_EDGE('',*,*,#20437,.T.);
#29057=ORIENTED_EDGE('',*,*,#20423,.T.);
#29058=ORIENTED_EDGE('',*,*,#20426,.T.);
#29059=ORIENTED_EDGE('',*,*,#20450,.F.);
#29060=ORIENTED_EDGE('',*,*,#20462,.F.);
#29061=ORIENTED_EDGE('',*,*,#20463,.F.);
#29062=ORIENTED_EDGE('',*,*,#20464,.F.);
#29063=ORIENTED_EDGE('',*,*,#20465,.T.);
#29064=ORIENTED_EDGE('',*,*,#20466,.F.);
#29065=ORIENTED_EDGE('',*,*,#20386,.F.);
#29066=ORIENTED_EDGE('',*,*,#20467,.F.);
#29067=ORIENTED_EDGE('',*,*,#20468,.F.);
#29068=ORIENTED_EDGE('',*,*,#20469,.F.);
#29069=ORIENTED_EDGE('',*,*,#20470,.F.);
#29070=ORIENTED_EDGE('',*,*,#20471,.F.);
#29071=ORIENTED_EDGE('',*,*,#20472,.F.);
#29072=ORIENTED_EDGE('',*,*,#20473,.F.);
#29073=ORIENTED_EDGE('',*,*,#20399,.F.);
#29074=ORIENTED_EDGE('',*,*,#20474,.F.);
#29075=ORIENTED_EDGE('',*,*,#20434,.T.);
#29076=ORIENTED_EDGE('',*,*,#20475,.T.);
#29077=ORIENTED_EDGE('',*,*,#20476,.T.);
#29078=ORIENTED_EDGE('',*,*,#20477,.F.);
#29079=ORIENTED_EDGE('',*,*,#20478,.F.);
#29080=ORIENTED_EDGE('',*,*,#20476,.F.);
#29081=ORIENTED_EDGE('',*,*,#20479,.T.);
#29082=ORIENTED_EDGE('',*,*,#20480,.F.);
#29083=ORIENTED_EDGE('',*,*,#20481,.F.);
#29084=ORIENTED_EDGE('',*,*,#20482,.F.);
#29085=ORIENTED_EDGE('',*,*,#20483,.F.);
#29086=ORIENTED_EDGE('',*,*,#20484,.T.);
#29087=ORIENTED_EDGE('',*,*,#20485,.T.);
#29088=ORIENTED_EDGE('',*,*,#20486,.T.);
#29089=ORIENTED_EDGE('',*,*,#20485,.F.);
#29090=ORIENTED_EDGE('',*,*,#20487,.T.);
#29091=ORIENTED_EDGE('',*,*,#20488,.F.);
#29092=ORIENTED_EDGE('',*,*,#20489,.F.);
#29093=ORIENTED_EDGE('',*,*,#20490,.F.);
#29094=ORIENTED_EDGE('',*,*,#20491,.F.);
#29095=ORIENTED_EDGE('',*,*,#20489,.T.);
#29096=ORIENTED_EDGE('',*,*,#20492,.F.);
#29097=ORIENTED_EDGE('',*,*,#20493,.T.);
#29098=ORIENTED_EDGE('',*,*,#20490,.T.);
#29099=ORIENTED_EDGE('',*,*,#20493,.F.);
#29100=ORIENTED_EDGE('',*,*,#20494,.F.);
#29101=ORIENTED_EDGE('',*,*,#20495,.F.);
#29102=ORIENTED_EDGE('',*,*,#20496,.T.);
#29103=ORIENTED_EDGE('',*,*,#20497,.T.);
#29104=ORIENTED_EDGE('',*,*,#20498,.F.);
#29105=ORIENTED_EDGE('',*,*,#20499,.F.);
#29106=ORIENTED_EDGE('',*,*,#20500,.T.);
#29107=ORIENTED_EDGE('',*,*,#20501,.T.);
#29108=ORIENTED_EDGE('',*,*,#20496,.F.);
#29109=ORIENTED_EDGE('',*,*,#20502,.F.);
#29110=ORIENTED_EDGE('',*,*,#20503,.T.);
#29111=ORIENTED_EDGE('',*,*,#20504,.T.);
#29112=ORIENTED_EDGE('',*,*,#20500,.F.);
#29113=ORIENTED_EDGE('',*,*,#20505,.F.);
#29114=ORIENTED_EDGE('',*,*,#20479,.F.);
#29115=ORIENTED_EDGE('',*,*,#20475,.F.);
#29116=ORIENTED_EDGE('',*,*,#20506,.F.);
#29117=ORIENTED_EDGE('',*,*,#20507,.T.);
#29118=ORIENTED_EDGE('',*,*,#20508,.F.);
#29119=ORIENTED_EDGE('',*,*,#20487,.F.);
#29120=ORIENTED_EDGE('',*,*,#20484,.F.);
#29121=ORIENTED_EDGE('',*,*,#20509,.F.);
#29122=ORIENTED_EDGE('',*,*,#20507,.F.);
#29123=ORIENTED_EDGE('',*,*,#20510,.T.);
#29124=ORIENTED_EDGE('',*,*,#20511,.T.);
#29125=ORIENTED_EDGE('',*,*,#20512,.T.);
#29126=ORIENTED_EDGE('',*,*,#20513,.T.);
#29127=ORIENTED_EDGE('',*,*,#20514,.F.);
#29128=ORIENTED_EDGE('',*,*,#20513,.F.);
#29129=ORIENTED_EDGE('',*,*,#20515,.T.);
#29130=ORIENTED_EDGE('',*,*,#20516,.T.);
#29131=ORIENTED_EDGE('',*,*,#20517,.T.);
#29132=ORIENTED_EDGE('',*,*,#20518,.F.);
#29133=ORIENTED_EDGE('',*,*,#20517,.F.);
#29134=ORIENTED_EDGE('',*,*,#20519,.T.);
#29135=ORIENTED_EDGE('',*,*,#20520,.T.);
#29136=ORIENTED_EDGE('',*,*,#20521,.T.);
#29137=ORIENTED_EDGE('',*,*,#20522,.F.);
#29138=ORIENTED_EDGE('',*,*,#20521,.F.);
#29139=ORIENTED_EDGE('',*,*,#20523,.T.);
#29140=ORIENTED_EDGE('',*,*,#20524,.T.);
#29141=ORIENTED_EDGE('',*,*,#20525,.T.);
#29142=ORIENTED_EDGE('',*,*,#20526,.F.);
#29143=ORIENTED_EDGE('',*,*,#20525,.F.);
#29144=ORIENTED_EDGE('',*,*,#20491,.T.);
#29145=ORIENTED_EDGE('',*,*,#20494,.T.);
#29146=ORIENTED_EDGE('',*,*,#20492,.T.);
#29147=ORIENTED_EDGE('',*,*,#20488,.T.);
#29148=ORIENTED_EDGE('',*,*,#20508,.T.);
#29149=ORIENTED_EDGE('',*,*,#20509,.T.);
#29150=ORIENTED_EDGE('',*,*,#20506,.T.);
#29151=ORIENTED_EDGE('',*,*,#20482,.T.);
#29152=ORIENTED_EDGE('',*,*,#20527,.T.);
#29153=ORIENTED_EDGE('',*,*,#20528,.F.);
#29154=ORIENTED_EDGE('',*,*,#20529,.F.);
#29155=ORIENTED_EDGE('',*,*,#20530,.F.);
#29156=ORIENTED_EDGE('',*,*,#20531,.F.);
#29157=ORIENTED_EDGE('',*,*,#20481,.T.);
#29158=ORIENTED_EDGE('',*,*,#20532,.F.);
#29159=ORIENTED_EDGE('',*,*,#20533,.F.);
#29160=ORIENTED_EDGE('',*,*,#20534,.F.);
#29161=ORIENTED_EDGE('',*,*,#20535,.F.);
#29162=ORIENTED_EDGE('',*,*,#20527,.F.);
#29163=ORIENTED_EDGE('',*,*,#20536,.F.);
#29164=ORIENTED_EDGE('',*,*,#20537,.F.);
#29165=ORIENTED_EDGE('',*,*,#20538,.F.);
#29166=ORIENTED_EDGE('',*,*,#20502,.T.);
#29167=ORIENTED_EDGE('',*,*,#20499,.T.);
#29168=ORIENTED_EDGE('',*,*,#20495,.T.);
#29169=ORIENTED_EDGE('',*,*,#20539,.T.);
#29170=ORIENTED_EDGE('',*,*,#20540,.T.);
#29171=ORIENTED_EDGE('',*,*,#20541,.T.);
#29172=ORIENTED_EDGE('',*,*,#20542,.T.);
#29173=ORIENTED_EDGE('',*,*,#20543,.T.);
#29174=ORIENTED_EDGE('',*,*,#20544,.T.);
#29175=ORIENTED_EDGE('',*,*,#20545,.T.);
#29176=ORIENTED_EDGE('',*,*,#20546,.F.);
#29177=ORIENTED_EDGE('',*,*,#20547,.T.);
#29178=ORIENTED_EDGE('',*,*,#20548,.F.);
#29179=ORIENTED_EDGE('',*,*,#20547,.F.);
#29180=ORIENTED_EDGE('',*,*,#20546,.T.);
#29181=ORIENTED_EDGE('',*,*,#20549,.T.);
#29182=ORIENTED_EDGE('',*,*,#20550,.T.);
#29183=ORIENTED_EDGE('',*,*,#20551,.T.);
#29184=ORIENTED_EDGE('',*,*,#20552,.T.);
#29185=ORIENTED_EDGE('',*,*,#20553,.F.);
#29186=ORIENTED_EDGE('',*,*,#20554,.F.);
#29187=ORIENTED_EDGE('',*,*,#20555,.T.);
#29188=ORIENTED_EDGE('',*,*,#20556,.T.);
#29189=ORIENTED_EDGE('',*,*,#20557,.T.);
#29190=ORIENTED_EDGE('',*,*,#20554,.T.);
#29191=ORIENTED_EDGE('',*,*,#20558,.F.);
#29192=ORIENTED_EDGE('',*,*,#20559,.F.);
#29193=ORIENTED_EDGE('',*,*,#20560,.T.);
#29194=ORIENTED_EDGE('',*,*,#20561,.T.);
#29195=ORIENTED_EDGE('',*,*,#20562,.T.);
#29196=ORIENTED_EDGE('',*,*,#20559,.T.);
#29197=ORIENTED_EDGE('',*,*,#20563,.F.);
#29198=ORIENTED_EDGE('',*,*,#20564,.F.);
#29199=ORIENTED_EDGE('',*,*,#20565,.T.);
#29200=ORIENTED_EDGE('',*,*,#20566,.T.);
#29201=ORIENTED_EDGE('',*,*,#20567,.T.);
#29202=ORIENTED_EDGE('',*,*,#20564,.T.);
#29203=ORIENTED_EDGE('',*,*,#20568,.F.);
#29204=ORIENTED_EDGE('',*,*,#20569,.F.);
#29205=ORIENTED_EDGE('',*,*,#20565,.F.);
#29206=ORIENTED_EDGE('',*,*,#20570,.F.);
#29207=ORIENTED_EDGE('',*,*,#20571,.T.);
#29208=ORIENTED_EDGE('',*,*,#20567,.F.);
#29209=ORIENTED_EDGE('',*,*,#20572,.T.);
#29210=ORIENTED_EDGE('',*,*,#20560,.F.);
#29211=ORIENTED_EDGE('',*,*,#20573,.F.);
#29212=ORIENTED_EDGE('',*,*,#20574,.F.);
#29213=ORIENTED_EDGE('',*,*,#20575,.T.);
#29214=ORIENTED_EDGE('',*,*,#20576,.F.);
#29215=ORIENTED_EDGE('',*,*,#20551,.F.);
#29216=ORIENTED_EDGE('',*,*,#20577,.T.);
#29217=ORIENTED_EDGE('',*,*,#20557,.F.);
#29218=ORIENTED_EDGE('',*,*,#20578,.T.);
#29219=ORIENTED_EDGE('',*,*,#20549,.F.);
#29220=ORIENTED_EDGE('',*,*,#20576,.T.);
#29221=ORIENTED_EDGE('',*,*,#20579,.T.);
#29222=ORIENTED_EDGE('',*,*,#20574,.T.);
#29223=ORIENTED_EDGE('',*,*,#20580,.T.);
#29224=ORIENTED_EDGE('',*,*,#20581,.F.);
#29225=ORIENTED_EDGE('',*,*,#20552,.F.);
#29226=ORIENTED_EDGE('',*,*,#20573,.T.);
#29227=ORIENTED_EDGE('',*,*,#20582,.T.);
#29228=ORIENTED_EDGE('',*,*,#20570,.T.);
#29229=ORIENTED_EDGE('',*,*,#20569,.T.);
#29230=ORIENTED_EDGE('',*,*,#20583,.F.);
#29231=ORIENTED_EDGE('',*,*,#20580,.F.);
#29232=ORIENTED_EDGE('',*,*,#20555,.F.);
#29233=ORIENTED_EDGE('',*,*,#20562,.F.);
#29234=ORIENTED_EDGE('',*,*,#20584,.T.);
#29235=ORIENTED_EDGE('',*,*,#20572,.F.);
#29236=ORIENTED_EDGE('',*,*,#20566,.F.);
#29237=ORIENTED_EDGE('',*,*,#20571,.F.);
#29238=ORIENTED_EDGE('',*,*,#20582,.F.);
#29239=ORIENTED_EDGE('',*,*,#20575,.F.);
#29240=ORIENTED_EDGE('',*,*,#20579,.F.);
#29241=ORIENTED_EDGE('',*,*,#20577,.F.);
#29242=ORIENTED_EDGE('',*,*,#20550,.F.);
#29243=ORIENTED_EDGE('',*,*,#20578,.F.);
#29244=ORIENTED_EDGE('',*,*,#20556,.F.);
#29245=ORIENTED_EDGE('',*,*,#20584,.F.);
#29246=ORIENTED_EDGE('',*,*,#20561,.F.);
#29247=ORIENTED_EDGE('',*,*,#20585,.T.);
#29248=ORIENTED_EDGE('',*,*,#20586,.T.);
#29249=ORIENTED_EDGE('',*,*,#20587,.T.);
#29250=ORIENTED_EDGE('',*,*,#20588,.T.);
#29251=ORIENTED_EDGE('',*,*,#20589,.F.);
#29252=ORIENTED_EDGE('',*,*,#20590,.F.);
#29253=ORIENTED_EDGE('',*,*,#20591,.T.);
#29254=ORIENTED_EDGE('',*,*,#20592,.T.);
#29255=ORIENTED_EDGE('',*,*,#20593,.T.);
#29256=ORIENTED_EDGE('',*,*,#20590,.T.);
#29257=ORIENTED_EDGE('',*,*,#20594,.F.);
#29258=ORIENTED_EDGE('',*,*,#20595,.F.);
#29259=ORIENTED_EDGE('',*,*,#20596,.T.);
#29260=ORIENTED_EDGE('',*,*,#20597,.T.);
#29261=ORIENTED_EDGE('',*,*,#20598,.T.);
#29262=ORIENTED_EDGE('',*,*,#20595,.T.);
#29263=ORIENTED_EDGE('',*,*,#20599,.F.);
#29264=ORIENTED_EDGE('',*,*,#20600,.F.);
#29265=ORIENTED_EDGE('',*,*,#20601,.T.);
#29266=ORIENTED_EDGE('',*,*,#20602,.T.);
#29267=ORIENTED_EDGE('',*,*,#20603,.T.);
#29268=ORIENTED_EDGE('',*,*,#20600,.T.);
#29269=ORIENTED_EDGE('',*,*,#20604,.F.);
#29270=ORIENTED_EDGE('',*,*,#20605,.F.);
#29271=ORIENTED_EDGE('',*,*,#20601,.F.);
#29272=ORIENTED_EDGE('',*,*,#20606,.F.);
#29273=ORIENTED_EDGE('',*,*,#20607,.T.);
#29274=ORIENTED_EDGE('',*,*,#20603,.F.);
#29275=ORIENTED_EDGE('',*,*,#20608,.T.);
#29276=ORIENTED_EDGE('',*,*,#20596,.F.);
#29277=ORIENTED_EDGE('',*,*,#20609,.F.);
#29278=ORIENTED_EDGE('',*,*,#20610,.F.);
#29279=ORIENTED_EDGE('',*,*,#20611,.T.);
#29280=ORIENTED_EDGE('',*,*,#20612,.F.);
#29281=ORIENTED_EDGE('',*,*,#20587,.F.);
#29282=ORIENTED_EDGE('',*,*,#20613,.T.);
#29283=ORIENTED_EDGE('',*,*,#20593,.F.);
#29284=ORIENTED_EDGE('',*,*,#20614,.T.);
#29285=ORIENTED_EDGE('',*,*,#20585,.F.);
#29286=ORIENTED_EDGE('',*,*,#20612,.T.);
#29287=ORIENTED_EDGE('',*,*,#20615,.T.);
#29288=ORIENTED_EDGE('',*,*,#20610,.T.);
#29289=ORIENTED_EDGE('',*,*,#20616,.T.);
#29290=ORIENTED_EDGE('',*,*,#20617,.F.);
#29291=ORIENTED_EDGE('',*,*,#20588,.F.);
#29292=ORIENTED_EDGE('',*,*,#20609,.T.);
#29293=ORIENTED_EDGE('',*,*,#20618,.T.);
#29294=ORIENTED_EDGE('',*,*,#20606,.T.);
#29295=ORIENTED_EDGE('',*,*,#20605,.T.);
#29296=ORIENTED_EDGE('',*,*,#20619,.F.);
#29297=ORIENTED_EDGE('',*,*,#20616,.F.);
#29298=ORIENTED_EDGE('',*,*,#20591,.F.);
#29299=ORIENTED_EDGE('',*,*,#20598,.F.);
#29300=ORIENTED_EDGE('',*,*,#20620,.T.);
#29301=ORIENTED_EDGE('',*,*,#20608,.F.);
#29302=ORIENTED_EDGE('',*,*,#20602,.F.);
#29303=ORIENTED_EDGE('',*,*,#20607,.F.);
#29304=ORIENTED_EDGE('',*,*,#20618,.F.);
#29305=ORIENTED_EDGE('',*,*,#20611,.F.);
#29306=ORIENTED_EDGE('',*,*,#20615,.F.);
#29307=ORIENTED_EDGE('',*,*,#20613,.F.);
#29308=ORIENTED_EDGE('',*,*,#20586,.F.);
#29309=ORIENTED_EDGE('',*,*,#20614,.F.);
#29310=ORIENTED_EDGE('',*,*,#20592,.F.);
#29311=ORIENTED_EDGE('',*,*,#20620,.F.);
#29312=ORIENTED_EDGE('',*,*,#20597,.F.);
#29313=ORIENTED_EDGE('',*,*,#20385,.F.);
#29314=ORIENTED_EDGE('',*,*,#20402,.F.);
#29315=ORIENTED_EDGE('',*,*,#20621,.F.);
#29316=ORIENTED_EDGE('',*,*,#20622,.T.);
#29317=ORIENTED_EDGE('',*,*,#20467,.T.);
#29318=ORIENTED_EDGE('',*,*,#20623,.F.);
#29319=ORIENTED_EDGE('',*,*,#20368,.T.);
#29320=ORIENTED_EDGE('',*,*,#20624,.T.);
#29321=ORIENTED_EDGE('',*,*,#20625,.T.);
#29322=ORIENTED_EDGE('',*,*,#20624,.F.);
#29323=ORIENTED_EDGE('',*,*,#20367,.T.);
#29324=ORIENTED_EDGE('',*,*,#20626,.T.);
#29325=ORIENTED_EDGE('',*,*,#20627,.T.);
#29326=ORIENTED_EDGE('',*,*,#20626,.F.);
#29327=ORIENTED_EDGE('',*,*,#20366,.T.);
#29328=ORIENTED_EDGE('',*,*,#20628,.T.);
#29329=ORIENTED_EDGE('',*,*,#20629,.T.);
#29330=ORIENTED_EDGE('',*,*,#20628,.F.);
#29331=ORIENTED_EDGE('',*,*,#20365,.T.);
#29332=ORIENTED_EDGE('',*,*,#20630,.T.);
#29333=ORIENTED_EDGE('',*,*,#20631,.T.);
#29334=ORIENTED_EDGE('',*,*,#20630,.F.);
#29335=ORIENTED_EDGE('',*,*,#20364,.T.);
#29336=ORIENTED_EDGE('',*,*,#20632,.T.);
#29337=ORIENTED_EDGE('',*,*,#20633,.T.);
#29338=ORIENTED_EDGE('',*,*,#20632,.F.);
#29339=ORIENTED_EDGE('',*,*,#20363,.T.);
#29340=ORIENTED_EDGE('',*,*,#20395,.T.);
#29341=ORIENTED_EDGE('',*,*,#20634,.T.);
#29342=ORIENTED_EDGE('',*,*,#20411,.T.);
#29343=ORIENTED_EDGE('',*,*,#20635,.F.);
#29344=ORIENTED_EDGE('',*,*,#20465,.F.);
#29345=ORIENTED_EDGE('',*,*,#20636,.F.);
#29346=ORIENTED_EDGE('',*,*,#20413,.T.);
#29347=ORIENTED_EDGE('',*,*,#20637,.F.);
#29348=ORIENTED_EDGE('',*,*,#20372,.T.);
#29349=ORIENTED_EDGE('',*,*,#20638,.F.);
#29350=ORIENTED_EDGE('',*,*,#20414,.T.);
#29351=ORIENTED_EDGE('',*,*,#20638,.T.);
#29352=ORIENTED_EDGE('',*,*,#20371,.T.);
#29353=ORIENTED_EDGE('',*,*,#20390,.T.);
#29354=ORIENTED_EDGE('',*,*,#20639,.T.);
#29355=ORIENTED_EDGE('',*,*,#20461,.T.);
#29356=ORIENTED_EDGE('',*,*,#20640,.T.);
#29357=ORIENTED_EDGE('',*,*,#20460,.T.);
#29358=ORIENTED_EDGE('',*,*,#20641,.T.);
#29359=ORIENTED_EDGE('',*,*,#20642,.T.);
#29360=ORIENTED_EDGE('',*,*,#20643,.T.);
#29361=ORIENTED_EDGE('',*,*,#20644,.T.);
#29362=ORIENTED_EDGE('',*,*,#20645,.T.);
#29363=ORIENTED_EDGE('',*,*,#20646,.T.);
#29364=ORIENTED_EDGE('',*,*,#20647,.T.);
#29365=ORIENTED_EDGE('',*,*,#20648,.F.);
#29366=ORIENTED_EDGE('',*,*,#20646,.F.);
#29367=ORIENTED_EDGE('',*,*,#20649,.T.);
#29368=ORIENTED_EDGE('',*,*,#20650,.T.);
#29369=ORIENTED_EDGE('',*,*,#20649,.F.);
#29370=ORIENTED_EDGE('',*,*,#20645,.F.);
#29371=ORIENTED_EDGE('',*,*,#20651,.T.);
#29372=ORIENTED_EDGE('',*,*,#20652,.T.);
#29373=ORIENTED_EDGE('',*,*,#20653,.F.);
#29374=ORIENTED_EDGE('',*,*,#20651,.F.);
#29375=ORIENTED_EDGE('',*,*,#20644,.F.);
#29376=ORIENTED_EDGE('',*,*,#20654,.T.);
#29377=ORIENTED_EDGE('',*,*,#20652,.F.);
#29378=ORIENTED_EDGE('',*,*,#20643,.F.);
#29379=ORIENTED_EDGE('',*,*,#20655,.T.);
#29380=ORIENTED_EDGE('',*,*,#20656,.T.);
#29381=ORIENTED_EDGE('',*,*,#20655,.F.);
#29382=ORIENTED_EDGE('',*,*,#20642,.F.);
#29383=ORIENTED_EDGE('',*,*,#20657,.T.);
#29384=ORIENTED_EDGE('',*,*,#20658,.T.);
#29385=ORIENTED_EDGE('',*,*,#20657,.F.);
#29386=ORIENTED_EDGE('',*,*,#20641,.F.);
#29387=ORIENTED_EDGE('',*,*,#20648,.T.);
#29388=ORIENTED_EDGE('',*,*,#20659,.T.);
#29389=ORIENTED_EDGE('',*,*,#20438,.T.);
#29390=ORIENTED_EDGE('',*,*,#20639,.F.);
#29391=ORIENTED_EDGE('',*,*,#20659,.F.);
#29392=ORIENTED_EDGE('',*,*,#20654,.F.);
#29393=ORIENTED_EDGE('',*,*,#20656,.F.);
#29394=ORIENTED_EDGE('',*,*,#20658,.F.);
#29395=ORIENTED_EDGE('',*,*,#20647,.F.);
#29396=ORIENTED_EDGE('',*,*,#20650,.F.);
#29397=ORIENTED_EDGE('',*,*,#20653,.T.);
#29398=ORIENTED_EDGE('',*,*,#20660,.T.);
#29399=ORIENTED_EDGE('',*,*,#20661,.T.);
#29400=ORIENTED_EDGE('',*,*,#20662,.T.);
#29401=ORIENTED_EDGE('',*,*,#20663,.T.);
#29402=ORIENTED_EDGE('',*,*,#20664,.T.);
#29403=ORIENTED_EDGE('',*,*,#20665,.T.);
#29404=ORIENTED_EDGE('',*,*,#20666,.T.);
#29405=ORIENTED_EDGE('',*,*,#20667,.F.);
#29406=ORIENTED_EDGE('',*,*,#20665,.F.);
#29407=ORIENTED_EDGE('',*,*,#20668,.T.);
#29408=ORIENTED_EDGE('',*,*,#20669,.T.);
#29409=ORIENTED_EDGE('',*,*,#20668,.F.);
#29410=ORIENTED_EDGE('',*,*,#20664,.F.);
#29411=ORIENTED_EDGE('',*,*,#20670,.T.);
#29412=ORIENTED_EDGE('',*,*,#20671,.T.);
#29413=ORIENTED_EDGE('',*,*,#20672,.F.);
#29414=ORIENTED_EDGE('',*,*,#20670,.F.);
#29415=ORIENTED_EDGE('',*,*,#20663,.F.);
#29416=ORIENTED_EDGE('',*,*,#20673,.T.);
#29417=ORIENTED_EDGE('',*,*,#20671,.F.);
#29418=ORIENTED_EDGE('',*,*,#20662,.F.);
#29419=ORIENTED_EDGE('',*,*,#20674,.T.);
#29420=ORIENTED_EDGE('',*,*,#20675,.T.);
#29421=ORIENTED_EDGE('',*,*,#20674,.F.);
#29422=ORIENTED_EDGE('',*,*,#20661,.F.);
#29423=ORIENTED_EDGE('',*,*,#20676,.T.);
#29424=ORIENTED_EDGE('',*,*,#20677,.T.);
#29425=ORIENTED_EDGE('',*,*,#20676,.F.);
#29426=ORIENTED_EDGE('',*,*,#20660,.F.);
#29427=ORIENTED_EDGE('',*,*,#20667,.T.);
#29428=ORIENTED_EDGE('',*,*,#20678,.T.);
#29429=ORIENTED_EDGE('',*,*,#20440,.T.);
#29430=ORIENTED_EDGE('',*,*,#20640,.F.);
#29431=ORIENTED_EDGE('',*,*,#20678,.F.);
#29432=ORIENTED_EDGE('',*,*,#20673,.F.);
#29433=ORIENTED_EDGE('',*,*,#20675,.F.);
#29434=ORIENTED_EDGE('',*,*,#20677,.F.);
#29435=ORIENTED_EDGE('',*,*,#20666,.F.);
#29436=ORIENTED_EDGE('',*,*,#20669,.F.);
#29437=ORIENTED_EDGE('',*,*,#20672,.T.);
#29438=ORIENTED_EDGE('',*,*,#20541,.F.);
#29439=ORIENTED_EDGE('',*,*,#20679,.T.);
#29440=ORIENTED_EDGE('',*,*,#20680,.T.);
#29441=ORIENTED_EDGE('',*,*,#20503,.F.);
#29442=ORIENTED_EDGE('',*,*,#20540,.F.);
#29443=ORIENTED_EDGE('',*,*,#20681,.T.);
#29444=ORIENTED_EDGE('',*,*,#20682,.F.);
#29445=ORIENTED_EDGE('',*,*,#20679,.F.);
#29446=ORIENTED_EDGE('',*,*,#20539,.F.);
#29447=ORIENTED_EDGE('',*,*,#20498,.T.);
#29448=ORIENTED_EDGE('',*,*,#20683,.T.);
#29449=ORIENTED_EDGE('',*,*,#20681,.F.);
#29450=ORIENTED_EDGE('',*,*,#20684,.T.);
#29451=ORIENTED_EDGE('',*,*,#20682,.T.);
#29452=ORIENTED_EDGE('',*,*,#20683,.F.);
#29453=ORIENTED_EDGE('',*,*,#20497,.F.);
#29454=ORIENTED_EDGE('',*,*,#20501,.F.);
#29455=ORIENTED_EDGE('',*,*,#20504,.F.);
#29456=ORIENTED_EDGE('',*,*,#20680,.F.);
#29457=ORIENTED_EDGE('',*,*,#20538,.T.);
#29458=ORIENTED_EDGE('',*,*,#20685,.T.);
#29459=ORIENTED_EDGE('',*,*,#20684,.F.);
#29460=ORIENTED_EDGE('',*,*,#20685,.F.);
#29461=ORIENTED_EDGE('',*,*,#20537,.T.);
#29462=ORIENTED_EDGE('',*,*,#20463,.T.);
#29463=ORIENTED_EDGE('',*,*,#20686,.T.);
#29464=ORIENTED_EDGE('',*,*,#20687,.F.);
#29465=ORIENTED_EDGE('',*,*,#20688,.F.);
#29466=ORIENTED_EDGE('',*,*,#20686,.F.);
#29467=ORIENTED_EDGE('',*,*,#20688,.T.);
#29468=ORIENTED_EDGE('',*,*,#20689,.T.);
#29469=ORIENTED_EDGE('',*,*,#20690,.F.);
#29470=ORIENTED_EDGE('',*,*,#20691,.F.);
#29471=ORIENTED_EDGE('',*,*,#20689,.F.);
#29472=ORIENTED_EDGE('',*,*,#20687,.T.);
#29473=ORIENTED_EDGE('',*,*,#20691,.T.);
#29474=ORIENTED_EDGE('',*,*,#20692,.T.);
#29475=ORIENTED_EDGE('',*,*,#20693,.F.);
#29476=ORIENTED_EDGE('',*,*,#20692,.F.);
#29477=ORIENTED_EDGE('',*,*,#20690,.T.);
#29478=ORIENTED_EDGE('',*,*,#20694,.T.);
#29479=ORIENTED_EDGE('',*,*,#20695,.F.);
#29480=ORIENTED_EDGE('',*,*,#20696,.F.);
#29481=ORIENTED_EDGE('',*,*,#20694,.F.);
#29482=ORIENTED_EDGE('',*,*,#20696,.T.);
#29483=ORIENTED_EDGE('',*,*,#20697,.T.);
#29484=ORIENTED_EDGE('',*,*,#20698,.F.);
#29485=ORIENTED_EDGE('',*,*,#20699,.F.);
#29486=ORIENTED_EDGE('',*,*,#20697,.F.);
#29487=ORIENTED_EDGE('',*,*,#20695,.T.);
#29488=ORIENTED_EDGE('',*,*,#20699,.T.);
#29489=ORIENTED_EDGE('',*,*,#20700,.T.);
#29490=ORIENTED_EDGE('',*,*,#20701,.F.);
#29491=ORIENTED_EDGE('',*,*,#20700,.F.);
#29492=ORIENTED_EDGE('',*,*,#20698,.T.);
#29493=ORIENTED_EDGE('',*,*,#20702,.T.);
#29494=ORIENTED_EDGE('',*,*,#20703,.F.);
#29495=ORIENTED_EDGE('',*,*,#20704,.F.);
#29496=ORIENTED_EDGE('',*,*,#20702,.F.);
#29497=ORIENTED_EDGE('',*,*,#20704,.T.);
#29498=ORIENTED_EDGE('',*,*,#20705,.T.);
#29499=ORIENTED_EDGE('',*,*,#20706,.F.);
#29500=ORIENTED_EDGE('',*,*,#20707,.F.);
#29501=ORIENTED_EDGE('',*,*,#20705,.F.);
#29502=ORIENTED_EDGE('',*,*,#20703,.T.);
#29503=ORIENTED_EDGE('',*,*,#20707,.T.);
#29504=ORIENTED_EDGE('',*,*,#20708,.T.);
#29505=ORIENTED_EDGE('',*,*,#20709,.F.);
#29506=ORIENTED_EDGE('',*,*,#20708,.F.);
#29507=ORIENTED_EDGE('',*,*,#20706,.T.);
#29508=ORIENTED_EDGE('',*,*,#20710,.F.);
#29509=ORIENTED_EDGE('',*,*,#20711,.F.);
#29510=ORIENTED_EDGE('',*,*,#20712,.T.);
#29511=ORIENTED_EDGE('',*,*,#20713,.T.);
#29512=ORIENTED_EDGE('',*,*,#20712,.F.);
#29513=ORIENTED_EDGE('',*,*,#20710,.T.);
#29514=ORIENTED_EDGE('',*,*,#20711,.T.);
#29515=ORIENTED_EDGE('',*,*,#20714,.T.);
#29516=ORIENTED_EDGE('',*,*,#20715,.F.);
#29517=ORIENTED_EDGE('',*,*,#20716,.F.);
#29518=ORIENTED_EDGE('',*,*,#20714,.F.);
#29519=ORIENTED_EDGE('',*,*,#20717,.T.);
#29520=ORIENTED_EDGE('',*,*,#20715,.T.);
#29521=ORIENTED_EDGE('',*,*,#20716,.T.);
#29522=ORIENTED_EDGE('',*,*,#20717,.F.);
#29523=ORIENTED_EDGE('',*,*,#20718,.F.);
#29524=ORIENTED_EDGE('',*,*,#20719,.F.);
#29525=ORIENTED_EDGE('',*,*,#20720,.T.);
#29526=ORIENTED_EDGE('',*,*,#20721,.T.);
#29527=ORIENTED_EDGE('',*,*,#20720,.F.);
#29528=ORIENTED_EDGE('',*,*,#20718,.T.);
#29529=ORIENTED_EDGE('',*,*,#20719,.T.);
#29530=ORIENTED_EDGE('',*,*,#20722,.T.);
#29531=ORIENTED_EDGE('',*,*,#20723,.F.);
#29532=ORIENTED_EDGE('',*,*,#20724,.F.);
#29533=ORIENTED_EDGE('',*,*,#20722,.F.);
#29534=ORIENTED_EDGE('',*,*,#20725,.T.);
#29535=ORIENTED_EDGE('',*,*,#20723,.T.);
#29536=ORIENTED_EDGE('',*,*,#20724,.T.);
#29537=ORIENTED_EDGE('',*,*,#20725,.F.);
#29538=ORIENTED_EDGE('',*,*,#20726,.F.);
#29539=ORIENTED_EDGE('',*,*,#20727,.F.);
#29540=ORIENTED_EDGE('',*,*,#20728,.T.);
#29541=ORIENTED_EDGE('',*,*,#20729,.T.);
#29542=ORIENTED_EDGE('',*,*,#20728,.F.);
#29543=ORIENTED_EDGE('',*,*,#20726,.T.);
#29544=ORIENTED_EDGE('',*,*,#20727,.T.);
#29545=ORIENTED_EDGE('',*,*,#20730,.T.);
#29546=ORIENTED_EDGE('',*,*,#20731,.F.);
#29547=ORIENTED_EDGE('',*,*,#20732,.F.);
#29548=ORIENTED_EDGE('',*,*,#20730,.F.);
#29549=ORIENTED_EDGE('',*,*,#20733,.T.);
#29550=ORIENTED_EDGE('',*,*,#20731,.T.);
#29551=ORIENTED_EDGE('',*,*,#20732,.T.);
#29552=ORIENTED_EDGE('',*,*,#20733,.F.);
#29553=ORIENTED_EDGE('',*,*,#20734,.F.);
#29554=ORIENTED_EDGE('',*,*,#20735,.F.);
#29555=ORIENTED_EDGE('',*,*,#20736,.T.);
#29556=ORIENTED_EDGE('',*,*,#20737,.T.);
#29557=ORIENTED_EDGE('',*,*,#20736,.F.);
#29558=ORIENTED_EDGE('',*,*,#20734,.T.);
#29559=ORIENTED_EDGE('',*,*,#20735,.T.);
#29560=ORIENTED_EDGE('',*,*,#20738,.T.);
#29561=ORIENTED_EDGE('',*,*,#20739,.F.);
#29562=ORIENTED_EDGE('',*,*,#20740,.F.);
#29563=ORIENTED_EDGE('',*,*,#20738,.F.);
#29564=ORIENTED_EDGE('',*,*,#20741,.T.);
#29565=ORIENTED_EDGE('',*,*,#20739,.T.);
#29566=ORIENTED_EDGE('',*,*,#20740,.T.);
#29567=ORIENTED_EDGE('',*,*,#20741,.F.);
#29568=ORIENTED_EDGE('',*,*,#20742,.T.);
#29569=ORIENTED_EDGE('',*,*,#20454,.T.);
#29570=ORIENTED_EDGE('',*,*,#20455,.T.);
#29571=ORIENTED_EDGE('',*,*,#20742,.F.);
#29572=ORIENTED_EDGE('',*,*,#20743,.T.);
#29573=ORIENTED_EDGE('',*,*,#20418,.T.);
#29574=ORIENTED_EDGE('',*,*,#20419,.T.);
#29575=ORIENTED_EDGE('',*,*,#20743,.F.);
#29576=ORIENTED_EDGE('',*,*,#20744,.T.);
#29577=ORIENTED_EDGE('',*,*,#20511,.F.);
#29578=ORIENTED_EDGE('',*,*,#20512,.F.);
#29579=ORIENTED_EDGE('',*,*,#20744,.F.);
#29580=ORIENTED_EDGE('',*,*,#20745,.T.);
#29581=ORIENTED_EDGE('',*,*,#20515,.F.);
#29582=ORIENTED_EDGE('',*,*,#20516,.F.);
#29583=ORIENTED_EDGE('',*,*,#20745,.F.);
#29584=ORIENTED_EDGE('',*,*,#20746,.T.);
#29585=ORIENTED_EDGE('',*,*,#20519,.F.);
#29586=ORIENTED_EDGE('',*,*,#20520,.F.);
#29587=ORIENTED_EDGE('',*,*,#20746,.F.);
#29588=ORIENTED_EDGE('',*,*,#20747,.T.);
#29589=ORIENTED_EDGE('',*,*,#20523,.F.);
#29590=ORIENTED_EDGE('',*,*,#20524,.F.);
#29591=ORIENTED_EDGE('',*,*,#20747,.F.);
#29592=ORIENTED_EDGE('',*,*,#20748,.T.);
#29593=ORIENTED_EDGE('',*,*,#20432,.T.);
#29594=ORIENTED_EDGE('',*,*,#20433,.T.);
#29595=ORIENTED_EDGE('',*,*,#20748,.F.);
#29596=ORIENTED_EDGE('',*,*,#20749,.T.);
#29597=ORIENTED_EDGE('',*,*,#20447,.T.);
#29598=ORIENTED_EDGE('',*,*,#20448,.T.);
#29599=ORIENTED_EDGE('',*,*,#20749,.F.);
#29600=ORIENTED_EDGE('',*,*,#20750,.T.);
#29601=ORIENTED_EDGE('',*,*,#20443,.T.);
#29602=ORIENTED_EDGE('',*,*,#20751,.F.);
#29603=ORIENTED_EDGE('',*,*,#20752,.F.);
#29604=ORIENTED_EDGE('',*,*,#20751,.T.);
#29605=ORIENTED_EDGE('',*,*,#20442,.T.);
#29606=ORIENTED_EDGE('',*,*,#20753,.F.);
#29607=ORIENTED_EDGE('',*,*,#20754,.F.);
#29608=ORIENTED_EDGE('',*,*,#20755,.T.);
#29609=ORIENTED_EDGE('',*,*,#20535,.T.);
#29610=ORIENTED_EDGE('',*,*,#20756,.F.);
#29611=ORIENTED_EDGE('',*,*,#20757,.F.);
#29612=ORIENTED_EDGE('',*,*,#20753,.T.);
#29613=ORIENTED_EDGE('',*,*,#20459,.T.);
#29614=ORIENTED_EDGE('',*,*,#20758,.F.);
#29615=ORIENTED_EDGE('',*,*,#20759,.F.);
#29616=ORIENTED_EDGE('',*,*,#20758,.T.);
#29617=ORIENTED_EDGE('',*,*,#20458,.T.);
#29618=ORIENTED_EDGE('',*,*,#20760,.F.);
#29619=ORIENTED_EDGE('',*,*,#20761,.F.);
#29620=ORIENTED_EDGE('',*,*,#20760,.T.);
#29621=ORIENTED_EDGE('',*,*,#20457,.T.);
#29622=ORIENTED_EDGE('',*,*,#20530,.T.);
#29623=ORIENTED_EDGE('',*,*,#20762,.F.);
#29624=ORIENTED_EDGE('',*,*,#20763,.F.);
#29625=ORIENTED_EDGE('',*,*,#20762,.T.);
#29626=ORIENTED_EDGE('',*,*,#20529,.T.);
#29627=ORIENTED_EDGE('',*,*,#20764,.F.);
#29628=ORIENTED_EDGE('',*,*,#20765,.F.);
#29629=ORIENTED_EDGE('',*,*,#20764,.T.);
#29630=ORIENTED_EDGE('',*,*,#20528,.T.);
#29631=ORIENTED_EDGE('',*,*,#20755,.F.);
#29632=ORIENTED_EDGE('',*,*,#20766,.F.);
#29633=ORIENTED_EDGE('',*,*,#20767,.T.);
#29634=ORIENTED_EDGE('',*,*,#20768,.T.);
#29635=ORIENTED_EDGE('',*,*,#20752,.T.);
#29636=ORIENTED_EDGE('',*,*,#20754,.T.);
#29637=ORIENTED_EDGE('',*,*,#20759,.T.);
#29638=ORIENTED_EDGE('',*,*,#20761,.T.);
#29639=ORIENTED_EDGE('',*,*,#20763,.T.);
#29640=ORIENTED_EDGE('',*,*,#20765,.T.);
#29641=ORIENTED_EDGE('',*,*,#20766,.T.);
#29642=ORIENTED_EDGE('',*,*,#20757,.T.);
#29643=ORIENTED_EDGE('',*,*,#20769,.T.);
#29644=ORIENTED_EDGE('',*,*,#20770,.T.);
#29645=ORIENTED_EDGE('',*,*,#20771,.T.);
#29646=ORIENTED_EDGE('',*,*,#20772,.T.);
#29647=ORIENTED_EDGE('',*,*,#20773,.T.);
#29648=ORIENTED_EDGE('',*,*,#20774,.T.);
#29649=ORIENTED_EDGE('',*,*,#20775,.T.);
#29650=ORIENTED_EDGE('',*,*,#20776,.T.);
#29651=ORIENTED_EDGE('',*,*,#20777,.T.);
#29652=ORIENTED_EDGE('',*,*,#20778,.F.);
#29653=ORIENTED_EDGE('',*,*,#20778,.T.);
#29654=ORIENTED_EDGE('',*,*,#20779,.T.);
#29655=ORIENTED_EDGE('',*,*,#20780,.T.);
#29656=ORIENTED_EDGE('',*,*,#20779,.F.);
#29657=ORIENTED_EDGE('',*,*,#20781,.T.);
#29658=ORIENTED_EDGE('',*,*,#20782,.T.);
#29659=ORIENTED_EDGE('',*,*,#20783,.F.);
#29660=ORIENTED_EDGE('',*,*,#20782,.F.);
#29661=ORIENTED_EDGE('',*,*,#20784,.T.);
#29662=ORIENTED_EDGE('',*,*,#20483,.T.);
#29663=ORIENTED_EDGE('',*,*,#20531,.T.);
#29664=ORIENTED_EDGE('',*,*,#20456,.T.);
#29665=ORIENTED_EDGE('',*,*,#20451,.T.);
#29666=ORIENTED_EDGE('',*,*,#20357,.T.);
#29667=ORIENTED_EDGE('',*,*,#20637,.T.);
#29668=ORIENTED_EDGE('',*,*,#20412,.T.);
#29669=ORIENTED_EDGE('',*,*,#20636,.T.);
#29670=ORIENTED_EDGE('',*,*,#20464,.T.);
#29671=ORIENTED_EDGE('',*,*,#20536,.T.);
#29672=ORIENTED_EDGE('',*,*,#20462,.T.);
#29673=ORIENTED_EDGE('',*,*,#20449,.T.);
#29674=ORIENTED_EDGE('',*,*,#20445,.T.);
#29675=ORIENTED_EDGE('',*,*,#20532,.T.);
#29676=ORIENTED_EDGE('',*,*,#20480,.T.);
#29677=ORIENTED_EDGE('',*,*,#20505,.T.);
#29678=ORIENTED_EDGE('',*,*,#20514,.T.);
#29679=ORIENTED_EDGE('',*,*,#20518,.T.);
#29680=ORIENTED_EDGE('',*,*,#20522,.T.);
#29681=ORIENTED_EDGE('',*,*,#20526,.T.);
#29682=ORIENTED_EDGE('',*,*,#20391,.F.);
#29683=ORIENTED_EDGE('',*,*,#20369,.T.);
#29684=ORIENTED_EDGE('',*,*,#20623,.T.);
#29685=ORIENTED_EDGE('',*,*,#20785,.T.);
#29686=ORIENTED_EDGE('',*,*,#20393,.F.);
#29687=ORIENTED_EDGE('',*,*,#20400,.T.);
#29688=ORIENTED_EDGE('',*,*,#20473,.T.);
#29689=ORIENTED_EDGE('',*,*,#20786,.F.);
#29690=ORIENTED_EDGE('',*,*,#20787,.F.);
#29691=ORIENTED_EDGE('',*,*,#20786,.T.);
#29692=ORIENTED_EDGE('',*,*,#20472,.T.);
#29693=ORIENTED_EDGE('',*,*,#20788,.F.);
#29694=ORIENTED_EDGE('',*,*,#20789,.F.);
#29695=ORIENTED_EDGE('',*,*,#20788,.T.);
#29696=ORIENTED_EDGE('',*,*,#20471,.T.);
#29697=ORIENTED_EDGE('',*,*,#20790,.F.);
#29698=ORIENTED_EDGE('',*,*,#20791,.F.);
#29699=ORIENTED_EDGE('',*,*,#20790,.T.);
#29700=ORIENTED_EDGE('',*,*,#20470,.T.);
#29701=ORIENTED_EDGE('',*,*,#20792,.F.);
#29702=ORIENTED_EDGE('',*,*,#20793,.F.);
#29703=ORIENTED_EDGE('',*,*,#20792,.T.);
#29704=ORIENTED_EDGE('',*,*,#20469,.T.);
#29705=ORIENTED_EDGE('',*,*,#20794,.F.);
#29706=ORIENTED_EDGE('',*,*,#20795,.F.);
#29707=ORIENTED_EDGE('',*,*,#20794,.T.);
#29708=ORIENTED_EDGE('',*,*,#20468,.T.);
#29709=ORIENTED_EDGE('',*,*,#20622,.F.);
#29710=ORIENTED_EDGE('',*,*,#20796,.F.);
#29711=ORIENTED_EDGE('',*,*,#20621,.T.);
#29712=ORIENTED_EDGE('',*,*,#20401,.T.);
#29713=ORIENTED_EDGE('',*,*,#20787,.T.);
#29714=ORIENTED_EDGE('',*,*,#20789,.T.);
#29715=ORIENTED_EDGE('',*,*,#20791,.T.);
#29716=ORIENTED_EDGE('',*,*,#20793,.T.);
#29717=ORIENTED_EDGE('',*,*,#20795,.T.);
#29718=ORIENTED_EDGE('',*,*,#20796,.T.);
#29719=ORIENTED_EDGE('',*,*,#20713,.F.);
#29720=ORIENTED_EDGE('',*,*,#20721,.F.);
#29721=ORIENTED_EDGE('',*,*,#20729,.F.);
#29722=ORIENTED_EDGE('',*,*,#20737,.F.);
#29723=ORIENTED_EDGE('',*,*,#20783,.T.);
#29724=ORIENTED_EDGE('',*,*,#20797,.T.);
#29725=ORIENTED_EDGE('',*,*,#20533,.T.);
#29726=ORIENTED_EDGE('',*,*,#20444,.T.);
#29727=ORIENTED_EDGE('',*,*,#20750,.F.);
#29728=ORIENTED_EDGE('',*,*,#20768,.F.);
#29729=ORIENTED_EDGE('',*,*,#20756,.T.);
#29730=ORIENTED_EDGE('',*,*,#20534,.T.);
#29731=ORIENTED_EDGE('',*,*,#20797,.F.);
#29732=ORIENTED_EDGE('',*,*,#20767,.F.);
#29733=ORIENTED_EDGE('',*,*,#20410,.T.);
#29734=ORIENTED_EDGE('',*,*,#20387,.F.);
#29735=ORIENTED_EDGE('',*,*,#20466,.T.);
#29736=ORIENTED_EDGE('',*,*,#20635,.T.);
#29737=ORIENTED_EDGE('',*,*,#20798,.F.);
#29738=ORIENTED_EDGE('',*,*,#20799,.F.);
#29739=ORIENTED_EDGE('',*,*,#20800,.T.);
#29740=ORIENTED_EDGE('',*,*,#20801,.T.);
#29741=ORIENTED_EDGE('',*,*,#20800,.F.);
#29742=ORIENTED_EDGE('',*,*,#20415,.T.);
#29743=ORIENTED_EDGE('',*,*,#20802,.T.);
#29744=ORIENTED_EDGE('',*,*,#20803,.F.);
#29745=ORIENTED_EDGE('',*,*,#20804,.F.);
#29746=ORIENTED_EDGE('',*,*,#20805,.F.);
#29747=ORIENTED_EDGE('',*,*,#20802,.F.);
#29748=ORIENTED_EDGE('',*,*,#20478,.T.);
#29749=ORIENTED_EDGE('',*,*,#20806,.T.);
#29750=ORIENTED_EDGE('',*,*,#20807,.F.);
#29751=ORIENTED_EDGE('',*,*,#20806,.F.);
#29752=ORIENTED_EDGE('',*,*,#20477,.T.);
#29753=ORIENTED_EDGE('',*,*,#20798,.T.);
#29754=ORIENTED_EDGE('',*,*,#20799,.T.);
#29755=ORIENTED_EDGE('',*,*,#20808,.T.);
#29756=ORIENTED_EDGE('',*,*,#20804,.T.);
#29757=ORIENTED_EDGE('',*,*,#20809,.T.);
#29758=ORIENTED_EDGE('',*,*,#20777,.F.);
#29759=ORIENTED_EDGE('',*,*,#20809,.F.);
#29760=ORIENTED_EDGE('',*,*,#20803,.T.);
#29761=ORIENTED_EDGE('',*,*,#20805,.T.);
#29762=ORIENTED_EDGE('',*,*,#20808,.F.);
#29763=ORIENTED_EDGE('',*,*,#20405,.T.);
#29764=ORIENTED_EDGE('',*,*,#20378,.F.);
#29765=ORIENTED_EDGE('',*,*,#20396,.T.);
#29766=ORIENTED_EDGE('',*,*,#20361,.T.);
#29767=ORIENTED_EDGE('',*,*,#20420,.T.);
#29768=ORIENTED_EDGE('',*,*,#20409,.T.);
#29769=ORIENTED_EDGE('',*,*,#20435,.T.);
#29770=ORIENTED_EDGE('',*,*,#20474,.T.);
#29771=ORIENTED_EDGE('',*,*,#20398,.T.);
#29772=ORIENTED_EDGE('',*,*,#20404,.T.);
#29773=ORIENTED_EDGE('',*,*,#20810,.T.);
#29774=ORIENTED_EDGE('',*,*,#20811,.T.);
#29775=ORIENTED_EDGE('',*,*,#20812,.T.);
#29776=ORIENTED_EDGE('',*,*,#20811,.F.);
#29777=ORIENTED_EDGE('',*,*,#20813,.T.);
#29778=ORIENTED_EDGE('',*,*,#20814,.T.);
#29779=ORIENTED_EDGE('',*,*,#20815,.T.);
#29780=ORIENTED_EDGE('',*,*,#20816,.F.);
#29781=ORIENTED_EDGE('',*,*,#20815,.F.);
#29782=ORIENTED_EDGE('',*,*,#20785,.F.);
#29783=ORIENTED_EDGE('',*,*,#20625,.F.);
#29784=ORIENTED_EDGE('',*,*,#20627,.F.);
#29785=ORIENTED_EDGE('',*,*,#20629,.F.);
#29786=ORIENTED_EDGE('',*,*,#20631,.F.);
#29787=ORIENTED_EDGE('',*,*,#20633,.F.);
#29788=ORIENTED_EDGE('',*,*,#20634,.F.);
#29789=ORIENTED_EDGE('',*,*,#20394,.F.);
#29790=ORIENTED_EDGE('',*,*,#20553,.T.);
#29791=ORIENTED_EDGE('',*,*,#20581,.T.);
#29792=ORIENTED_EDGE('',*,*,#20583,.T.);
#29793=ORIENTED_EDGE('',*,*,#20568,.T.);
#29794=ORIENTED_EDGE('',*,*,#20563,.T.);
#29795=ORIENTED_EDGE('',*,*,#20558,.T.);
#29796=ORIENTED_EDGE('',*,*,#20817,.T.);
#29797=ORIENTED_EDGE('',*,*,#20818,.T.);
#29798=ORIENTED_EDGE('',*,*,#20819,.T.);
#29799=ORIENTED_EDGE('',*,*,#20820,.T.);
#29800=ORIENTED_EDGE('',*,*,#20821,.T.);
#29801=ORIENTED_EDGE('',*,*,#20822,.T.);
#29802=ORIENTED_EDGE('',*,*,#20589,.T.);
#29803=ORIENTED_EDGE('',*,*,#20617,.T.);
#29804=ORIENTED_EDGE('',*,*,#20619,.T.);
#29805=ORIENTED_EDGE('',*,*,#20604,.T.);
#29806=ORIENTED_EDGE('',*,*,#20599,.T.);
#29807=ORIENTED_EDGE('',*,*,#20594,.T.);
#29808=ORIENTED_EDGE('',*,*,#20823,.T.);
#29809=ORIENTED_EDGE('',*,*,#20824,.T.);
#29810=ORIENTED_EDGE('',*,*,#20825,.T.);
#29811=ORIENTED_EDGE('',*,*,#20826,.T.);
#29812=ORIENTED_EDGE('',*,*,#20827,.T.);
#29813=ORIENTED_EDGE('',*,*,#20828,.T.);
#29814=ORIENTED_EDGE('',*,*,#20816,.T.);
#29815=ORIENTED_EDGE('',*,*,#20829,.T.);
#29816=ORIENTED_EDGE('',*,*,#20810,.F.);
#29817=ORIENTED_EDGE('',*,*,#20830,.F.);
#29818=ORIENTED_EDGE('',*,*,#20831,.T.);
#29819=ORIENTED_EDGE('',*,*,#20829,.F.);
#29820=ORIENTED_EDGE('',*,*,#20831,.F.);
#29821=ORIENTED_EDGE('',*,*,#20801,.F.);
#29822=ORIENTED_EDGE('',*,*,#20830,.T.);
#29823=ORIENTED_EDGE('',*,*,#20832,.T.);
#29824=ORIENTED_EDGE('',*,*,#20833,.T.);
#29825=ORIENTED_EDGE('',*,*,#20834,.T.);
#29826=ORIENTED_EDGE('',*,*,#20835,.F.);
#29827=ORIENTED_EDGE('',*,*,#20834,.F.);
#29828=ORIENTED_EDGE('',*,*,#20836,.T.);
#29829=ORIENTED_EDGE('',*,*,#20837,.T.);
#29830=ORIENTED_EDGE('',*,*,#20838,.T.);
#29831=ORIENTED_EDGE('',*,*,#20839,.F.);
#29832=ORIENTED_EDGE('',*,*,#20838,.F.);
#29833=ORIENTED_EDGE('',*,*,#20839,.T.);
#29834=ORIENTED_EDGE('',*,*,#20840,.F.);
#29835=ORIENTED_EDGE('',*,*,#20841,.T.);
#29836=ORIENTED_EDGE('',*,*,#20842,.F.);
#29837=ORIENTED_EDGE('',*,*,#20843,.F.);
#29838=ORIENTED_EDGE('',*,*,#20844,.F.);
#29839=ORIENTED_EDGE('',*,*,#20845,.T.);
#29840=ORIENTED_EDGE('',*,*,#20842,.T.);
#29841=ORIENTED_EDGE('',*,*,#20846,.T.);
#29842=ORIENTED_EDGE('',*,*,#20847,.F.);
#29843=ORIENTED_EDGE('',*,*,#20548,.T.);
#29844=ORIENTED_EDGE('',*,*,#20844,.T.);
#29845=ORIENTED_EDGE('',*,*,#20848,.T.);
#29846=ORIENTED_EDGE('',*,*,#20849,.F.);
#29847=ORIENTED_EDGE('',*,*,#20850,.T.);
#29848=ORIENTED_EDGE('',*,*,#20851,.T.);
#29849=ORIENTED_EDGE('',*,*,#20852,.T.);
#29850=ORIENTED_EDGE('',*,*,#20853,.T.);
#29851=ORIENTED_EDGE('',*,*,#20854,.T.);
#29852=ORIENTED_EDGE('',*,*,#20855,.T.);
#29853=ORIENTED_EDGE('',*,*,#20856,.F.);
#29854=ORIENTED_EDGE('',*,*,#20855,.F.);
#29855=ORIENTED_EDGE('',*,*,#20542,.F.);
#29856=ORIENTED_EDGE('',*,*,#20857,.F.);
#29857=ORIENTED_EDGE('',*,*,#20840,.T.);
#29858=ORIENTED_EDGE('',*,*,#20858,.T.);
#29859=ORIENTED_EDGE('',*,*,#20835,.T.);
#29860=ORIENTED_EDGE('',*,*,#20856,.T.);
#29861=ORIENTED_EDGE('',*,*,#20859,.T.);
#29862=ORIENTED_EDGE('',*,*,#20860,.T.);
#29863=ORIENTED_EDGE('',*,*,#20861,.T.);
#29864=ORIENTED_EDGE('',*,*,#20862,.T.);
#29865=ORIENTED_EDGE('',*,*,#20863,.T.);
#29866=ORIENTED_EDGE('',*,*,#20864,.T.);
#29867=ORIENTED_EDGE('',*,*,#20865,.T.);
#29868=ORIENTED_EDGE('',*,*,#20866,.F.);
#29869=ORIENTED_EDGE('',*,*,#20864,.F.);
#29870=ORIENTED_EDGE('',*,*,#20867,.T.);
#29871=ORIENTED_EDGE('',*,*,#20868,.T.);
#29872=ORIENTED_EDGE('',*,*,#20867,.F.);
#29873=ORIENTED_EDGE('',*,*,#20863,.F.);
#29874=ORIENTED_EDGE('',*,*,#20869,.T.);
#29875=ORIENTED_EDGE('',*,*,#20870,.T.);
#29876=ORIENTED_EDGE('',*,*,#20871,.F.);
#29877=ORIENTED_EDGE('',*,*,#20869,.F.);
#29878=ORIENTED_EDGE('',*,*,#20862,.F.);
#29879=ORIENTED_EDGE('',*,*,#20872,.T.);
#29880=ORIENTED_EDGE('',*,*,#20870,.F.);
#29881=ORIENTED_EDGE('',*,*,#20861,.F.);
#29882=ORIENTED_EDGE('',*,*,#20873,.T.);
#29883=ORIENTED_EDGE('',*,*,#20874,.T.);
#29884=ORIENTED_EDGE('',*,*,#20873,.F.);
#29885=ORIENTED_EDGE('',*,*,#20860,.F.);
#29886=ORIENTED_EDGE('',*,*,#20875,.T.);
#29887=ORIENTED_EDGE('',*,*,#20876,.T.);
#29888=ORIENTED_EDGE('',*,*,#20875,.F.);
#29889=ORIENTED_EDGE('',*,*,#20859,.F.);
#29890=ORIENTED_EDGE('',*,*,#20866,.T.);
#29891=ORIENTED_EDGE('',*,*,#20877,.T.);
#29892=ORIENTED_EDGE('',*,*,#20878,.T.);
#29893=ORIENTED_EDGE('',*,*,#20879,.T.);
#29894=ORIENTED_EDGE('',*,*,#20880,.T.);
#29895=ORIENTED_EDGE('',*,*,#20881,.T.);
#29896=ORIENTED_EDGE('',*,*,#20882,.T.);
#29897=ORIENTED_EDGE('',*,*,#20883,.T.);
#29898=ORIENTED_EDGE('',*,*,#20884,.F.);
#29899=ORIENTED_EDGE('',*,*,#20882,.F.);
#29900=ORIENTED_EDGE('',*,*,#20885,.T.);
#29901=ORIENTED_EDGE('',*,*,#20886,.T.);
#29902=ORIENTED_EDGE('',*,*,#20885,.F.);
#29903=ORIENTED_EDGE('',*,*,#20881,.F.);
#29904=ORIENTED_EDGE('',*,*,#20887,.T.);
#29905=ORIENTED_EDGE('',*,*,#20888,.T.);
#29906=ORIENTED_EDGE('',*,*,#20889,.F.);
#29907=ORIENTED_EDGE('',*,*,#20887,.F.);
#29908=ORIENTED_EDGE('',*,*,#20880,.F.);
#29909=ORIENTED_EDGE('',*,*,#20890,.T.);
#29910=ORIENTED_EDGE('',*,*,#20888,.F.);
#29911=ORIENTED_EDGE('',*,*,#20879,.F.);
#29912=ORIENTED_EDGE('',*,*,#20891,.T.);
#29913=ORIENTED_EDGE('',*,*,#20892,.T.);
#29914=ORIENTED_EDGE('',*,*,#20891,.F.);
#29915=ORIENTED_EDGE('',*,*,#20878,.F.);
#29916=ORIENTED_EDGE('',*,*,#20893,.T.);
#29917=ORIENTED_EDGE('',*,*,#20894,.T.);
#29918=ORIENTED_EDGE('',*,*,#20893,.F.);
#29919=ORIENTED_EDGE('',*,*,#20877,.F.);
#29920=ORIENTED_EDGE('',*,*,#20884,.T.);
#29921=ORIENTED_EDGE('',*,*,#20895,.T.);
#29922=ORIENTED_EDGE('',*,*,#20871,.T.);
#29923=ORIENTED_EDGE('',*,*,#20872,.F.);
#29924=ORIENTED_EDGE('',*,*,#20874,.F.);
#29925=ORIENTED_EDGE('',*,*,#20876,.F.);
#29926=ORIENTED_EDGE('',*,*,#20865,.F.);
#29927=ORIENTED_EDGE('',*,*,#20868,.F.);
#29928=ORIENTED_EDGE('',*,*,#20896,.T.);
#29929=ORIENTED_EDGE('',*,*,#20897,.T.);
#29930=ORIENTED_EDGE('',*,*,#20898,.T.);
#29931=ORIENTED_EDGE('',*,*,#20895,.F.);
#29932=ORIENTED_EDGE('',*,*,#20898,.F.);
#29933=ORIENTED_EDGE('',*,*,#20899,.F.);
#29934=ORIENTED_EDGE('',*,*,#20900,.T.);
#29935=ORIENTED_EDGE('',*,*,#20896,.F.);
#29936=ORIENTED_EDGE('',*,*,#20897,.F.);
#29937=ORIENTED_EDGE('',*,*,#20900,.F.);
#29938=ORIENTED_EDGE('',*,*,#20901,.F.);
#29939=ORIENTED_EDGE('',*,*,#20902,.F.);
#29940=ORIENTED_EDGE('',*,*,#20903,.T.);
#29941=ORIENTED_EDGE('',*,*,#20904,.T.);
#29942=ORIENTED_EDGE('',*,*,#20903,.F.);
#29943=ORIENTED_EDGE('',*,*,#20904,.F.);
#29944=ORIENTED_EDGE('',*,*,#20905,.T.);
#29945=ORIENTED_EDGE('',*,*,#20889,.T.);
#29946=ORIENTED_EDGE('',*,*,#20890,.F.);
#29947=ORIENTED_EDGE('',*,*,#20892,.F.);
#29948=ORIENTED_EDGE('',*,*,#20894,.F.);
#29949=ORIENTED_EDGE('',*,*,#20883,.F.);
#29950=ORIENTED_EDGE('',*,*,#20886,.F.);
#29951=ORIENTED_EDGE('',*,*,#20906,.T.);
#29952=ORIENTED_EDGE('',*,*,#20907,.T.);
#29953=ORIENTED_EDGE('',*,*,#20908,.T.);
#29954=ORIENTED_EDGE('',*,*,#20905,.F.);
#29955=ORIENTED_EDGE('',*,*,#20908,.F.);
#29956=ORIENTED_EDGE('',*,*,#20909,.T.);
#29957=ORIENTED_EDGE('',*,*,#20910,.T.);
#29958=ORIENTED_EDGE('',*,*,#20911,.T.);
#29959=ORIENTED_EDGE('',*,*,#20912,.T.);
#29960=ORIENTED_EDGE('',*,*,#20913,.T.);
#29961=ORIENTED_EDGE('',*,*,#20914,.T.);
#29962=ORIENTED_EDGE('',*,*,#20915,.T.);
#29963=ORIENTED_EDGE('',*,*,#20916,.F.);
#29964=ORIENTED_EDGE('',*,*,#20914,.F.);
#29965=ORIENTED_EDGE('',*,*,#20917,.T.);
#29966=ORIENTED_EDGE('',*,*,#20918,.T.);
#29967=ORIENTED_EDGE('',*,*,#20917,.F.);
#29968=ORIENTED_EDGE('',*,*,#20913,.F.);
#29969=ORIENTED_EDGE('',*,*,#20919,.T.);
#29970=ORIENTED_EDGE('',*,*,#20920,.T.);
#29971=ORIENTED_EDGE('',*,*,#20921,.F.);
#29972=ORIENTED_EDGE('',*,*,#20919,.F.);
#29973=ORIENTED_EDGE('',*,*,#20912,.F.);
#29974=ORIENTED_EDGE('',*,*,#20922,.T.);
#29975=ORIENTED_EDGE('',*,*,#20920,.F.);
#29976=ORIENTED_EDGE('',*,*,#20911,.F.);
#29977=ORIENTED_EDGE('',*,*,#20923,.T.);
#29978=ORIENTED_EDGE('',*,*,#20924,.T.);
#29979=ORIENTED_EDGE('',*,*,#20923,.F.);
#29980=ORIENTED_EDGE('',*,*,#20910,.F.);
#29981=ORIENTED_EDGE('',*,*,#20925,.T.);
#29982=ORIENTED_EDGE('',*,*,#20926,.T.);
#29983=ORIENTED_EDGE('',*,*,#20925,.F.);
#29984=ORIENTED_EDGE('',*,*,#20909,.F.);
#29985=ORIENTED_EDGE('',*,*,#20916,.T.);
#29986=ORIENTED_EDGE('',*,*,#20927,.T.);
#29987=ORIENTED_EDGE('',*,*,#20928,.T.);
#29988=ORIENTED_EDGE('',*,*,#20929,.T.);
#29989=ORIENTED_EDGE('',*,*,#20930,.T.);
#29990=ORIENTED_EDGE('',*,*,#20931,.T.);
#29991=ORIENTED_EDGE('',*,*,#20932,.T.);
#29992=ORIENTED_EDGE('',*,*,#20933,.T.);
#29993=ORIENTED_EDGE('',*,*,#20934,.F.);
#29994=ORIENTED_EDGE('',*,*,#20932,.F.);
#29995=ORIENTED_EDGE('',*,*,#20935,.T.);
#29996=ORIENTED_EDGE('',*,*,#20936,.T.);
#29997=ORIENTED_EDGE('',*,*,#20935,.F.);
#29998=ORIENTED_EDGE('',*,*,#20931,.F.);
#29999=ORIENTED_EDGE('',*,*,#20937,.T.);
#30000=ORIENTED_EDGE('',*,*,#20938,.T.);
#30001=ORIENTED_EDGE('',*,*,#20939,.F.);
#30002=ORIENTED_EDGE('',*,*,#20937,.F.);
#30003=ORIENTED_EDGE('',*,*,#20930,.F.);
#30004=ORIENTED_EDGE('',*,*,#20940,.T.);
#30005=ORIENTED_EDGE('',*,*,#20938,.F.);
#30006=ORIENTED_EDGE('',*,*,#20929,.F.);
#30007=ORIENTED_EDGE('',*,*,#20941,.T.);
#30008=ORIENTED_EDGE('',*,*,#20942,.T.);
#30009=ORIENTED_EDGE('',*,*,#20941,.F.);
#30010=ORIENTED_EDGE('',*,*,#20928,.F.);
#30011=ORIENTED_EDGE('',*,*,#20943,.T.);
#30012=ORIENTED_EDGE('',*,*,#20944,.T.);
#30013=ORIENTED_EDGE('',*,*,#20943,.F.);
#30014=ORIENTED_EDGE('',*,*,#20927,.F.);
#30015=ORIENTED_EDGE('',*,*,#20934,.T.);
#30016=ORIENTED_EDGE('',*,*,#20945,.T.);
#30017=ORIENTED_EDGE('',*,*,#20939,.T.);
#30018=ORIENTED_EDGE('',*,*,#20940,.F.);
#30019=ORIENTED_EDGE('',*,*,#20942,.F.);
#30020=ORIENTED_EDGE('',*,*,#20944,.F.);
#30021=ORIENTED_EDGE('',*,*,#20933,.F.);
#30022=ORIENTED_EDGE('',*,*,#20936,.F.);
#30023=ORIENTED_EDGE('',*,*,#20946,.T.);
#30024=ORIENTED_EDGE('',*,*,#20947,.T.);
#30025=ORIENTED_EDGE('',*,*,#20948,.T.);
#30026=ORIENTED_EDGE('',*,*,#20945,.F.);
#30027=ORIENTED_EDGE('',*,*,#20948,.F.);
#30028=ORIENTED_EDGE('',*,*,#20949,.F.);
#30029=ORIENTED_EDGE('',*,*,#20950,.T.);
#30030=ORIENTED_EDGE('',*,*,#20946,.F.);
#30031=ORIENTED_EDGE('',*,*,#20947,.F.);
#30032=ORIENTED_EDGE('',*,*,#20950,.F.);
#30033=ORIENTED_EDGE('',*,*,#20951,.F.);
#30034=ORIENTED_EDGE('',*,*,#20952,.F.);
#30035=ORIENTED_EDGE('',*,*,#20953,.T.);
#30036=ORIENTED_EDGE('',*,*,#20954,.T.);
#30037=ORIENTED_EDGE('',*,*,#20953,.F.);
#30038=ORIENTED_EDGE('',*,*,#20954,.F.);
#30039=ORIENTED_EDGE('',*,*,#20955,.T.);
#30040=ORIENTED_EDGE('',*,*,#20921,.T.);
#30041=ORIENTED_EDGE('',*,*,#20922,.F.);
#30042=ORIENTED_EDGE('',*,*,#20924,.F.);
#30043=ORIENTED_EDGE('',*,*,#20926,.F.);
#30044=ORIENTED_EDGE('',*,*,#20915,.F.);
#30045=ORIENTED_EDGE('',*,*,#20918,.F.);
#30046=ORIENTED_EDGE('',*,*,#20956,.T.);
#30047=ORIENTED_EDGE('',*,*,#20957,.T.);
#30048=ORIENTED_EDGE('',*,*,#20958,.T.);
#30049=ORIENTED_EDGE('',*,*,#20955,.F.);
#30050=ORIENTED_EDGE('',*,*,#20958,.F.);
#30051=ORIENTED_EDGE('',*,*,#20959,.F.);
#30052=ORIENTED_EDGE('',*,*,#20960,.T.);
#30053=ORIENTED_EDGE('',*,*,#20956,.F.);
#30054=ORIENTED_EDGE('',*,*,#20957,.F.);
#30055=ORIENTED_EDGE('',*,*,#20960,.F.);
#30056=ORIENTED_EDGE('',*,*,#20853,.F.);
#30057=ORIENTED_EDGE('',*,*,#20854,.F.);
#30058=ORIENTED_EDGE('',*,*,#20961,.T.);
#30059=ORIENTED_EDGE('',*,*,#20962,.T.);
#30060=ORIENTED_EDGE('',*,*,#20961,.F.);
#30061=ORIENTED_EDGE('',*,*,#20962,.F.);
#30062=ORIENTED_EDGE('',*,*,#20951,.T.);
#30063=ORIENTED_EDGE('',*,*,#20952,.T.);
#30064=ORIENTED_EDGE('',*,*,#20963,.T.);
#30065=ORIENTED_EDGE('',*,*,#20851,.F.);
#30066=ORIENTED_EDGE('',*,*,#20963,.F.);
#30067=ORIENTED_EDGE('',*,*,#20901,.T.);
#30068=ORIENTED_EDGE('',*,*,#20902,.T.);
#30069=ORIENTED_EDGE('',*,*,#20964,.T.);
#30070=ORIENTED_EDGE('',*,*,#20852,.F.);
#30071=ORIENTED_EDGE('',*,*,#20964,.F.);
#30072=ORIENTED_EDGE('',*,*,#20965,.F.);
#30073=ORIENTED_EDGE('',*,*,#20832,.F.);
#30074=ORIENTED_EDGE('',*,*,#20833,.F.);
#30075=ORIENTED_EDGE('',*,*,#20966,.T.);
#30076=ORIENTED_EDGE('',*,*,#20965,.T.);
#30077=ORIENTED_EDGE('',*,*,#20966,.F.);
#30078=ORIENTED_EDGE('',*,*,#20967,.F.);
#30079=ORIENTED_EDGE('',*,*,#20968,.T.);
#30080=ORIENTED_EDGE('',*,*,#20906,.F.);
#30081=ORIENTED_EDGE('',*,*,#20907,.F.);
#30082=ORIENTED_EDGE('',*,*,#20968,.F.);
#30083=ORIENTED_EDGE('',*,*,#20969,.T.);
#30084=ORIENTED_EDGE('',*,*,#20970,.T.);
#30085=ORIENTED_EDGE('',*,*,#20971,.T.);
#30086=ORIENTED_EDGE('',*,*,#20972,.T.);
#30087=ORIENTED_EDGE('',*,*,#20971,.F.);
#30088=ORIENTED_EDGE('',*,*,#20959,.T.);
#30089=ORIENTED_EDGE('',*,*,#20949,.T.);
#30090=ORIENTED_EDGE('',*,*,#20969,.F.);
#30091=ORIENTED_EDGE('',*,*,#20970,.F.);
#30092=ORIENTED_EDGE('',*,*,#20973,.T.);
#30093=ORIENTED_EDGE('',*,*,#20847,.T.);
#30094=ORIENTED_EDGE('',*,*,#20973,.F.);
#30095=ORIENTED_EDGE('',*,*,#20848,.F.);
#30096=ORIENTED_EDGE('',*,*,#20846,.F.);
#30097=ORIENTED_EDGE('',*,*,#20841,.F.);
#30098=ORIENTED_EDGE('',*,*,#20857,.T.);
#30099=ORIENTED_EDGE('',*,*,#20545,.F.);
#30100=ORIENTED_EDGE('',*,*,#20974,.F.);
#30101=ORIENTED_EDGE('',*,*,#20544,.F.);
#30102=ORIENTED_EDGE('',*,*,#20975,.T.);
#30103=ORIENTED_EDGE('',*,*,#20849,.T.);
#30104=ORIENTED_EDGE('',*,*,#20974,.T.);
#30105=ORIENTED_EDGE('',*,*,#20543,.F.);
#30106=ORIENTED_EDGE('',*,*,#20858,.F.);
#30107=ORIENTED_EDGE('',*,*,#20843,.T.);
#30108=ORIENTED_EDGE('',*,*,#20845,.F.);
#30109=ORIENTED_EDGE('',*,*,#20850,.F.);
#30110=ORIENTED_EDGE('',*,*,#20975,.F.);
#30111=ORIENTED_EDGE('',*,*,#20976,.T.);
#30112=ORIENTED_EDGE('',*,*,#20977,.T.);
#30113=ORIENTED_EDGE('',*,*,#20836,.F.);
#30114=ORIENTED_EDGE('',*,*,#20837,.F.);
#30115=ORIENTED_EDGE('',*,*,#20977,.F.);
#30116=ORIENTED_EDGE('',*,*,#20899,.T.);
#30117=ORIENTED_EDGE('',*,*,#20967,.T.);
#30118=ORIENTED_EDGE('',*,*,#20780,.F.);
#30119=ORIENTED_EDGE('',*,*,#20978,.F.);
#30120=ORIENTED_EDGE('',*,*,#20979,.T.);
#30121=ORIENTED_EDGE('',*,*,#20972,.F.);
#30122=ORIENTED_EDGE('',*,*,#20781,.F.);
#30123=ORIENTED_EDGE('',*,*,#20980,.T.);
#30124=ORIENTED_EDGE('',*,*,#20979,.F.);
#30125=ORIENTED_EDGE('',*,*,#20980,.F.);
#30126=ORIENTED_EDGE('',*,*,#20784,.F.);
#30127=ORIENTED_EDGE('',*,*,#20978,.T.);
#30128=ORIENTED_EDGE('',*,*,#20981,.T.);
#30129=ORIENTED_EDGE('',*,*,#20982,.T.);
#30130=ORIENTED_EDGE('',*,*,#20981,.F.);
#30131=ORIENTED_EDGE('',*,*,#20812,.F.);
#30132=ORIENTED_EDGE('',*,*,#20982,.F.);
#30133=ORIENTED_EDGE('',*,*,#20983,.T.);
#30134=ORIENTED_EDGE('',*,*,#20976,.F.);
#30135=ORIENTED_EDGE('',*,*,#20813,.F.);
#30136=ORIENTED_EDGE('',*,*,#20814,.F.);
#30137=ORIENTED_EDGE('',*,*,#20984,.T.);
#30138=ORIENTED_EDGE('',*,*,#20983,.F.);
#30139=ORIENTED_EDGE('',*,*,#20984,.F.);
#30140=ORIENTED_EDGE('',*,*,#20985,.F.);
#30141=ORIENTED_EDGE('',*,*,#20986,.F.);
#30142=ORIENTED_EDGE('',*,*,#20987,.F.);
#30143=ORIENTED_EDGE('',*,*,#20988,.F.);
#30144=ORIENTED_EDGE('',*,*,#20989,.F.);
#30145=ORIENTED_EDGE('',*,*,#20990,.F.);
#30146=ORIENTED_EDGE('',*,*,#20991,.F.);
#30147=ORIENTED_EDGE('',*,*,#20992,.F.);
#30148=ORIENTED_EDGE('',*,*,#20993,.F.);
#30149=ORIENTED_EDGE('',*,*,#20994,.F.);
#30150=ORIENTED_EDGE('',*,*,#20995,.F.);
#30151=ORIENTED_EDGE('',*,*,#20996,.F.);
#30152=ORIENTED_EDGE('',*,*,#20997,.F.);
#30153=ORIENTED_EDGE('',*,*,#20998,.F.);
#30154=ORIENTED_EDGE('',*,*,#20995,.T.);
#30155=ORIENTED_EDGE('',*,*,#20999,.T.);
#30156=ORIENTED_EDGE('',*,*,#20988,.T.);
#30157=ORIENTED_EDGE('',*,*,#21000,.T.);
#30158=ORIENTED_EDGE('',*,*,#21001,.T.);
#30159=ORIENTED_EDGE('',*,*,#20825,.F.);
#30160=ORIENTED_EDGE('',*,*,#21002,.F.);
#30161=ORIENTED_EDGE('',*,*,#21003,.T.);
#30162=ORIENTED_EDGE('',*,*,#20990,.T.);
#30163=ORIENTED_EDGE('',*,*,#21004,.T.);
#30164=ORIENTED_EDGE('',*,*,#21002,.T.);
#30165=ORIENTED_EDGE('',*,*,#20824,.F.);
#30166=ORIENTED_EDGE('',*,*,#21005,.F.);
#30167=ORIENTED_EDGE('',*,*,#21006,.F.);
#30168=ORIENTED_EDGE('',*,*,#20993,.T.);
#30169=ORIENTED_EDGE('',*,*,#21007,.F.);
#30170=ORIENTED_EDGE('',*,*,#21003,.F.);
#30171=ORIENTED_EDGE('',*,*,#21008,.F.);
#30172=ORIENTED_EDGE('',*,*,#20991,.T.);
#30173=ORIENTED_EDGE('',*,*,#20999,.F.);
#30174=ORIENTED_EDGE('',*,*,#21004,.F.);
#30175=ORIENTED_EDGE('',*,*,#20989,.T.);
#30176=ORIENTED_EDGE('',*,*,#21009,.F.);
#30177=ORIENTED_EDGE('',*,*,#20985,.T.);
#30178=ORIENTED_EDGE('',*,*,#21010,.F.);
#30179=ORIENTED_EDGE('',*,*,#21011,.F.);
#30180=ORIENTED_EDGE('',*,*,#21000,.F.);
#30181=ORIENTED_EDGE('',*,*,#20987,.T.);
#30182=ORIENTED_EDGE('',*,*,#21011,.T.);
#30183=ORIENTED_EDGE('',*,*,#20986,.T.);
#30184=ORIENTED_EDGE('',*,*,#21009,.T.);
#30185=ORIENTED_EDGE('',*,*,#21012,.T.);
#30186=ORIENTED_EDGE('',*,*,#20826,.F.);
#30187=ORIENTED_EDGE('',*,*,#21001,.F.);
#30188=ORIENTED_EDGE('',*,*,#21010,.T.);
#30189=ORIENTED_EDGE('',*,*,#20996,.T.);
#30190=ORIENTED_EDGE('',*,*,#20998,.T.);
#30191=ORIENTED_EDGE('',*,*,#21013,.T.);
#30192=ORIENTED_EDGE('',*,*,#20827,.F.);
#30193=ORIENTED_EDGE('',*,*,#21012,.F.);
#30194=ORIENTED_EDGE('',*,*,#20997,.T.);
#30195=ORIENTED_EDGE('',*,*,#20994,.T.);
#30196=ORIENTED_EDGE('',*,*,#21006,.T.);
#30197=ORIENTED_EDGE('',*,*,#21014,.T.);
#30198=ORIENTED_EDGE('',*,*,#20828,.F.);
#30199=ORIENTED_EDGE('',*,*,#21013,.F.);
#30200=ORIENTED_EDGE('',*,*,#21007,.T.);
#30201=ORIENTED_EDGE('',*,*,#20992,.T.);
#30202=ORIENTED_EDGE('',*,*,#21008,.T.);
#30203=ORIENTED_EDGE('',*,*,#21005,.T.);
#30204=ORIENTED_EDGE('',*,*,#20823,.F.);
#30205=ORIENTED_EDGE('',*,*,#21014,.F.);
#30206=ORIENTED_EDGE('',*,*,#21015,.F.);
#30207=ORIENTED_EDGE('',*,*,#21016,.F.);
#30208=ORIENTED_EDGE('',*,*,#21017,.F.);
#30209=ORIENTED_EDGE('',*,*,#21018,.F.);
#30210=ORIENTED_EDGE('',*,*,#21019,.F.);
#30211=ORIENTED_EDGE('',*,*,#21020,.F.);
#30212=ORIENTED_EDGE('',*,*,#21021,.F.);
#30213=ORIENTED_EDGE('',*,*,#21022,.F.);
#30214=ORIENTED_EDGE('',*,*,#21023,.F.);
#30215=ORIENTED_EDGE('',*,*,#21024,.F.);
#30216=ORIENTED_EDGE('',*,*,#21025,.F.);
#30217=ORIENTED_EDGE('',*,*,#21026,.F.);
#30218=ORIENTED_EDGE('',*,*,#21027,.F.);
#30219=ORIENTED_EDGE('',*,*,#21028,.F.);
#30220=ORIENTED_EDGE('',*,*,#21025,.T.);
#30221=ORIENTED_EDGE('',*,*,#21029,.T.);
#30222=ORIENTED_EDGE('',*,*,#21018,.T.);
#30223=ORIENTED_EDGE('',*,*,#21030,.T.);
#30224=ORIENTED_EDGE('',*,*,#21031,.T.);
#30225=ORIENTED_EDGE('',*,*,#20819,.F.);
#30226=ORIENTED_EDGE('',*,*,#21032,.F.);
#30227=ORIENTED_EDGE('',*,*,#21033,.T.);
#30228=ORIENTED_EDGE('',*,*,#21020,.T.);
#30229=ORIENTED_EDGE('',*,*,#21034,.T.);
#30230=ORIENTED_EDGE('',*,*,#21032,.T.);
#30231=ORIENTED_EDGE('',*,*,#20818,.F.);
#30232=ORIENTED_EDGE('',*,*,#21035,.F.);
#30233=ORIENTED_EDGE('',*,*,#21036,.F.);
#30234=ORIENTED_EDGE('',*,*,#21023,.T.);
#30235=ORIENTED_EDGE('',*,*,#21037,.F.);
#30236=ORIENTED_EDGE('',*,*,#21033,.F.);
#30237=ORIENTED_EDGE('',*,*,#21038,.F.);
#30238=ORIENTED_EDGE('',*,*,#21021,.T.);
#30239=ORIENTED_EDGE('',*,*,#21029,.F.);
#30240=ORIENTED_EDGE('',*,*,#21034,.F.);
#30241=ORIENTED_EDGE('',*,*,#21019,.T.);
#30242=ORIENTED_EDGE('',*,*,#21039,.F.);
#30243=ORIENTED_EDGE('',*,*,#21015,.T.);
#30244=ORIENTED_EDGE('',*,*,#21040,.F.);
#30245=ORIENTED_EDGE('',*,*,#21041,.F.);
#30246=ORIENTED_EDGE('',*,*,#21030,.F.);
#30247=ORIENTED_EDGE('',*,*,#21017,.T.);
#30248=ORIENTED_EDGE('',*,*,#21041,.T.);
#30249=ORIENTED_EDGE('',*,*,#21016,.T.);
#30250=ORIENTED_EDGE('',*,*,#21039,.T.);
#30251=ORIENTED_EDGE('',*,*,#21042,.T.);
#30252=ORIENTED_EDGE('',*,*,#20820,.F.);
#30253=ORIENTED_EDGE('',*,*,#21031,.F.);
#30254=ORIENTED_EDGE('',*,*,#21040,.T.);
#30255=ORIENTED_EDGE('',*,*,#21026,.T.);
#30256=ORIENTED_EDGE('',*,*,#21028,.T.);
#30257=ORIENTED_EDGE('',*,*,#21043,.T.);
#30258=ORIENTED_EDGE('',*,*,#20821,.F.);
#30259=ORIENTED_EDGE('',*,*,#21042,.F.);
#30260=ORIENTED_EDGE('',*,*,#21027,.T.);
#30261=ORIENTED_EDGE('',*,*,#21024,.T.);
#30262=ORIENTED_EDGE('',*,*,#21036,.T.);
#30263=ORIENTED_EDGE('',*,*,#21044,.T.);
#30264=ORIENTED_EDGE('',*,*,#20822,.F.);
#30265=ORIENTED_EDGE('',*,*,#21043,.F.);
#30266=ORIENTED_EDGE('',*,*,#21037,.T.);
#30267=ORIENTED_EDGE('',*,*,#21022,.T.);
#30268=ORIENTED_EDGE('',*,*,#21038,.T.);
#30269=ORIENTED_EDGE('',*,*,#21035,.T.);
#30270=ORIENTED_EDGE('',*,*,#20817,.F.);
#30271=ORIENTED_EDGE('',*,*,#21044,.F.);
#30272=ORIENTED_EDGE('',*,*,#21045,.T.);
#30273=ORIENTED_EDGE('',*,*,#20709,.T.);
#30274=ORIENTED_EDGE('',*,*,#21046,.T.);
#30275=ORIENTED_EDGE('',*,*,#20701,.T.);
#30276=ORIENTED_EDGE('',*,*,#21047,.T.);
#30277=ORIENTED_EDGE('',*,*,#20693,.T.);
#30278=ORIENTED_EDGE('',*,*,#21048,.T.);
#30279=ORIENTED_EDGE('',*,*,#21049,.T.);
#30280=ORIENTED_EDGE('',*,*,#21050,.F.);
#30281=ORIENTED_EDGE('',*,*,#21049,.F.);
#30282=ORIENTED_EDGE('',*,*,#21051,.T.);
#30283=ORIENTED_EDGE('',*,*,#21052,.T.);
#30284=ORIENTED_EDGE('',*,*,#21053,.F.);
#30285=ORIENTED_EDGE('',*,*,#21052,.F.);
#30286=ORIENTED_EDGE('',*,*,#21054,.F.);
#30287=ORIENTED_EDGE('',*,*,#21055,.T.);
#30288=ORIENTED_EDGE('',*,*,#20510,.F.);
#30289=ORIENTED_EDGE('',*,*,#21055,.F.);
#30290=ORIENTED_EDGE('',*,*,#21056,.T.);
#30291=ORIENTED_EDGE('',*,*,#21057,.T.);
#30292=ORIENTED_EDGE('',*,*,#21058,.F.);
#30293=ORIENTED_EDGE('',*,*,#21057,.F.);
#30294=ORIENTED_EDGE('',*,*,#21059,.T.);
#30295=ORIENTED_EDGE('',*,*,#21060,.T.);
#30296=ORIENTED_EDGE('',*,*,#21061,.F.);
#30297=ORIENTED_EDGE('',*,*,#21060,.F.);
#30298=ORIENTED_EDGE('',*,*,#21062,.T.);
#30299=ORIENTED_EDGE('',*,*,#21063,.T.);
#30300=ORIENTED_EDGE('',*,*,#21064,.F.);
#30301=ORIENTED_EDGE('',*,*,#21063,.F.);
#30302=ORIENTED_EDGE('',*,*,#21065,.T.);
#30303=ORIENTED_EDGE('',*,*,#21066,.T.);
#30304=ORIENTED_EDGE('',*,*,#21067,.F.);
#30305=ORIENTED_EDGE('',*,*,#21066,.F.);
#30306=ORIENTED_EDGE('',*,*,#21068,.F.);
#30307=ORIENTED_EDGE('',*,*,#21069,.T.);
#30308=ORIENTED_EDGE('',*,*,#21070,.T.);
#30309=ORIENTED_EDGE('',*,*,#21071,.T.);
#30310=ORIENTED_EDGE('',*,*,#21072,.T.);
#30311=ORIENTED_EDGE('',*,*,#21073,.T.);
#30312=ORIENTED_EDGE('',*,*,#21074,.T.);
#30313=ORIENTED_EDGE('',*,*,#21075,.T.);
#30314=ORIENTED_EDGE('',*,*,#21076,.T.);
#30315=ORIENTED_EDGE('',*,*,#21077,.F.);
#30316=ORIENTED_EDGE('',*,*,#21078,.F.);
#30317=ORIENTED_EDGE('',*,*,#21079,.T.);
#30318=ORIENTED_EDGE('',*,*,#21080,.T.);
#30319=ORIENTED_EDGE('',*,*,#21081,.F.);
#30320=ORIENTED_EDGE('',*,*,#21082,.F.);
#30321=ORIENTED_EDGE('',*,*,#21077,.T.);
#30322=ORIENTED_EDGE('',*,*,#21083,.T.);
#30323=ORIENTED_EDGE('',*,*,#21084,.F.);
#30324=ORIENTED_EDGE('',*,*,#21085,.F.);
#30325=ORIENTED_EDGE('',*,*,#21081,.T.);
#30326=ORIENTED_EDGE('',*,*,#21086,.T.);
#30327=ORIENTED_EDGE('',*,*,#21087,.F.);
#30328=ORIENTED_EDGE('',*,*,#21088,.F.);
#30329=ORIENTED_EDGE('',*,*,#21084,.T.);
#30330=ORIENTED_EDGE('',*,*,#21089,.T.);
#30331=ORIENTED_EDGE('',*,*,#21090,.F.);
#30332=ORIENTED_EDGE('',*,*,#21091,.F.);
#30333=ORIENTED_EDGE('',*,*,#21087,.T.);
#30334=ORIENTED_EDGE('',*,*,#21092,.T.);
#30335=ORIENTED_EDGE('',*,*,#21093,.F.);
#30336=ORIENTED_EDGE('',*,*,#21094,.F.);
#30337=ORIENTED_EDGE('',*,*,#21090,.T.);
#30338=ORIENTED_EDGE('',*,*,#21095,.F.);
#30339=ORIENTED_EDGE('',*,*,#21096,.F.);
#30340=ORIENTED_EDGE('',*,*,#21097,.T.);
#30341=ORIENTED_EDGE('',*,*,#21093,.T.);
#30342=ORIENTED_EDGE('',*,*,#21098,.T.);
#30343=ORIENTED_EDGE('',*,*,#21079,.F.);
#30344=ORIENTED_EDGE('',*,*,#21099,.F.);
#30345=ORIENTED_EDGE('',*,*,#21096,.T.);
#30346=ORIENTED_EDGE('',*,*,#21078,.T.);
#30347=ORIENTED_EDGE('',*,*,#21082,.T.);
#30348=ORIENTED_EDGE('',*,*,#21085,.T.);
#30349=ORIENTED_EDGE('',*,*,#21088,.T.);
#30350=ORIENTED_EDGE('',*,*,#21091,.T.);
#30351=ORIENTED_EDGE('',*,*,#21094,.T.);
#30352=ORIENTED_EDGE('',*,*,#21097,.F.);
#30353=ORIENTED_EDGE('',*,*,#21099,.T.);
#30354=ORIENTED_EDGE('',*,*,#21100,.T.);
#30355=ORIENTED_EDGE('',*,*,#21101,.F.);
#30356=ORIENTED_EDGE('',*,*,#21102,.F.);
#30357=ORIENTED_EDGE('',*,*,#21103,.T.);
#30358=ORIENTED_EDGE('',*,*,#21104,.T.);
#30359=ORIENTED_EDGE('',*,*,#21105,.F.);
#30360=ORIENTED_EDGE('',*,*,#21106,.F.);
#30361=ORIENTED_EDGE('',*,*,#21101,.T.);
#30362=ORIENTED_EDGE('',*,*,#21107,.T.);
#30363=ORIENTED_EDGE('',*,*,#21108,.F.);
#30364=ORIENTED_EDGE('',*,*,#21109,.F.);
#30365=ORIENTED_EDGE('',*,*,#21105,.T.);
#30366=ORIENTED_EDGE('',*,*,#21110,.T.);
#30367=ORIENTED_EDGE('',*,*,#21111,.F.);
#30368=ORIENTED_EDGE('',*,*,#21112,.F.);
#30369=ORIENTED_EDGE('',*,*,#21108,.T.);
#30370=ORIENTED_EDGE('',*,*,#21113,.T.);
#30371=ORIENTED_EDGE('',*,*,#21114,.F.);
#30372=ORIENTED_EDGE('',*,*,#21115,.F.);
#30373=ORIENTED_EDGE('',*,*,#21111,.T.);
#30374=ORIENTED_EDGE('',*,*,#21116,.T.);
#30375=ORIENTED_EDGE('',*,*,#21117,.F.);
#30376=ORIENTED_EDGE('',*,*,#21118,.F.);
#30377=ORIENTED_EDGE('',*,*,#21114,.T.);
#30378=ORIENTED_EDGE('',*,*,#21119,.F.);
#30379=ORIENTED_EDGE('',*,*,#21120,.F.);
#30380=ORIENTED_EDGE('',*,*,#21121,.T.);
#30381=ORIENTED_EDGE('',*,*,#21117,.T.);
#30382=ORIENTED_EDGE('',*,*,#21122,.T.);
#30383=ORIENTED_EDGE('',*,*,#21103,.F.);
#30384=ORIENTED_EDGE('',*,*,#21123,.F.);
#30385=ORIENTED_EDGE('',*,*,#21120,.T.);
#30386=ORIENTED_EDGE('',*,*,#21102,.T.);
#30387=ORIENTED_EDGE('',*,*,#21106,.T.);
#30388=ORIENTED_EDGE('',*,*,#21109,.T.);
#30389=ORIENTED_EDGE('',*,*,#21112,.T.);
#30390=ORIENTED_EDGE('',*,*,#21115,.T.);
#30391=ORIENTED_EDGE('',*,*,#21118,.T.);
#30392=ORIENTED_EDGE('',*,*,#21121,.F.);
#30393=ORIENTED_EDGE('',*,*,#21123,.T.);
#30394=ORIENTED_EDGE('',*,*,#21124,.T.);
#30395=ORIENTED_EDGE('',*,*,#21125,.F.);
#30396=ORIENTED_EDGE('',*,*,#21126,.F.);
#30397=ORIENTED_EDGE('',*,*,#21127,.T.);
#30398=ORIENTED_EDGE('',*,*,#21128,.T.);
#30399=ORIENTED_EDGE('',*,*,#21129,.F.);
#30400=ORIENTED_EDGE('',*,*,#21130,.F.);
#30401=ORIENTED_EDGE('',*,*,#21125,.T.);
#30402=ORIENTED_EDGE('',*,*,#21131,.T.);
#30403=ORIENTED_EDGE('',*,*,#21132,.F.);
#30404=ORIENTED_EDGE('',*,*,#21133,.F.);
#30405=ORIENTED_EDGE('',*,*,#21129,.T.);
#30406=ORIENTED_EDGE('',*,*,#21134,.T.);
#30407=ORIENTED_EDGE('',*,*,#21135,.F.);
#30408=ORIENTED_EDGE('',*,*,#21136,.F.);
#30409=ORIENTED_EDGE('',*,*,#21132,.T.);
#30410=ORIENTED_EDGE('',*,*,#21137,.T.);
#30411=ORIENTED_EDGE('',*,*,#21138,.F.);
#30412=ORIENTED_EDGE('',*,*,#21139,.F.);
#30413=ORIENTED_EDGE('',*,*,#21135,.T.);
#30414=ORIENTED_EDGE('',*,*,#21140,.T.);
#30415=ORIENTED_EDGE('',*,*,#21141,.F.);
#30416=ORIENTED_EDGE('',*,*,#21142,.F.);
#30417=ORIENTED_EDGE('',*,*,#21138,.T.);
#30418=ORIENTED_EDGE('',*,*,#21143,.F.);
#30419=ORIENTED_EDGE('',*,*,#21144,.F.);
#30420=ORIENTED_EDGE('',*,*,#21145,.T.);
#30421=ORIENTED_EDGE('',*,*,#21141,.T.);
#30422=ORIENTED_EDGE('',*,*,#21146,.T.);
#30423=ORIENTED_EDGE('',*,*,#21127,.F.);
#30424=ORIENTED_EDGE('',*,*,#21147,.F.);
#30425=ORIENTED_EDGE('',*,*,#21144,.T.);
#30426=ORIENTED_EDGE('',*,*,#21126,.T.);
#30427=ORIENTED_EDGE('',*,*,#21130,.T.);
#30428=ORIENTED_EDGE('',*,*,#21133,.T.);
#30429=ORIENTED_EDGE('',*,*,#21136,.T.);
#30430=ORIENTED_EDGE('',*,*,#21139,.T.);
#30431=ORIENTED_EDGE('',*,*,#21142,.T.);
#30432=ORIENTED_EDGE('',*,*,#21145,.F.);
#30433=ORIENTED_EDGE('',*,*,#21147,.T.);
#30434=ORIENTED_EDGE('',*,*,#21047,.F.);
#30435=ORIENTED_EDGE('',*,*,#21148,.T.);
#30436=ORIENTED_EDGE('',*,*,#21149,.F.);
#30437=ORIENTED_EDGE('',*,*,#21148,.F.);
#30438=ORIENTED_EDGE('',*,*,#21046,.F.);
#30439=ORIENTED_EDGE('',*,*,#21150,.T.);
#30440=ORIENTED_EDGE('',*,*,#21151,.F.);
#30441=ORIENTED_EDGE('',*,*,#21150,.F.);
#30442=ORIENTED_EDGE('',*,*,#21045,.F.);
#30443=ORIENTED_EDGE('',*,*,#21152,.T.);
#30444=ORIENTED_EDGE('',*,*,#21153,.F.);
#30445=ORIENTED_EDGE('',*,*,#21152,.F.);
#30446=ORIENTED_EDGE('',*,*,#21154,.T.);
#30447=ORIENTED_EDGE('',*,*,#21155,.F.);
#30448=ORIENTED_EDGE('',*,*,#21156,.F.);
#30449=ORIENTED_EDGE('',*,*,#21157,.F.);
#30450=ORIENTED_EDGE('',*,*,#21158,.T.);
#30451=ORIENTED_EDGE('',*,*,#21156,.T.);
#30452=ORIENTED_EDGE('',*,*,#21159,.T.);
#30453=ORIENTED_EDGE('',*,*,#21160,.F.);
#30454=ORIENTED_EDGE('',*,*,#21161,.F.);
#30455=ORIENTED_EDGE('',*,*,#21162,.F.);
#30456=ORIENTED_EDGE('',*,*,#21163,.T.);
#30457=ORIENTED_EDGE('',*,*,#21161,.T.);
#30458=ORIENTED_EDGE('',*,*,#21164,.F.);
#30459=ORIENTED_EDGE('',*,*,#21165,.T.);
#30460=ORIENTED_EDGE('',*,*,#21166,.F.);
#30461=ORIENTED_EDGE('',*,*,#21167,.F.);
#30462=ORIENTED_EDGE('',*,*,#21168,.T.);
#30463=ORIENTED_EDGE('',*,*,#21167,.T.);
#30464=ORIENTED_EDGE('',*,*,#21169,.F.);
#30465=ORIENTED_EDGE('',*,*,#21170,.F.);
#30466=ORIENTED_EDGE('',*,*,#21171,.T.);
#30467=ORIENTED_EDGE('',*,*,#21172,.F.);
#30468=ORIENTED_EDGE('',*,*,#21173,.F.);
#30469=ORIENTED_EDGE('',*,*,#21174,.F.);
#30470=ORIENTED_EDGE('',*,*,#21153,.T.);
#30471=ORIENTED_EDGE('',*,*,#21175,.F.);
#30472=ORIENTED_EDGE('',*,*,#21176,.F.);
#30473=ORIENTED_EDGE('',*,*,#21177,.F.);
#30474=ORIENTED_EDGE('',*,*,#21178,.F.);
#30475=ORIENTED_EDGE('',*,*,#21179,.T.);
#30476=ORIENTED_EDGE('',*,*,#21180,.F.);
#30477=ORIENTED_EDGE('',*,*,#21149,.T.);
#30478=ORIENTED_EDGE('',*,*,#21181,.F.);
#30479=ORIENTED_EDGE('',*,*,#21182,.F.);
#30480=ORIENTED_EDGE('',*,*,#21183,.F.);
#30481=ORIENTED_EDGE('',*,*,#21184,.F.);
#30482=ORIENTED_EDGE('',*,*,#21185,.T.);
#30483=ORIENTED_EDGE('',*,*,#21186,.F.);
#30484=ORIENTED_EDGE('',*,*,#21187,.T.);
#30485=ORIENTED_EDGE('',*,*,#21188,.F.);
#30486=ORIENTED_EDGE('',*,*,#21189,.T.);
#30487=ORIENTED_EDGE('',*,*,#21190,.T.);
#30488=ORIENTED_EDGE('',*,*,#21191,.T.);
#30489=ORIENTED_EDGE('',*,*,#21189,.F.);
#30490=ORIENTED_EDGE('',*,*,#21192,.T.);
#30491=ORIENTED_EDGE('',*,*,#20776,.F.);
#30492=ORIENTED_EDGE('',*,*,#21193,.T.);
#30493=ORIENTED_EDGE('',*,*,#21194,.T.);
#30494=ORIENTED_EDGE('',*,*,#21195,.T.);
#30495=ORIENTED_EDGE('',*,*,#21196,.T.);
#30496=ORIENTED_EDGE('',*,*,#21197,.T.);
#30497=ORIENTED_EDGE('',*,*,#20770,.F.);
#30498=ORIENTED_EDGE('',*,*,#21198,.T.);
#30499=ORIENTED_EDGE('',*,*,#20774,.F.);
#30500=ORIENTED_EDGE('',*,*,#21199,.T.);
#30501=ORIENTED_EDGE('',*,*,#21200,.T.);
#30502=ORIENTED_EDGE('',*,*,#21201,.T.);
#30503=ORIENTED_EDGE('',*,*,#20772,.F.);
#30504=ORIENTED_EDGE('',*,*,#21202,.T.);
#30505=ORIENTED_EDGE('',*,*,#21203,.T.);
#30506=ORIENTED_EDGE('',*,*,#21204,.T.);
#30507=ORIENTED_EDGE('',*,*,#21164,.T.);
#30508=ORIENTED_EDGE('',*,*,#21168,.F.);
#30509=ORIENTED_EDGE('',*,*,#21166,.T.);
#30510=ORIENTED_EDGE('',*,*,#21205,.T.);
#30511=ORIENTED_EDGE('',*,*,#21206,.F.);
#30512=ORIENTED_EDGE('',*,*,#21173,.T.);
#30513=ORIENTED_EDGE('',*,*,#21207,.T.);
#30514=ORIENTED_EDGE('',*,*,#21208,.F.);
#30515=ORIENTED_EDGE('',*,*,#21209,.T.);
#30516=ORIENTED_EDGE('',*,*,#21177,.T.);
#30517=ORIENTED_EDGE('',*,*,#21210,.T.);
#30518=ORIENTED_EDGE('',*,*,#21210,.F.);
#30519=ORIENTED_EDGE('',*,*,#21176,.T.);
#30520=ORIENTED_EDGE('',*,*,#21211,.T.);
#30521=ORIENTED_EDGE('',*,*,#21212,.T.);
#30522=ORIENTED_EDGE('',*,*,#21213,.T.);
#30523=ORIENTED_EDGE('',*,*,#21162,.T.);
#30524=ORIENTED_EDGE('',*,*,#21163,.F.);
#30525=ORIENTED_EDGE('',*,*,#21160,.T.);
#30526=ORIENTED_EDGE('',*,*,#21214,.T.);
#30527=ORIENTED_EDGE('',*,*,#21211,.F.);
#30528=ORIENTED_EDGE('',*,*,#21175,.T.);
#30529=ORIENTED_EDGE('',*,*,#21215,.T.);
#30530=ORIENTED_EDGE('',*,*,#21216,.F.);
#30531=ORIENTED_EDGE('',*,*,#21217,.T.);
#30532=ORIENTED_EDGE('',*,*,#21183,.T.);
#30533=ORIENTED_EDGE('',*,*,#21218,.T.);
#30534=ORIENTED_EDGE('',*,*,#21218,.F.);
#30535=ORIENTED_EDGE('',*,*,#21182,.T.);
#30536=ORIENTED_EDGE('',*,*,#21219,.T.);
#30537=ORIENTED_EDGE('',*,*,#21220,.T.);
#30538=ORIENTED_EDGE('',*,*,#21221,.T.);
#30539=ORIENTED_EDGE('',*,*,#21157,.T.);
#30540=ORIENTED_EDGE('',*,*,#21158,.F.);
#30541=ORIENTED_EDGE('',*,*,#21155,.T.);
#30542=ORIENTED_EDGE('',*,*,#21222,.T.);
#30543=ORIENTED_EDGE('',*,*,#21219,.F.);
#30544=ORIENTED_EDGE('',*,*,#21181,.T.);
#30545=ORIENTED_EDGE('',*,*,#21223,.T.);
#30546=ORIENTED_EDGE('',*,*,#21224,.F.);
#30547=ORIENTED_EDGE('',*,*,#21225,.T.);
#30548=ORIENTED_EDGE('',*,*,#21226,.T.);
#30549=ORIENTED_EDGE('',*,*,#21227,.T.);
#30550=ORIENTED_EDGE('',*,*,#21227,.F.);
#30551=ORIENTED_EDGE('',*,*,#21228,.T.);
#30552=ORIENTED_EDGE('',*,*,#21229,.T.);
#30553=ORIENTED_EDGE('',*,*,#21230,.T.);
#30554=ORIENTED_EDGE('',*,*,#21231,.T.);
#30555=ORIENTED_EDGE('',*,*,#21232,.T.);
#30556=ORIENTED_EDGE('',*,*,#21233,.F.);
#30557=ORIENTED_EDGE('',*,*,#21234,.T.);
#30558=ORIENTED_EDGE('',*,*,#21235,.T.);
#30559=ORIENTED_EDGE('',*,*,#21229,.F.);
#30560=ORIENTED_EDGE('',*,*,#21236,.T.);
#30561=ORIENTED_EDGE('',*,*,#21237,.T.);
#30562=ORIENTED_EDGE('',*,*,#21238,.F.);
#30563=ORIENTED_EDGE('',*,*,#21239,.T.);
#30564=ORIENTED_EDGE('',*,*,#21169,.T.);
#30565=ORIENTED_EDGE('',*,*,#21240,.T.);
#30566=ORIENTED_EDGE('',*,*,#21240,.F.);
#30567=ORIENTED_EDGE('',*,*,#21174,.T.);
#30568=ORIENTED_EDGE('',*,*,#21206,.T.);
#30569=ORIENTED_EDGE('',*,*,#21241,.T.);
#30570=ORIENTED_EDGE('',*,*,#21242,.T.);
#30571=ORIENTED_EDGE('',*,*,#21238,.T.);
#30572=ORIENTED_EDGE('',*,*,#21243,.F.);
#30573=ORIENTED_EDGE('',*,*,#21244,.F.);
#30574=ORIENTED_EDGE('',*,*,#21245,.T.);
#30575=ORIENTED_EDGE('',*,*,#21224,.T.);
#30576=ORIENTED_EDGE('',*,*,#21246,.F.);
#30577=ORIENTED_EDGE('',*,*,#21247,.F.);
#30578=ORIENTED_EDGE('',*,*,#21248,.T.);
#30579=ORIENTED_EDGE('',*,*,#21216,.T.);
#30580=ORIENTED_EDGE('',*,*,#21249,.F.);
#30581=ORIENTED_EDGE('',*,*,#21250,.F.);
#30582=ORIENTED_EDGE('',*,*,#21251,.T.);
#30583=ORIENTED_EDGE('',*,*,#21208,.T.);
#30584=ORIENTED_EDGE('',*,*,#21252,.F.);
#30585=ORIENTED_EDGE('',*,*,#21253,.F.);
#30586=ORIENTED_EDGE('',*,*,#21054,.T.);
#30587=ORIENTED_EDGE('',*,*,#21237,.F.);
#30588=ORIENTED_EDGE('',*,*,#21254,.T.);
#30589=ORIENTED_EDGE('',*,*,#21255,.T.);
#30590=ORIENTED_EDGE('',*,*,#21243,.T.);
#30591=ORIENTED_EDGE('',*,*,#21244,.T.);
#30592=ORIENTED_EDGE('',*,*,#21255,.F.);
#30593=ORIENTED_EDGE('',*,*,#21256,.F.);
#30594=ORIENTED_EDGE('',*,*,#21257,.T.);
#30595=ORIENTED_EDGE('',*,*,#21225,.F.);
#30596=ORIENTED_EDGE('',*,*,#21245,.F.);
#30597=ORIENTED_EDGE('',*,*,#21257,.F.);
#30598=ORIENTED_EDGE('',*,*,#21258,.T.);
#30599=ORIENTED_EDGE('',*,*,#21223,.F.);
#30600=ORIENTED_EDGE('',*,*,#21186,.T.);
#30601=ORIENTED_EDGE('',*,*,#21259,.T.);
#30602=ORIENTED_EDGE('',*,*,#21246,.T.);
#30603=ORIENTED_EDGE('',*,*,#21247,.T.);
#30604=ORIENTED_EDGE('',*,*,#21259,.F.);
#30605=ORIENTED_EDGE('',*,*,#21185,.F.);
#30606=ORIENTED_EDGE('',*,*,#21260,.T.);
#30607=ORIENTED_EDGE('',*,*,#21217,.F.);
#30608=ORIENTED_EDGE('',*,*,#21248,.F.);
#30609=ORIENTED_EDGE('',*,*,#21260,.F.);
#30610=ORIENTED_EDGE('',*,*,#21184,.T.);
#30611=ORIENTED_EDGE('',*,*,#21215,.F.);
#30612=ORIENTED_EDGE('',*,*,#21180,.T.);
#30613=ORIENTED_EDGE('',*,*,#21261,.T.);
#30614=ORIENTED_EDGE('',*,*,#21249,.T.);
#30615=ORIENTED_EDGE('',*,*,#21250,.T.);
#30616=ORIENTED_EDGE('',*,*,#21261,.F.);
#30617=ORIENTED_EDGE('',*,*,#21179,.F.);
#30618=ORIENTED_EDGE('',*,*,#21262,.T.);
#30619=ORIENTED_EDGE('',*,*,#21209,.F.);
#30620=ORIENTED_EDGE('',*,*,#21251,.F.);
#30621=ORIENTED_EDGE('',*,*,#21262,.F.);
#30622=ORIENTED_EDGE('',*,*,#21178,.T.);
#30623=ORIENTED_EDGE('',*,*,#21207,.F.);
#30624=ORIENTED_EDGE('',*,*,#21172,.T.);
#30625=ORIENTED_EDGE('',*,*,#21263,.T.);
#30626=ORIENTED_EDGE('',*,*,#21252,.T.);
#30627=ORIENTED_EDGE('',*,*,#21253,.T.);
#30628=ORIENTED_EDGE('',*,*,#21263,.F.);
#30629=ORIENTED_EDGE('',*,*,#21171,.F.);
#30630=ORIENTED_EDGE('',*,*,#21264,.T.);
#30631=ORIENTED_EDGE('',*,*,#21239,.F.);
#30632=ORIENTED_EDGE('',*,*,#21242,.F.);
#30633=ORIENTED_EDGE('',*,*,#21264,.F.);
#30634=ORIENTED_EDGE('',*,*,#21170,.T.);
#30635=ORIENTED_EDGE('',*,*,#21236,.F.);
#30636=ORIENTED_EDGE('',*,*,#21228,.F.);
#30637=ORIENTED_EDGE('',*,*,#21226,.F.);
#30638=ORIENTED_EDGE('',*,*,#21258,.F.);
#30639=ORIENTED_EDGE('',*,*,#21256,.T.);
#30640=ORIENTED_EDGE('',*,*,#21254,.F.);
#30641=ORIENTED_EDGE('',*,*,#21151,.T.);
#30642=ORIENTED_EDGE('',*,*,#21265,.T.);
#30643=ORIENTED_EDGE('',*,*,#21234,.F.);
#30644=ORIENTED_EDGE('',*,*,#21266,.F.);
#30645=ORIENTED_EDGE('',*,*,#21232,.F.);
#30646=ORIENTED_EDGE('',*,*,#21233,.T.);
#30647=ORIENTED_EDGE('',*,*,#21266,.T.);
#30648=ORIENTED_EDGE('',*,*,#21267,.T.);
#30649=ORIENTED_EDGE('',*,*,#21268,.F.);
#30650=ORIENTED_EDGE('',*,*,#21269,.F.);
#30651=ORIENTED_EDGE('',*,*,#21270,.T.);
#30652=ORIENTED_EDGE('',*,*,#21271,.T.);
#30653=ORIENTED_EDGE('',*,*,#21272,.F.);
#30654=ORIENTED_EDGE('',*,*,#21273,.F.);
#30655=ORIENTED_EDGE('',*,*,#21268,.T.);
#30656=ORIENTED_EDGE('',*,*,#21274,.T.);
#30657=ORIENTED_EDGE('',*,*,#21275,.F.);
#30658=ORIENTED_EDGE('',*,*,#21276,.F.);
#30659=ORIENTED_EDGE('',*,*,#21272,.T.);
#30660=ORIENTED_EDGE('',*,*,#21277,.F.);
#30661=ORIENTED_EDGE('',*,*,#21278,.F.);
#30662=ORIENTED_EDGE('',*,*,#21279,.T.);
#30663=ORIENTED_EDGE('',*,*,#21275,.T.);
#30664=ORIENTED_EDGE('',*,*,#21280,.T.);
#30665=ORIENTED_EDGE('',*,*,#21281,.F.);
#30666=ORIENTED_EDGE('',*,*,#21282,.F.);
#30667=ORIENTED_EDGE('',*,*,#21278,.T.);
#30668=ORIENTED_EDGE('',*,*,#21283,.T.);
#30669=ORIENTED_EDGE('',*,*,#21284,.F.);
#30670=ORIENTED_EDGE('',*,*,#21285,.F.);
#30671=ORIENTED_EDGE('',*,*,#21281,.T.);
#30672=ORIENTED_EDGE('',*,*,#21286,.T.);
#30673=ORIENTED_EDGE('',*,*,#21287,.F.);
#30674=ORIENTED_EDGE('',*,*,#21288,.F.);
#30675=ORIENTED_EDGE('',*,*,#21284,.T.);
#30676=ORIENTED_EDGE('',*,*,#21289,.T.);
#30677=ORIENTED_EDGE('',*,*,#21270,.F.);
#30678=ORIENTED_EDGE('',*,*,#21290,.F.);
#30679=ORIENTED_EDGE('',*,*,#21287,.T.);
#30680=ORIENTED_EDGE('',*,*,#21269,.T.);
#30681=ORIENTED_EDGE('',*,*,#21273,.T.);
#30682=ORIENTED_EDGE('',*,*,#21276,.T.);
#30683=ORIENTED_EDGE('',*,*,#21279,.F.);
#30684=ORIENTED_EDGE('',*,*,#21282,.T.);
#30685=ORIENTED_EDGE('',*,*,#21285,.T.);
#30686=ORIENTED_EDGE('',*,*,#21288,.T.);
#30687=ORIENTED_EDGE('',*,*,#21290,.T.);
#30688=ORIENTED_EDGE('',*,*,#21291,.T.);
#30689=ORIENTED_EDGE('',*,*,#21292,.F.);
#30690=ORIENTED_EDGE('',*,*,#21293,.F.);
#30691=ORIENTED_EDGE('',*,*,#21294,.T.);
#30692=ORIENTED_EDGE('',*,*,#21295,.T.);
#30693=ORIENTED_EDGE('',*,*,#21296,.F.);
#30694=ORIENTED_EDGE('',*,*,#21297,.F.);
#30695=ORIENTED_EDGE('',*,*,#21292,.T.);
#30696=ORIENTED_EDGE('',*,*,#21298,.F.);
#30697=ORIENTED_EDGE('',*,*,#21299,.F.);
#30698=ORIENTED_EDGE('',*,*,#21300,.T.);
#30699=ORIENTED_EDGE('',*,*,#21296,.T.);
#30700=ORIENTED_EDGE('',*,*,#21301,.T.);
#30701=ORIENTED_EDGE('',*,*,#21302,.F.);
#30702=ORIENTED_EDGE('',*,*,#21303,.F.);
#30703=ORIENTED_EDGE('',*,*,#21299,.T.);
#30704=ORIENTED_EDGE('',*,*,#21304,.T.);
#30705=ORIENTED_EDGE('',*,*,#21305,.F.);
#30706=ORIENTED_EDGE('',*,*,#21306,.F.);
#30707=ORIENTED_EDGE('',*,*,#21302,.T.);
#30708=ORIENTED_EDGE('',*,*,#21307,.T.);
#30709=ORIENTED_EDGE('',*,*,#21308,.F.);
#30710=ORIENTED_EDGE('',*,*,#21309,.F.);
#30711=ORIENTED_EDGE('',*,*,#21305,.T.);
#30712=ORIENTED_EDGE('',*,*,#21310,.T.);
#30713=ORIENTED_EDGE('',*,*,#21311,.F.);
#30714=ORIENTED_EDGE('',*,*,#21312,.F.);
#30715=ORIENTED_EDGE('',*,*,#21308,.T.);
#30716=ORIENTED_EDGE('',*,*,#21313,.T.);
#30717=ORIENTED_EDGE('',*,*,#21294,.F.);
#30718=ORIENTED_EDGE('',*,*,#21314,.F.);
#30719=ORIENTED_EDGE('',*,*,#21311,.T.);
#30720=ORIENTED_EDGE('',*,*,#21293,.T.);
#30721=ORIENTED_EDGE('',*,*,#21297,.T.);
#30722=ORIENTED_EDGE('',*,*,#21300,.F.);
#30723=ORIENTED_EDGE('',*,*,#21303,.T.);
#30724=ORIENTED_EDGE('',*,*,#21306,.T.);
#30725=ORIENTED_EDGE('',*,*,#21309,.T.);
#30726=ORIENTED_EDGE('',*,*,#21312,.T.);
#30727=ORIENTED_EDGE('',*,*,#21314,.T.);
#30728=ORIENTED_EDGE('',*,*,#21315,.T.);
#30729=ORIENTED_EDGE('',*,*,#21316,.F.);
#30730=ORIENTED_EDGE('',*,*,#21317,.F.);
#30731=ORIENTED_EDGE('',*,*,#21318,.T.);
#30732=ORIENTED_EDGE('',*,*,#21319,.T.);
#30733=ORIENTED_EDGE('',*,*,#21320,.F.);
#30734=ORIENTED_EDGE('',*,*,#21321,.F.);
#30735=ORIENTED_EDGE('',*,*,#21316,.T.);
#30736=ORIENTED_EDGE('',*,*,#21322,.T.);
#30737=ORIENTED_EDGE('',*,*,#21323,.F.);
#30738=ORIENTED_EDGE('',*,*,#21324,.F.);
#30739=ORIENTED_EDGE('',*,*,#21320,.T.);
#30740=ORIENTED_EDGE('',*,*,#21325,.T.);
#30741=ORIENTED_EDGE('',*,*,#21326,.F.);
#30742=ORIENTED_EDGE('',*,*,#21327,.F.);
#30743=ORIENTED_EDGE('',*,*,#21323,.T.);
#30744=ORIENTED_EDGE('',*,*,#21328,.F.);
#30745=ORIENTED_EDGE('',*,*,#21329,.F.);
#30746=ORIENTED_EDGE('',*,*,#21330,.T.);
#30747=ORIENTED_EDGE('',*,*,#21326,.T.);
#30748=ORIENTED_EDGE('',*,*,#21331,.T.);
#30749=ORIENTED_EDGE('',*,*,#21332,.F.);
#30750=ORIENTED_EDGE('',*,*,#21333,.F.);
#30751=ORIENTED_EDGE('',*,*,#21329,.T.);
#30752=ORIENTED_EDGE('',*,*,#21334,.T.);
#30753=ORIENTED_EDGE('',*,*,#21335,.F.);
#30754=ORIENTED_EDGE('',*,*,#21336,.F.);
#30755=ORIENTED_EDGE('',*,*,#21332,.T.);
#30756=ORIENTED_EDGE('',*,*,#21337,.T.);
#30757=ORIENTED_EDGE('',*,*,#21318,.F.);
#30758=ORIENTED_EDGE('',*,*,#21338,.F.);
#30759=ORIENTED_EDGE('',*,*,#21335,.T.);
#30760=ORIENTED_EDGE('',*,*,#21317,.T.);
#30761=ORIENTED_EDGE('',*,*,#21321,.T.);
#30762=ORIENTED_EDGE('',*,*,#21324,.T.);
#30763=ORIENTED_EDGE('',*,*,#21327,.T.);
#30764=ORIENTED_EDGE('',*,*,#21330,.F.);
#30765=ORIENTED_EDGE('',*,*,#21333,.T.);
#30766=ORIENTED_EDGE('',*,*,#21336,.T.);
#30767=ORIENTED_EDGE('',*,*,#21338,.T.);
#30768=ORIENTED_EDGE('',*,*,#21339,.T.);
#30769=ORIENTED_EDGE('',*,*,#21340,.F.);
#30770=ORIENTED_EDGE('',*,*,#21341,.F.);
#30771=ORIENTED_EDGE('',*,*,#21342,.T.);
#30772=ORIENTED_EDGE('',*,*,#21343,.T.);
#30773=ORIENTED_EDGE('',*,*,#21344,.F.);
#30774=ORIENTED_EDGE('',*,*,#21345,.F.);
#30775=ORIENTED_EDGE('',*,*,#21340,.T.);
#30776=ORIENTED_EDGE('',*,*,#21346,.T.);
#30777=ORIENTED_EDGE('',*,*,#21347,.F.);
#30778=ORIENTED_EDGE('',*,*,#21348,.F.);
#30779=ORIENTED_EDGE('',*,*,#21344,.T.);
#30780=ORIENTED_EDGE('',*,*,#21349,.T.);
#30781=ORIENTED_EDGE('',*,*,#21350,.F.);
#30782=ORIENTED_EDGE('',*,*,#21351,.F.);
#30783=ORIENTED_EDGE('',*,*,#21347,.T.);
#30784=ORIENTED_EDGE('',*,*,#21352,.F.);
#30785=ORIENTED_EDGE('',*,*,#21353,.F.);
#30786=ORIENTED_EDGE('',*,*,#21354,.T.);
#30787=ORIENTED_EDGE('',*,*,#21350,.T.);
#30788=ORIENTED_EDGE('',*,*,#21355,.T.);
#30789=ORIENTED_EDGE('',*,*,#21356,.F.);
#30790=ORIENTED_EDGE('',*,*,#21357,.F.);
#30791=ORIENTED_EDGE('',*,*,#21353,.T.);
#30792=ORIENTED_EDGE('',*,*,#21358,.T.);
#30793=ORIENTED_EDGE('',*,*,#21359,.F.);
#30794=ORIENTED_EDGE('',*,*,#21360,.F.);
#30795=ORIENTED_EDGE('',*,*,#21356,.T.);
#30796=ORIENTED_EDGE('',*,*,#21361,.T.);
#30797=ORIENTED_EDGE('',*,*,#21342,.F.);
#30798=ORIENTED_EDGE('',*,*,#21362,.F.);
#30799=ORIENTED_EDGE('',*,*,#21359,.T.);
#30800=ORIENTED_EDGE('',*,*,#21341,.T.);
#30801=ORIENTED_EDGE('',*,*,#21345,.T.);
#30802=ORIENTED_EDGE('',*,*,#21348,.T.);
#30803=ORIENTED_EDGE('',*,*,#21351,.T.);
#30804=ORIENTED_EDGE('',*,*,#21354,.F.);
#30805=ORIENTED_EDGE('',*,*,#21357,.T.);
#30806=ORIENTED_EDGE('',*,*,#21360,.T.);
#30807=ORIENTED_EDGE('',*,*,#21362,.T.);
#30808=ORIENTED_EDGE('',*,*,#21363,.F.);
#30809=ORIENTED_EDGE('',*,*,#21364,.F.);
#30810=ORIENTED_EDGE('',*,*,#21068,.T.);
#30811=ORIENTED_EDGE('',*,*,#21365,.T.);
#30812=ORIENTED_EDGE('',*,*,#21366,.T.);
#30813=ORIENTED_EDGE('',*,*,#21365,.F.);
#30814=ORIENTED_EDGE('',*,*,#21075,.F.);
#30815=ORIENTED_EDGE('',*,*,#21367,.T.);
#30816=ORIENTED_EDGE('',*,*,#21368,.T.);
#30817=ORIENTED_EDGE('',*,*,#21367,.F.);
#30818=ORIENTED_EDGE('',*,*,#21074,.F.);
#30819=ORIENTED_EDGE('',*,*,#21369,.T.);
#30820=ORIENTED_EDGE('',*,*,#21370,.T.);
#30821=ORIENTED_EDGE('',*,*,#21369,.F.);
#30822=ORIENTED_EDGE('',*,*,#21073,.F.);
#30823=ORIENTED_EDGE('',*,*,#21371,.T.);
#30824=ORIENTED_EDGE('',*,*,#21372,.T.);
#30825=ORIENTED_EDGE('',*,*,#21371,.F.);
#30826=ORIENTED_EDGE('',*,*,#21072,.F.);
#30827=ORIENTED_EDGE('',*,*,#21373,.T.);
#30828=ORIENTED_EDGE('',*,*,#21374,.T.);
#30829=ORIENTED_EDGE('',*,*,#21373,.F.);
#30830=ORIENTED_EDGE('',*,*,#21071,.F.);
#30831=ORIENTED_EDGE('',*,*,#21375,.T.);
#30832=ORIENTED_EDGE('',*,*,#21376,.T.);
#30833=ORIENTED_EDGE('',*,*,#21377,.F.);
#30834=ORIENTED_EDGE('',*,*,#21069,.F.);
#30835=ORIENTED_EDGE('',*,*,#21364,.T.);
#30836=ORIENTED_EDGE('',*,*,#21378,.T.);
#30837=ORIENTED_EDGE('',*,*,#21375,.F.);
#30838=ORIENTED_EDGE('',*,*,#21070,.F.);
#30839=ORIENTED_EDGE('',*,*,#21377,.T.);
#30840=ORIENTED_EDGE('',*,*,#21191,.F.);
#30841=ORIENTED_EDGE('',*,*,#21379,.T.);
#30842=ORIENTED_EDGE('',*,*,#21380,.T.);
#30843=ORIENTED_EDGE('',*,*,#21379,.F.);
#30844=ORIENTED_EDGE('',*,*,#21190,.F.);
#30845=ORIENTED_EDGE('',*,*,#21380,.F.);
#30846=ORIENTED_EDGE('',*,*,#21050,.T.);
#30847=ORIENTED_EDGE('',*,*,#21053,.T.);
#30848=ORIENTED_EDGE('',*,*,#21058,.T.);
#30849=ORIENTED_EDGE('',*,*,#21061,.T.);
#30850=ORIENTED_EDGE('',*,*,#21064,.T.);
#30851=ORIENTED_EDGE('',*,*,#21067,.T.);
#30852=ORIENTED_EDGE('',*,*,#21381,.T.);
#30853=ORIENTED_EDGE('',*,*,#21382,.T.);
#30854=ORIENTED_EDGE('',*,*,#21383,.T.);
#30855=ORIENTED_EDGE('',*,*,#21384,.T.);
#30856=ORIENTED_EDGE('',*,*,#21385,.T.);
#30857=ORIENTED_EDGE('',*,*,#21386,.T.);
#30858=ORIENTED_EDGE('',*,*,#21387,.T.);
#30859=ORIENTED_EDGE('',*,*,#21388,.T.);
#30860=ORIENTED_EDGE('',*,*,#21194,.F.);
#30861=ORIENTED_EDGE('',*,*,#21389,.F.);
#30862=ORIENTED_EDGE('',*,*,#21388,.F.);
#30863=ORIENTED_EDGE('',*,*,#21390,.T.);
#30864=ORIENTED_EDGE('',*,*,#21196,.F.);
#30865=ORIENTED_EDGE('',*,*,#21391,.F.);
#30866=ORIENTED_EDGE('',*,*,#21386,.F.);
#30867=ORIENTED_EDGE('',*,*,#21392,.T.);
#30868=ORIENTED_EDGE('',*,*,#21195,.F.);
#30869=ORIENTED_EDGE('',*,*,#20769,.F.);
#30870=ORIENTED_EDGE('',*,*,#21192,.F.);
#30871=ORIENTED_EDGE('',*,*,#21390,.F.);
#30872=ORIENTED_EDGE('',*,*,#21387,.F.);
#30873=ORIENTED_EDGE('',*,*,#21391,.T.);
#30874=ORIENTED_EDGE('',*,*,#21201,.F.);
#30875=ORIENTED_EDGE('',*,*,#21393,.F.);
#30876=ORIENTED_EDGE('',*,*,#21383,.F.);
#30877=ORIENTED_EDGE('',*,*,#21394,.T.);
#30878=ORIENTED_EDGE('',*,*,#21199,.F.);
#30879=ORIENTED_EDGE('',*,*,#20773,.F.);
#30880=ORIENTED_EDGE('',*,*,#21200,.F.);
#30881=ORIENTED_EDGE('',*,*,#21394,.F.);
#30882=ORIENTED_EDGE('',*,*,#21382,.F.);
#30883=ORIENTED_EDGE('',*,*,#21395,.T.);
#30884=ORIENTED_EDGE('',*,*,#21188,.T.);
#30885=ORIENTED_EDGE('',*,*,#21376,.F.);
#30886=ORIENTED_EDGE('',*,*,#21363,.T.);
#30887=ORIENTED_EDGE('',*,*,#21366,.F.);
#30888=ORIENTED_EDGE('',*,*,#21368,.F.);
#30889=ORIENTED_EDGE('',*,*,#21370,.F.);
#30890=ORIENTED_EDGE('',*,*,#21372,.F.);
#30891=ORIENTED_EDGE('',*,*,#21374,.F.);
#30892=ORIENTED_EDGE('',*,*,#21378,.F.);
#30893=ORIENTED_EDGE('',*,*,#21165,.F.);
#30894=ORIENTED_EDGE('',*,*,#21204,.F.);
#30895=ORIENTED_EDGE('',*,*,#21212,.F.);
#30896=ORIENTED_EDGE('',*,*,#21214,.F.);
#30897=ORIENTED_EDGE('',*,*,#21159,.F.);
#30898=ORIENTED_EDGE('',*,*,#21213,.F.);
#30899=ORIENTED_EDGE('',*,*,#21220,.F.);
#30900=ORIENTED_EDGE('',*,*,#21222,.F.);
#30901=ORIENTED_EDGE('',*,*,#21154,.F.);
#30902=ORIENTED_EDGE('',*,*,#21221,.F.);
#30903=ORIENTED_EDGE('',*,*,#21230,.F.);
#30904=ORIENTED_EDGE('',*,*,#21235,.F.);
#30905=ORIENTED_EDGE('',*,*,#21265,.F.);
#30906=ORIENTED_EDGE('',*,*,#21231,.F.);
#30907=ORIENTED_EDGE('',*,*,#21241,.F.);
#30908=ORIENTED_EDGE('',*,*,#21205,.F.);
#30909=ORIENTED_EDGE('',*,*,#21048,.F.);
#30910=ORIENTED_EDGE('',*,*,#21051,.F.);
#30911=ORIENTED_EDGE('',*,*,#21056,.F.);
#30912=ORIENTED_EDGE('',*,*,#21059,.F.);
#30913=ORIENTED_EDGE('',*,*,#21062,.F.);
#30914=ORIENTED_EDGE('',*,*,#21065,.F.);
#30915=ORIENTED_EDGE('',*,*,#21124,.F.);
#30916=ORIENTED_EDGE('',*,*,#21146,.F.);
#30917=ORIENTED_EDGE('',*,*,#21143,.T.);
#30918=ORIENTED_EDGE('',*,*,#21140,.F.);
#30919=ORIENTED_EDGE('',*,*,#21137,.F.);
#30920=ORIENTED_EDGE('',*,*,#21134,.F.);
#30921=ORIENTED_EDGE('',*,*,#21131,.F.);
#30922=ORIENTED_EDGE('',*,*,#21128,.F.);
#30923=ORIENTED_EDGE('',*,*,#21100,.F.);
#30924=ORIENTED_EDGE('',*,*,#21122,.F.);
#30925=ORIENTED_EDGE('',*,*,#21119,.T.);
#30926=ORIENTED_EDGE('',*,*,#21116,.F.);
#30927=ORIENTED_EDGE('',*,*,#21113,.F.);
#30928=ORIENTED_EDGE('',*,*,#21110,.F.);
#30929=ORIENTED_EDGE('',*,*,#21107,.F.);
#30930=ORIENTED_EDGE('',*,*,#21104,.F.);
#30931=ORIENTED_EDGE('',*,*,#21076,.F.);
#30932=ORIENTED_EDGE('',*,*,#21098,.F.);
#30933=ORIENTED_EDGE('',*,*,#21095,.T.);
#30934=ORIENTED_EDGE('',*,*,#21092,.F.);
#30935=ORIENTED_EDGE('',*,*,#21089,.F.);
#30936=ORIENTED_EDGE('',*,*,#21086,.F.);
#30937=ORIENTED_EDGE('',*,*,#21083,.F.);
#30938=ORIENTED_EDGE('',*,*,#21080,.F.);
#30939=ORIENTED_EDGE('',*,*,#21339,.F.);
#30940=ORIENTED_EDGE('',*,*,#21361,.F.);
#30941=ORIENTED_EDGE('',*,*,#21358,.F.);
#30942=ORIENTED_EDGE('',*,*,#21355,.F.);
#30943=ORIENTED_EDGE('',*,*,#21352,.T.);
#30944=ORIENTED_EDGE('',*,*,#21349,.F.);
#30945=ORIENTED_EDGE('',*,*,#21346,.F.);
#30946=ORIENTED_EDGE('',*,*,#21343,.F.);
#30947=ORIENTED_EDGE('',*,*,#21315,.F.);
#30948=ORIENTED_EDGE('',*,*,#21337,.F.);
#30949=ORIENTED_EDGE('',*,*,#21334,.F.);
#30950=ORIENTED_EDGE('',*,*,#21331,.F.);
#30951=ORIENTED_EDGE('',*,*,#21328,.T.);
#30952=ORIENTED_EDGE('',*,*,#21325,.F.);
#30953=ORIENTED_EDGE('',*,*,#21322,.F.);
#30954=ORIENTED_EDGE('',*,*,#21319,.F.);
#30955=ORIENTED_EDGE('',*,*,#21291,.F.);
#30956=ORIENTED_EDGE('',*,*,#21313,.F.);
#30957=ORIENTED_EDGE('',*,*,#21310,.F.);
#30958=ORIENTED_EDGE('',*,*,#21307,.F.);
#30959=ORIENTED_EDGE('',*,*,#21304,.F.);
#30960=ORIENTED_EDGE('',*,*,#21301,.F.);
#30961=ORIENTED_EDGE('',*,*,#21298,.T.);
#30962=ORIENTED_EDGE('',*,*,#21295,.F.);
#30963=ORIENTED_EDGE('',*,*,#21267,.F.);
#30964=ORIENTED_EDGE('',*,*,#21289,.F.);
#30965=ORIENTED_EDGE('',*,*,#21286,.F.);
#30966=ORIENTED_EDGE('',*,*,#21283,.F.);
#30967=ORIENTED_EDGE('',*,*,#21280,.F.);
#30968=ORIENTED_EDGE('',*,*,#21277,.T.);
#30969=ORIENTED_EDGE('',*,*,#21274,.F.);
#30970=ORIENTED_EDGE('',*,*,#21271,.F.);
#30971=ORIENTED_EDGE('',*,*,#21202,.F.);
#30972=ORIENTED_EDGE('',*,*,#20771,.F.);
#30973=ORIENTED_EDGE('',*,*,#21197,.F.);
#30974=ORIENTED_EDGE('',*,*,#21392,.F.);
#30975=ORIENTED_EDGE('',*,*,#21385,.F.);
#30976=ORIENTED_EDGE('',*,*,#21396,.T.);
#30977=ORIENTED_EDGE('',*,*,#21198,.F.);
#30978=ORIENTED_EDGE('',*,*,#21395,.F.);
#30979=ORIENTED_EDGE('',*,*,#21381,.F.);
#30980=ORIENTED_EDGE('',*,*,#21389,.T.);
#30981=ORIENTED_EDGE('',*,*,#21193,.F.);
#30982=ORIENTED_EDGE('',*,*,#20775,.F.);
#30983=ORIENTED_EDGE('',*,*,#21203,.F.);
#30984=ORIENTED_EDGE('',*,*,#21396,.F.);
#30985=ORIENTED_EDGE('',*,*,#21384,.F.);
#30986=ORIENTED_EDGE('',*,*,#21393,.T.);
#30987=ORIENTED_EDGE('',*,*,#20807,.T.);
#30988=ORIENTED_EDGE('',*,*,#20486,.F.);
#30989=ORIENTED_EDGE('',*,*,#21397,.F.);
#30990=ORIENTED_EDGE('',*,*,#21398,.F.);
#30991=ORIENTED_EDGE('',*,*,#21399,.T.);
#30992=ORIENTED_EDGE('',*,*,#21400,.T.);
#30993=ORIENTED_EDGE('',*,*,#21399,.F.);
#30994=ORIENTED_EDGE('',*,*,#21397,.T.);
#30995=ORIENTED_EDGE('',*,*,#21398,.T.);
#30996=ORIENTED_EDGE('',*,*,#21401,.T.);
#30997=ORIENTED_EDGE('',*,*,#21402,.F.);
#30998=ORIENTED_EDGE('',*,*,#21403,.F.);
#30999=ORIENTED_EDGE('',*,*,#21401,.F.);
#31000=ORIENTED_EDGE('',*,*,#21403,.T.);
#31001=ORIENTED_EDGE('',*,*,#21404,.T.);
#31002=ORIENTED_EDGE('',*,*,#21187,.F.);
#31003=ORIENTED_EDGE('',*,*,#21404,.F.);
#31004=ORIENTED_EDGE('',*,*,#21402,.T.);
#31005=ORIENTED_EDGE('',*,*,#21405,.T.);
#31006=ORIENTED_EDGE('',*,*,#21406,.F.);
#31007=ORIENTED_EDGE('',*,*,#21407,.F.);
#31008=ORIENTED_EDGE('',*,*,#21408,.T.);
#31009=ORIENTED_EDGE('',*,*,#21409,.T.);
#31010=ORIENTED_EDGE('',*,*,#21410,.F.);
#31011=ORIENTED_EDGE('',*,*,#21411,.F.);
#31012=ORIENTED_EDGE('',*,*,#21406,.T.);
#31013=ORIENTED_EDGE('',*,*,#21412,.T.);
#31014=ORIENTED_EDGE('',*,*,#21413,.F.);
#31015=ORIENTED_EDGE('',*,*,#21414,.F.);
#31016=ORIENTED_EDGE('',*,*,#21410,.T.);
#31017=ORIENTED_EDGE('',*,*,#21413,.T.);
#31018=ORIENTED_EDGE('',*,*,#21415,.F.);
#31019=ORIENTED_EDGE('',*,*,#21416,.F.);
#31020=ORIENTED_EDGE('',*,*,#21417,.F.);
#31021=ORIENTED_EDGE('',*,*,#21418,.T.);
#31022=ORIENTED_EDGE('',*,*,#21419,.F.);
#31023=ORIENTED_EDGE('',*,*,#21420,.F.);
#31024=ORIENTED_EDGE('',*,*,#21416,.T.);
#31025=ORIENTED_EDGE('',*,*,#21407,.T.);
#31026=ORIENTED_EDGE('',*,*,#21411,.T.);
#31027=ORIENTED_EDGE('',*,*,#21414,.T.);
#31028=ORIENTED_EDGE('',*,*,#21417,.T.);
#31029=ORIENTED_EDGE('',*,*,#21420,.T.);
#31030=ORIENTED_EDGE('',*,*,#21421,.T.);
#31031=ORIENTED_EDGE('',*,*,#21422,.T.);
#31032=ORIENTED_EDGE('',*,*,#21408,.F.);
#31033=ORIENTED_EDGE('',*,*,#21421,.F.);
#31034=ORIENTED_EDGE('',*,*,#21419,.T.);
#31035=ORIENTED_EDGE('',*,*,#21400,.F.);
#31036=ORIENTED_EDGE('',*,*,#21412,.F.);
#31037=ORIENTED_EDGE('',*,*,#21409,.F.);
#31038=ORIENTED_EDGE('',*,*,#21405,.F.);
#31039=ORIENTED_EDGE('',*,*,#21422,.F.);
#31040=ORIENTED_EDGE('',*,*,#21418,.F.);
#31041=ORIENTED_EDGE('',*,*,#21415,.T.);
#31042=ORIENTED_EDGE('',*,*,#21423,.F.);
#31043=ORIENTED_EDGE('',*,*,#21424,.T.);
#31044=ORIENTED_EDGE('',*,*,#21425,.F.);
#31045=ORIENTED_EDGE('',*,*,#21424,.F.);
#31046=ORIENTED_EDGE('',*,*,#21426,.F.);
#31047=ORIENTED_EDGE('',*,*,#21427,.F.);
#31048=ORIENTED_EDGE('',*,*,#21428,.F.);
#31049=ORIENTED_EDGE('',*,*,#21429,.T.);
#31050=ORIENTED_EDGE('',*,*,#21430,.F.);
#31051=ORIENTED_EDGE('',*,*,#21429,.F.);
#31052=ORIENTED_EDGE('',*,*,#21431,.F.);
#31053=ORIENTED_EDGE('',*,*,#21432,.T.);
#31054=ORIENTED_EDGE('',*,*,#21433,.F.);
#31055=ORIENTED_EDGE('',*,*,#21432,.F.);
#31056=ORIENTED_EDGE('',*,*,#21426,.T.);
#31057=ORIENTED_EDGE('',*,*,#21434,.T.);
#31058=ORIENTED_EDGE('',*,*,#21435,.F.);
#31059=ORIENTED_EDGE('',*,*,#21436,.F.);
#31060=ORIENTED_EDGE('',*,*,#21434,.F.);
#31061=ORIENTED_EDGE('',*,*,#21427,.T.);
#31062=ORIENTED_EDGE('',*,*,#21437,.T.);
#31063=ORIENTED_EDGE('',*,*,#21438,.F.);
#31064=ORIENTED_EDGE('',*,*,#21439,.F.);
#31065=ORIENTED_EDGE('',*,*,#21437,.F.);
#31066=ORIENTED_EDGE('',*,*,#21440,.T.);
#31067=ORIENTED_EDGE('',*,*,#21425,.T.);
#31068=ORIENTED_EDGE('',*,*,#21440,.F.);
#31069=ORIENTED_EDGE('',*,*,#21441,.T.);
#31070=ORIENTED_EDGE('',*,*,#21442,.F.);
#31071=ORIENTED_EDGE('',*,*,#21441,.F.);
#31072=ORIENTED_EDGE('',*,*,#21428,.T.);
#31073=ORIENTED_EDGE('',*,*,#21431,.T.);
#31074=ORIENTED_EDGE('',*,*,#21443,.F.);
#31075=ORIENTED_EDGE('',*,*,#21444,.F.);
#31076=ORIENTED_EDGE('',*,*,#21445,.T.);
#31077=ORIENTED_EDGE('',*,*,#21446,.F.);
#31078=ORIENTED_EDGE('',*,*,#21447,.F.);
#31079=ORIENTED_EDGE('',*,*,#21445,.F.);
#31080=ORIENTED_EDGE('',*,*,#21435,.T.);
#31081=ORIENTED_EDGE('',*,*,#21436,.T.);
#31082=ORIENTED_EDGE('',*,*,#21438,.T.);
#31083=ORIENTED_EDGE('',*,*,#21439,.T.);
#31084=ORIENTED_EDGE('',*,*,#21443,.T.);
#31085=ORIENTED_EDGE('',*,*,#21444,.T.);
#31086=ORIENTED_EDGE('',*,*,#21448,.T.);
#31087=ORIENTED_EDGE('',*,*,#21449,.T.);
#31088=ORIENTED_EDGE('',*,*,#21448,.F.);
#31089=ORIENTED_EDGE('',*,*,#21449,.F.);
#31090=ORIENTED_EDGE('',*,*,#21423,.T.);
#31091=ORIENTED_EDGE('',*,*,#21450,.T.);
#31092=ORIENTED_EDGE('',*,*,#21451,.T.);
#31093=ORIENTED_EDGE('',*,*,#21452,.T.);
#31094=ORIENTED_EDGE('',*,*,#21453,.T.);
#31095=ORIENTED_EDGE('',*,*,#21452,.F.);
#31096=ORIENTED_EDGE('',*,*,#21450,.F.);
#31097=ORIENTED_EDGE('',*,*,#21451,.F.);
#31098=ORIENTED_EDGE('',*,*,#21454,.T.);
#31099=ORIENTED_EDGE('',*,*,#21455,.F.);
#31100=ORIENTED_EDGE('',*,*,#21456,.F.);
#31101=ORIENTED_EDGE('',*,*,#21454,.F.);
#31102=ORIENTED_EDGE('',*,*,#21430,.T.);
#31103=ORIENTED_EDGE('',*,*,#21433,.T.);
#31104=ORIENTED_EDGE('',*,*,#21453,.F.);
#31105=ORIENTED_EDGE('',*,*,#21442,.T.);
#31106=ORIENTED_EDGE('',*,*,#21456,.T.);
#31107=ORIENTED_EDGE('',*,*,#21457,.T.);
#31108=ORIENTED_EDGE('',*,*,#21446,.T.);
#31109=ORIENTED_EDGE('',*,*,#21447,.T.);
#31110=ORIENTED_EDGE('',*,*,#21457,.F.);
#31111=ORIENTED_EDGE('',*,*,#21455,.T.);
#31112=PLANE('',#34118);
#31113=PLANE('',#34119);
#31114=PLANE('',#34120);
#31115=PLANE('',#34121);
#31116=PLANE('',#34131);
#31117=PLANE('',#34134);
#31118=PLANE('',#34135);
#31119=PLANE('',#34136);
#31120=PLANE('',#34139);
#31121=PLANE('',#34140);
#31122=PLANE('',#34147);
#31123=PLANE('',#34148);
#31124=PLANE('',#34149);
#31125=PLANE('',#34152);
#31126=PLANE('',#34154);
#31127=PLANE('',#34175);
#31128=PLANE('',#34179);
#31129=PLANE('',#34183);
#31130=PLANE('',#34186);
#31131=PLANE('',#34214);
#31132=PLANE('',#34215);
#31133=PLANE('',#34217);
#31134=PLANE('',#34219);
#31135=PLANE('',#34235);
#31136=PLANE('',#34243);
#31137=PLANE('',#34293);
#31138=PLANE('',#34301);
#31139=PLANE('',#34347);
#31140=PLANE('',#34355);
#31141=PLANE('',#34359);
#31142=PLANE('',#34363);
#31143=PLANE('',#34367);
#31144=PLANE('',#34371);
#31145=PLANE('',#34375);
#31146=PLANE('',#34379);
#31147=PLANE('',#34385);
#31148=PLANE('',#34387);
#31149=PLANE('',#34389);
#31150=PLANE('',#34391);
#31151=PLANE('',#34401);
#31152=PLANE('',#34405);
#31153=PLANE('',#34411);
#31154=PLANE('',#34413);
#31155=PLANE('',#34414);
#31156=PLANE('',#34415);
#31157=PLANE('',#34416);
#31158=PLANE('',#34417);
#31159=PLANE('',#34418);
#31160=PLANE('',#34429);
#31161=PLANE('',#34433);
#31162=PLANE('',#34439);
#31163=PLANE('',#34441);
#31164=PLANE('',#34442);
#31165=PLANE('',#34443);
#31166=PLANE('',#34444);
#31167=PLANE('',#34445);
#31168=PLANE('',#34446);
#31169=PLANE('',#34457);
#31170=PLANE('',#34461);
#31171=PLANE('',#34467);
#31172=PLANE('',#34469);
#31173=PLANE('',#34470);
#31174=PLANE('',#34471);
#31175=PLANE('',#34472);
#31176=PLANE('',#34473);
#31177=PLANE('',#34474);
#31178=PLANE('',#34485);
#31179=PLANE('',#34489);
#31180=PLANE('',#34502);
#31181=PLANE('',#34503);
#31182=PLANE('',#34504);
#31183=PLANE('',#34505);
#31184=PLANE('',#34507);
#31185=PLANE('',#34508);
#31186=PLANE('',#34509);
#31187=PLANE('',#34510);
#31188=PLANE('',#34513);
#31189=PLANE('',#34514);
#31190=PLANE('',#34515);
#31191=PLANE('',#34516);
#31192=PLANE('',#34517);
#31193=PLANE('',#34518);
#31194=PLANE('',#34519);
#31195=PLANE('',#34520);
#31196=PLANE('',#34521);
#31197=PLANE('',#34522);
#31198=PLANE('',#34523);
#31199=PLANE('',#34524);
#31200=PLANE('',#34525);
#31201=PLANE('',#34526);
#31202=PLANE('',#34527);
#31203=PLANE('',#34547);
#31204=PLANE('',#34548);
#31205=PLANE('',#34549);
#31206=PLANE('',#34550);
#31207=PLANE('',#34551);
#31208=PLANE('',#34552);
#31209=PLANE('',#34553);
#31210=PLANE('',#34554);
#31211=PLANE('',#34555);
#31212=PLANE('',#34556);
#31213=PLANE('',#34557);
#31214=PLANE('',#34558);
#31215=PLANE('',#34559);
#31216=PLANE('',#34560);
#31217=PLANE('',#34561);
#31218=PLANE('',#34562);
#31219=PLANE('',#34563);
#31220=PLANE('',#34564);
#31221=PLANE('',#34565);
#31222=PLANE('',#34566);
#31223=PLANE('',#34567);
#31224=PLANE('',#34571);
#31225=PLANE('',#34572);
#31226=PLANE('',#34573);
#31227=PLANE('',#34574);
#31228=PLANE('',#34585);
#31229=PLANE('',#34586);
#31230=PLANE('',#34595);
#31231=PLANE('',#34609);
#31232=PLANE('',#34611);
#31233=PLANE('',#34613);
#31234=PLANE('',#34620);
#31235=PLANE('',#34622);
#31236=PLANE('',#34624);
#31237=PLANE('',#34626);
#31238=PLANE('',#34628);
#31239=PLANE('',#34630);
#31240=PLANE('',#34632);
#31241=PLANE('',#34634);
#31242=PLANE('',#34636);
#31243=PLANE('',#34638);
#31244=PLANE('',#34640);
#31245=PLANE('',#34642);
#31246=PLANE('',#34644);
#31247=PLANE('',#34646);
#31248=PLANE('',#34651);
#31249=PLANE('',#34655);
#31250=PLANE('',#34659);
#31251=PLANE('',#34663);
#31252=PLANE('',#34664);
#31253=PLANE('',#34665);
#31254=PLANE('',#34674);
#31255=PLANE('',#34677);
#31256=PLANE('',#34680);
#31257=PLANE('',#34683);
#31258=PLANE('',#34684);
#31259=PLANE('',#34715);
#31260=PLANE('',#34716);
#31261=PLANE('',#34717);
#31262=PLANE('',#34718);
#31263=PLANE('',#34719);
#31264=PLANE('',#34720);
#31265=PLANE('',#34721);
#31266=PLANE('',#34722);
#31267=PLANE('',#34723);
#31268=PLANE('',#34724);
#31269=PLANE('',#34725);
#31270=PLANE('',#34726);
#31271=PLANE('',#34727);
#31272=PLANE('',#34728);
#31273=PLANE('',#34729);
#31274=PLANE('',#34730);
#31275=PLANE('',#34731);
#31276=PLANE('',#34732);
#31277=PLANE('',#34733);
#31278=PLANE('',#34734);
#31279=PLANE('',#34735);
#31280=PLANE('',#34736);
#31281=PLANE('',#34737);
#31282=PLANE('',#34738);
#31283=PLANE('',#34739);
#31284=PLANE('',#34740);
#31285=PLANE('',#34741);
#31286=PLANE('',#34742);
#31287=PLANE('',#34743);
#31288=PLANE('',#34744);
#31289=PLANE('',#34745);
#31290=PLANE('',#34746);
#31291=PLANE('',#34747);
#31292=PLANE('',#34748);
#31293=PLANE('',#34749);
#31294=PLANE('',#34750);
#31295=PLANE('',#34752);
#31296=PLANE('',#34753);
#31297=PLANE('',#34755);
#31298=PLANE('',#34758);
#31299=PLANE('',#34760);
#31300=PLANE('',#34762);
#31301=PLANE('',#34764);
#31302=PLANE('',#34766);
#31303=PLANE('',#34767);
#31304=PLANE('',#34769);
#31305=PLANE('',#34770);
#31306=PLANE('',#34771);
#31307=PLANE('',#34772);
#31308=PLANE('',#34773);
#31309=PLANE('',#34774);
#31310=PLANE('',#34775);
#31311=PLANE('',#34776);
#31312=PLANE('',#34777);
#31313=PLANE('',#34778);
#31314=PLANE('',#34779);
#31315=PLANE('',#34780);
#31316=PLANE('',#34783);
#31317=PLANE('',#34784);
#31318=PLANE('',#34785);
#31319=PLANE('',#34797);
#31320=PLANE('',#34798);
#31321=PLANE('',#34799);
#31322=PLANE('',#34800);
#31323=PLANE('',#34801);
#31324=PLANE('',#34802);
#31325=PLANE('',#34803);
#31326=PLANE('',#34804);
#31327=PLANE('',#34805);
#31328=PLANE('',#34806);
#31329=PLANE('',#34807);
#31330=PLANE('',#34808);
#31331=PLANE('',#34814);
#31332=PLANE('',#34820);
#31333=PLANE('',#34826);
#31334=PLANE('',#34837);
#31335=PLANE('',#34838);
#31336=PLANE('',#34843);
#31337=PLANE('',#34845);
#31338=PLANE('',#34846);
#31339=PLANE('',#34848);
#31340=PLANE('',#34849);
#31341=PLANE('',#34850);
#31342=PLANE('',#34857);
#31343=PLANE('',#34860);
#31344=PLANE('',#34861);
#31345=PLANE('',#34868);
#31346=PLANE('',#34871);
#31347=PLANE('',#34872);
#31348=PLANE('',#34879);
#31349=PLANE('',#34886);
#31350=PLANE('',#34893);
#31351=PLANE('',#34902);
#31352=PLANE('',#34910);
#31353=PLANE('',#34914);
#31354=PLANE('',#34918);
#31355=PLANE('',#34921);
#31356=PLANE('',#34927);
#31357=PLANE('',#34930);
#31358=PLANE('',#34934);
#31359=PLANE('',#34935);
#31360=PLANE('',#34939);
#31361=PLANE('',#34944);
#31362=PLANE('',#34948);
#31363=PLANE('',#34949);
#31364=PLANE('',#34953);
#31365=PLANE('',#34954);
#31366=PLANE('',#34963);
#31367=PLANE('',#34970);
#31368=PLANE('',#34986);
#31369=PLANE('',#35009);
#31370=PLANE('',#35010);
#31371=PLANE('',#35011);
#31372=PLANE('',#35012);
#31373=PLANE('',#35013);
#31374=PLANE('',#35014);
#31375=PLANE('',#35015);
#31376=PLANE('',#35016);
#31377=PLANE('',#35017);
#31378=PLANE('',#35018);
#31379=PLANE('',#35019);
#31380=PLANE('',#35020);
#31381=PLANE('',#35021);
#31382=PLANE('',#35022);
#31383=PLANE('',#35023);
#31384=PLANE('',#35024);
#31385=PLANE('',#35025);
#31386=PLANE('',#35026);
#31387=PLANE('',#35027);
#31388=PLANE('',#35028);
#31389=PLANE('',#35029);
#31390=PLANE('',#35030);
#31391=PLANE('',#35031);
#31392=PLANE('',#35032);
#31393=PLANE('',#35033);
#31394=PLANE('',#35034);
#31395=PLANE('',#35035);
#31396=PLANE('',#35036);
#31397=PLANE('',#35037);
#31398=PLANE('',#35038);
#31399=PLANE('',#35039);
#31400=PLANE('',#35044);
#31401=PLANE('',#35052);
#31402=PLANE('',#35061);
#31403=PLANE('',#35062);
#31404=PLANE('',#35064);
#31405=PLANE('',#35140);
#31406=PLANE('',#35141);
#31407=PLANE('',#35142);
#31408=PLANE('',#35143);
#31409=PLANE('',#35148);
#31410=PLANE('',#35149);
#31411=PLANE('',#35150);
#31412=PLANE('',#35151);
#31413=PLANE('',#35176);
#31414=PLANE('',#35177);
#31415=PLANE('',#35178);
#31416=PLANE('',#35179);
#31417=PLANE('',#35180);
#31418=PLANE('',#35181);
#31419=PLANE('',#35182);
#31420=PLANE('',#35183);
#31421=PLANE('',#35184);
#31422=PLANE('',#35185);
#31423=PLANE('',#35186);
#31424=PLANE('',#35187);
#31425=PLANE('',#35188);
#31426=PLANE('',#35189);
#31427=PLANE('',#35190);
#31428=PLANE('',#35192);
#31429=PLANE('',#35196);
#31430=PLANE('',#35200);
#31431=PLANE('',#35204);
#31432=PLANE('',#35208);
#31433=PLANE('',#35212);
#31434=PLANE('',#35216);
#31435=PLANE('',#35220);
#31436=PLANE('',#35224);
#31437=PLANE('',#35225);
#31438=PLANE('',#35226);
#31439=PLANE('',#35230);
#31440=PLANE('',#35234);
#31441=PLANE('',#35238);
#31442=PLANE('',#35242);
#31443=PLANE('',#35246);
#31444=PLANE('',#35250);
#31445=PLANE('',#35254);
#31446=PLANE('',#35258);
#31447=PLANE('',#35259);
#31448=PLANE('',#35260);
#31449=PLANE('',#35264);
#31450=PLANE('',#35268);
#31451=PLANE('',#35272);
#31452=PLANE('',#35276);
#31453=PLANE('',#35280);
#31454=PLANE('',#35284);
#31455=PLANE('',#35288);
#31456=PLANE('',#35292);
#31457=PLANE('',#35293);
#31458=PLANE('',#35294);
#31459=PLANE('',#35298);
#31460=PLANE('',#35302);
#31461=PLANE('',#35306);
#31462=PLANE('',#35310);
#31463=PLANE('',#35314);
#31464=PLANE('',#35318);
#31465=PLANE('',#35322);
#31466=PLANE('',#35326);
#31467=PLANE('',#35327);
#31468=PLANE('',#35328);
#31469=PLANE('',#35337);
#31470=PLANE('',#35340);
#31471=PLANE('',#35347);
#31472=PLANE('',#35348);
#31473=PLANE('',#35353);
#31474=PLANE('',#35356);
#31475=PLANE('',#35358);
#31476=PLANE('',#35359);
#31477=PLANE('',#35361);
#31478=PLANE('',#35362);
#31479=PLANE('',#35371);
#31480=PLANE('',#35374);
#31481=PLANE('',#35379);
#31482=PLANE('',#35382);
#31483=PLANE('',#35383);
#31484=PLANE('',#35388);
#31485=PLANE('',#35391);
#31486=PLANE('',#35393);
#31487=PLANE('',#35395);
#31488=PLANE('',#35396);
#31489=PLANE('',#35405);
#31490=PLANE('',#35408);
#31491=PLANE('',#35411);
#31492=PLANE('',#35414);
#31493=PLANE('',#35417);
#31494=PLANE('',#35422);
#31495=PLANE('',#35423);
#31496=PLANE('',#35425);
#31497=PLANE('',#35428);
#31498=PLANE('',#35430);
#31499=PLANE('',#35439);
#31500=PLANE('',#35442);
#31501=PLANE('',#35445);
#31502=PLANE('',#35448);
#31503=PLANE('',#35451);
#31504=PLANE('',#35456);
#31505=PLANE('',#35457);
#31506=PLANE('',#35459);
#31507=PLANE('',#35462);
#31508=PLANE('',#35464);
#31509=PLANE('',#35468);
#31510=PLANE('',#35472);
#31511=PLANE('',#35476);
#31512=PLANE('',#35480);
#31513=PLANE('',#35484);
#31514=PLANE('',#35488);
#31515=PLANE('',#35492);
#31516=PLANE('',#35496);
#31517=PLANE('',#35497);
#31518=PLANE('',#35498);
#31519=PLANE('',#35502);
#31520=PLANE('',#35506);
#31521=PLANE('',#35510);
#31522=PLANE('',#35514);
#31523=PLANE('',#35518);
#31524=PLANE('',#35522);
#31525=PLANE('',#35526);
#31526=PLANE('',#35530);
#31527=PLANE('',#35531);
#31528=PLANE('',#35532);
#31529=PLANE('',#35536);
#31530=PLANE('',#35540);
#31531=PLANE('',#35544);
#31532=PLANE('',#35548);
#31533=PLANE('',#35552);
#31534=PLANE('',#35556);
#31535=PLANE('',#35560);
#31536=PLANE('',#35564);
#31537=PLANE('',#35565);
#31538=PLANE('',#35569);
#31539=PLANE('',#35573);
#31540=PLANE('',#35577);
#31541=PLANE('',#35581);
#31542=PLANE('',#35585);
#31543=PLANE('',#35589);
#31544=PLANE('',#35593);
#31545=PLANE('',#35597);
#31546=PLANE('',#35598);
#31547=PLANE('',#35599);
#31548=PLANE('',#35603);
#31549=PLANE('',#35607);
#31550=PLANE('',#35611);
#31551=PLANE('',#35615);
#31552=PLANE('',#35619);
#31553=PLANE('',#35623);
#31554=PLANE('',#35627);
#31555=PLANE('',#35631);
#31556=PLANE('',#35632);
#31557=PLANE('',#35633);
#31558=PLANE('',#35637);
#31559=PLANE('',#35641);
#31560=PLANE('',#35645);
#31561=PLANE('',#35649);
#31562=PLANE('',#35653);
#31563=PLANE('',#35657);
#31564=PLANE('',#35661);
#31565=PLANE('',#35665);
#31566=PLANE('',#35666);
#31567=PLANE('',#35667);
#31568=PLANE('',#35671);
#31569=PLANE('',#35675);
#31570=PLANE('',#35679);
#31571=PLANE('',#35683);
#31572=PLANE('',#35687);
#31573=PLANE('',#35691);
#31574=PLANE('',#35695);
#31575=PLANE('',#35699);
#31576=PLANE('',#35700);
#31577=PLANE('',#35701);
#31578=PLANE('',#35752);
#31579=PLANE('',#35753);
#31580=PLANE('',#35754);
#31581=PLANE('',#35755);
#31582=PLANE('',#35756);
#31583=PLANE('',#35757);
#31584=PLANE('',#35758);
#31585=PLANE('',#35759);
#31586=PLANE('',#35760);
#31587=PLANE('',#35761);
#31588=PLANE('',#35763);
#31589=PLANE('',#35767);
#31590=PLANE('',#35771);
#31591=PLANE('',#35820);
#31592=PLANE('',#35821);
#31593=PLANE('',#35822);
#31594=PLANE('',#35824);
#31595=PLANE('',#35828);
#31596=PLANE('',#35832);
#31597=PLANE('',#35881);
#31598=PLANE('',#35882);
#31599=PLANE('',#35883);
#31600=PLANE('',#35903);
#31601=PLANE('',#35904);
#31602=PLANE('',#35905);
#31603=PLANE('',#35906);
#31604=PLANE('',#35907);
#31605=PLANE('',#35908);
#31606=PLANE('',#35910);
#31607=PLANE('',#35911);
#31608=PLANE('',#35912);
#31609=PLANE('',#35916);
#31610=PLANE('',#35917);
#31611=PLANE('',#35918);
#31612=PLANE('',#35919);
#31613=PLANE('',#35920);
#31614=PLANE('',#35921);
#31615=PLANE('',#35935);
#31616=PLANE('',#35936);
#31617=PLANE('',#35937);
#31618=PLANE('',#35938);
#31619=PLANE('',#35939);
#31620=PLANE('',#35940);
#31621=PLANE('',#35941);
#31622=PLANE('',#35942);
#31623=PLANE('',#35943);
#31624=PLANE('',#35944);
#31625=PLANE('',#35968);
#31626=PLANE('',#35969);
#31627=PLANE('',#35972);
#31628=PLANE('',#35978);
#31629=PLANE('',#35987);
#31630=PLANE('',#36006);
#31631=PLANE('',#36009);
#31632=PLANE('',#36010);
#31633=PLANE('',#36013);
#31634=PLANE('',#36019);
#31635=PLANE('',#36023);
#31636=PLANE('',#36028);
#31637=PLANE('',#36042);
#31638=PLANE('',#36050);
#31639=PLANE('',#36051);
#31640=PLANE('',#36054);
#31641=PLANE('',#36057);
#31642=PLANE('',#36062);
#31643=PLANE('',#36077);
#31644=PLANE('',#36087);
#31645=PLANE('',#36090);
#31646=PLANE('',#36091);
#31647=PLANE('',#36094);
#31648=PLANE('',#36101);
#31649=PLANE('',#36106);
#31650=PLANE('',#36111);
#31651=PLANE('',#36112);
#31652=PLANE('',#36113);
#31653=PLANE('',#36114);
#31654=PLANE('',#36121);
#31655=PLANE('',#36129);
#31656=PLANE('',#36130);
#31657=PLANE('',#36156);
#31658=PLANE('',#36161);
#31659=PLANE('',#36354);
#31660=PLANE('',#36355);
#31661=PLANE('',#36358);
#31662=PLANE('',#36743);
#31663=PLANE('',#36752);
#31664=PLANE('',#36757);
#31665=PLANE('',#36918);
#31666=PLANE('',#36919);
#31667=PLANE('',#36922);
#31668=PLANE('',#37243);
#31669=PLANE('',#37252);
#31670=PLANE('',#37260);
#31671=PLANE('',#37262);
#31672=PLANE('',#37269);
#31673=PLANE('',#37277);
#31674=PLANE('',#37279);
#31675=PLANE('',#37286);
#31676=PLANE('',#37294);
#31677=PLANE('',#37298);
#31678=PLANE('',#37302);
#31679=PLANE('',#37306);
#31680=PLANE('',#37311);
#31681=PLANE('',#37319);
#31682=PLANE('',#37323);
#31683=PLANE('',#37328);
#31684=PLANE('',#37333);
#31685=PLANE('',#37337);
#31686=PLANE('',#37341);
#31687=PLANE('',#37342);
#31688=PLANE('',#37343);
#31689=PLANE('',#37345);
#31690=PLANE('',#37347);
#31691=PLANE('',#37348);
#31692=PLANE('',#37358);
#31693=PLANE('',#37360);
#31694=PLANE('',#37367);
#31695=PLANE('',#37369);
#31696=PLANE('',#37375);
#31697=PLANE('',#37376);
#31698=PLANE('',#37380);
#31699=PLANE('',#37383);
#31700=PLANE('',#37398);
#31701=PLANE('',#37399);
#31702=PLANE('',#37400);
#31703=PLANE('',#37401);
#31704=PLANE('',#37402);
#31705=PLANE('',#37403);
#31706=PLANE('',#37406);
#31707=PLANE('',#37424);
#31708=PLANE('',#37425);
#31709=PLANE('',#37426);
#31710=PLANE('',#37427);
#31711=PLANE('',#37430);
#31712=PLANE('',#37435);
#31713=PLANE('',#37436);
#31714=PLANE('',#37437);
#31715=PLANE('',#37438);
#31716=PLANE('',#37439);
#31717=PLANE('',#37450);
#31718=PLANE('',#37451);
#31719=PLANE('',#37454);
#31720=PLANE('',#37455);
#31721=PLANE('',#37456);
#31722=PLANE('',#37457);
#31723=PLANE('',#37458);
#31724=PLANE('',#37469);
#31725=PLANE('',#37470);
#31726=PLANE('',#37473);
#31727=PLANE('',#37474);
#31728=PLANE('',#37475);
#31729=PLANE('',#37476);
#31730=PLANE('',#37477);
#31731=PLANE('',#37478);
#31732=PLANE('',#37479);
#31733=PLANE('',#37480);
#31734=PLANE('',#37481);
#31735=PLANE('',#37483);
#31736=PLANE('',#37490);
#31737=PLANE('',#37491);
#31738=PLANE('',#37492);
#31739=PLANE('',#37493);
#31740=PLANE('',#37494);
#31741=PLANE('',#37495);
#31742=PLANE('',#37496);
#31743=PLANE('',#37499);
#31744=PLANE('',#37500);
#31745=PLANE('',#37501);
#31746=PLANE('',#37502);
#31747=PLANE('',#37503);
#31748=PLANE('',#37504);
#31749=PLANE('',#37505);
#31750=PLANE('',#37506);
#31751=PLANE('',#37509);
#31752=PLANE('',#37510);
#31753=PLANE('',#37511);
#31754=PLANE('',#37512);
#31755=PLANE('',#37513);
#31756=PLANE('',#37580);
#31757=PLANE('',#37581);
#31758=PLANE('',#37582);
#31759=PLANE('',#37583);
#31760=PLANE('',#37584);
#31761=PLANE('',#37585);
#31762=PLANE('',#37586);
#31763=PLANE('',#37587);
#31764=PLANE('',#37588);
#31765=PLANE('',#37589);
#31766=PLANE('',#37598);
#31767=PLANE('',#37599);
#31768=PLANE('',#37600);
#31769=PLANE('',#37601);
#31770=PLANE('',#37602);
#31771=PLANE('',#37603);
#31772=PLANE('',#37604);
#31773=PLANE('',#37605);
#31774=PLANE('',#37606);
#31775=PLANE('',#37607);
#31776=PLANE('',#37608);
#31777=PLANE('',#37627);
#31778=PLANE('',#37628);
#31779=PLANE('',#37632);
#31780=PLANE('',#37641);
#31781=PLANE('',#37645);
#31782=PLANE('',#37653);
#31783=PLANE('',#37654);
#31784=PLANE('',#37655);
#31785=PLANE('',#37656);
#31786=PLANE('',#37657);
#31787=PLANE('',#37658);
#31788=PLANE('',#37659);
#31789=PLANE('',#37660);
#31790=PLANE('',#37661);
#31791=PLANE('',#37662);
#31792=PLANE('',#37663);
#31793=PLANE('',#37664);
#31794=PLANE('',#37665);
#31795=PLANE('',#37666);
#31796=PLANE('',#37667);
#31797=PLANE('',#37668);
#31798=PLANE('',#37678);
#31799=PLANE('',#37679);
#31800=PLANE('',#37684);
#31801=PLANE('',#37685);
#31802=PLANE('',#37686);
#31803=PLANE('',#37687);
#31804=PLANE('',#37688);
#31805=PLANE('',#37689);
#31806=PLANE('',#37690);
#31807=PLANE('',#37691);
#31808=PLANE('',#37692);
#31809=PLANE('',#37693);
#31810=PLANE('',#37694);
#31811=PLANE('',#37695);
#31812=PLANE('',#37696);
#31813=PLANE('',#37697);
#31814=PLANE('',#37698);
#31815=PLANE('',#37708);
#31816=PLANE('',#37709);
#31817=PLANE('',#37717);
#31818=PLANE('',#37720);
#31819=PLANE('',#37729);
#31820=PLANE('',#37731);
#31821=PLANE('',#37734);
#31822=PLANE('',#37736);
#31823=PLANE('',#37741);
#31824=PLANE('',#37742);
#31825=PLANE('',#37745);
#31826=PLANE('',#37753);
#31827=PLANE('',#37754);
#31828=PLANE('',#37760);
#31829=PLANE('',#37761);
#31830=PLANE('',#37762);
#31831=PLANE('',#37763);
#31832=PLANE('',#37764);
#31833=PLANE('',#37772);
#31834=PLANE('',#37773);
#31835=PLANE('',#37779);
#31836=PLANE('',#37780);
#31837=PLANE('',#37781);
#31838=PLANE('',#37782);
#31839=PLANE('',#37783);
#31840=PLANE('',#37785);
#31841=PLANE('',#37787);
#31842=PLANE('',#37809);
#31843=PLANE('',#37816);
#31844=PLANE('',#37826);
#31845=PLANE('',#37836);
#31846=PLANE('',#37837);
#31847=PLANE('',#37847);
#31848=PLANE('',#37857);
#31849=PLANE('',#37858);
#31850=PLANE('',#37868);
#31851=PLANE('',#37878);
#31852=PLANE('',#37890);
#31853=PLANE('',#37896);
#31854=PLANE('',#37902);
#31855=PLANE('',#37903);
#31856=PLANE('',#37906);
#31857=PLANE('',#37909);
#31858=PLANE('',#37917);
#31859=PLANE('',#37918);
#31860=PLANE('',#37919);
#31861=PLANE('',#37920);
#31862=PLANE('',#37921);
#31863=PLANE('',#37924);
#31864=PLANE('',#37927);
#31865=PLANE('',#37931);
#31866=PLANE('',#37936);
#31867=PLANE('',#37941);
#31868=PLANE('',#37944);
#31869=PLANE('',#37945);
#31870=PLANE('',#37947);
#31871=PLANE('',#37948);
#31872=PLANE('',#37950);
#31873=PLANE('',#37951);
#31874=PLANE('',#37953);
#31875=PLANE('',#37954);
#31876=PLANE('',#37958);
#31877=PLANE('',#37962);
#31878=PLANE('',#37972);
#31879=PLANE('',#37979);
#31880=PLANE('',#37980);
#31881=PLANE('',#37990);
#31882=PLANE('',#38000);
#31883=PLANE('',#38007);
#31884=PLANE('',#38017);
#31885=PLANE('',#38021);
#31886=PLANE('',#38028);
#31887=PLANE('',#38038);
#31888=PLANE('',#38042);
#31889=PLANE('',#38047);
#31890=PLANE('',#38056);
#31891=PLANE('',#38060);
#31892=PLANE('',#38061);
#31893=PLANE('',#38062);
#31894=PLANE('',#38063);
#31895=PLANE('',#38064);
#31896=PLANE('',#38065);
#31897=PLANE('',#38066);
#31898=PLANE('',#38067);
#31899=PLANE('',#38068);
#31900=PLANE('',#38069);
#31901=PLANE('',#38070);
#31902=PLANE('',#38079);
#31903=PLANE('',#38080);
#31904=PLANE('',#38081);
#31905=PLANE('',#38082);
#31906=PLANE('',#38083);
#31907=PLANE('',#38084);
#31908=PLANE('',#38085);
#31909=PLANE('',#38086);
#31910=PLANE('',#38095);
#31911=PLANE('',#38106);
#31912=PLANE('',#38114);
#31913=ADVANCED_FACE('',(#4232),#31112,.F.);
#31914=ADVANCED_FACE('',(#4233),#31113,.F.);
#31915=ADVANCED_FACE('',(#4234),#31114,.F.);
#31916=ADVANCED_FACE('',(#4235,#1878),#31115,.F.);
#31917=ADVANCED_FACE('',(#4236),#1038,.F.);
#31918=ADVANCED_FACE('',(#4237),#31116,.F.);
#31919=ADVANCED_FACE('',(#4238),#1039,.F.);
#31920=ADVANCED_FACE('',(#4239),#31117,.F.);
#31921=ADVANCED_FACE('',(#4240),#31118,.F.);
#31922=ADVANCED_FACE('',(#4241),#31119,.F.);
#31923=ADVANCED_FACE('',(#4242),#1040,.F.);
#31924=ADVANCED_FACE('',(#4243),#31120,.F.);
#31925=ADVANCED_FACE('',(#4244),#31121,.F.);
#31926=ADVANCED_FACE('',(#4245),#1041,.T.);
#31927=ADVANCED_FACE('',(#4246),#1042,.T.);
#31928=ADVANCED_FACE('',(#4247),#1043,.F.);
#31929=ADVANCED_FACE('',(#4248),#31122,.F.);
#31930=ADVANCED_FACE('',(#4249),#31123,.F.);
#31931=ADVANCED_FACE('',(#4250),#31124,.F.);
#31932=ADVANCED_FACE('',(#4251),#1044,.T.);
#31933=ADVANCED_FACE('',(#4252,#1879),#31125,.T.);
#31934=ADVANCED_FACE('',(#4253,#1880,#1881,#1882,#1883,#1884),#31126,.F.);
#31935=ADVANCED_FACE('',(#4254),#1045,.T.);
#31936=ADVANCED_FACE('',(#4255),#874,.T.);
#31937=ADVANCED_FACE('',(#4256),#1046,.T.);
#31938=ADVANCED_FACE('',(#4257,#1885),#31127,.T.);
#31939=ADVANCED_FACE('',(#4258,#1886),#31128,.T.);
#31940=ADVANCED_FACE('',(#4259,#1887),#31129,.T.);
#31941=ADVANCED_FACE('',(#4260,#1888),#31130,.T.);
#31942=ADVANCED_FACE('',(#4261),#1047,.F.);
#31943=ADVANCED_FACE('',(#4262),#1048,.F.);
#31944=ADVANCED_FACE('',(#4263),#1049,.F.);
#31945=ADVANCED_FACE('',(#4264),#1050,.F.);
#31946=ADVANCED_FACE('',(#4265),#875,.F.);
#31947=ADVANCED_FACE('',(#4266),#854,.F.);
#31948=ADVANCED_FACE('',(#4267),#1051,.T.);
#31949=ADVANCED_FACE('',(#4268),#876,.F.);
#31950=ADVANCED_FACE('',(#4269),#31131,.T.);
#31951=ADVANCED_FACE('',(#4270),#31132,.T.);
#31952=ADVANCED_FACE('',(#4271),#31133,.T.);
#31953=ADVANCED_FACE('',(#4272),#31134,.T.);
#31954=ADVANCED_FACE('',(#4273),#1052,.F.);
#31955=ADVANCED_FACE('',(#4274),#710,.F.);
#31956=ADVANCED_FACE('',(#4275),#1053,.T.);
#31957=ADVANCED_FACE('',(#4276),#711,.T.);
#31958=ADVANCED_FACE('',(#4277),#1054,.T.);
#31959=ADVANCED_FACE('',(#4278),#877,.T.);
#31960=ADVANCED_FACE('',(#4279),#1055,.T.);
#31961=ADVANCED_FACE('',(#4280),#31135,.T.);
#31962=ADVANCED_FACE('',(#4281),#1056,.T.);
#31963=ADVANCED_FACE('',(#4282),#878,.T.);
#31964=ADVANCED_FACE('',(#4283),#1057,.T.);
#31965=ADVANCED_FACE('',(#4284),#31136,.T.);
#31966=ADVANCED_FACE('',(#4285),#855,.T.);
#31967=ADVANCED_FACE('',(#4286),#1058,.F.);
#31968=ADVANCED_FACE('',(#4287),#712,.F.);
#31969=ADVANCED_FACE('',(#4288),#856,.F.);
#31970=ADVANCED_FACE('',(#4289),#1059,.T.);
#31971=ADVANCED_FACE('',(#4290),#713,.T.);
#31972=ADVANCED_FACE('',(#4291),#1060,.T.);
#31973=ADVANCED_FACE('',(#4292),#879,.F.);
#31974=ADVANCED_FACE('',(#4293),#857,.F.);
#31975=ADVANCED_FACE('',(#4294),#1061,.T.);
#31976=ADVANCED_FACE('',(#4295),#714,.T.);
#31977=ADVANCED_FACE('',(#4296),#858,.T.);
#31978=ADVANCED_FACE('',(#4297),#1062,.T.);
#31979=ADVANCED_FACE('',(#4298),#859,.T.);
#31980=ADVANCED_FACE('',(#4299),#1063,.F.);
#31981=ADVANCED_FACE('',(#4300),#715,.F.);
#31982=ADVANCED_FACE('',(#4301),#860,.F.);
#31983=ADVANCED_FACE('',(#4302),#1064,.T.);
#31984=ADVANCED_FACE('',(#4303),#716,.T.);
#31985=ADVANCED_FACE('',(#4304),#1065,.T.);
#31986=ADVANCED_FACE('',(#4305),#880,.F.);
#31987=ADVANCED_FACE('',(#4306),#717,.F.);
#31988=ADVANCED_FACE('',(#4307),#1066,.F.);
#31989=ADVANCED_FACE('',(#4308),#881,.F.);
#31990=ADVANCED_FACE('',(#4309),#861,.F.);
#31991=ADVANCED_FACE('',(#4310),#1067,.T.);
#31992=ADVANCED_FACE('',(#4311),#1068,.F.);
#31993=ADVANCED_FACE('',(#4312),#718,.F.);
#31994=ADVANCED_FACE('',(#4313),#862,.T.);
#31995=ADVANCED_FACE('',(#4314),#1069,.T.);
#31996=ADVANCED_FACE('',(#4315),#31137,.T.);
#31997=ADVANCED_FACE('',(#4316),#1070,.T.);
#31998=ADVANCED_FACE('',(#4317),#882,.T.);
#31999=ADVANCED_FACE('',(#4318),#1071,.T.);
#32000=ADVANCED_FACE('',(#4319),#31138,.T.);
#32001=ADVANCED_FACE('',(#4320),#1072,.T.);
#32002=ADVANCED_FACE('',(#4321),#719,.T.);
#32003=ADVANCED_FACE('',(#4322),#1073,.T.);
#32004=ADVANCED_FACE('',(#4323),#863,.F.);
#32005=ADVANCED_FACE('',(#4324),#883,.F.);
#32006=ADVANCED_FACE('',(#4325),#864,.F.);
#32007=ADVANCED_FACE('',(#4326),#1074,.T.);
#32008=ADVANCED_FACE('',(#4327),#720,.T.);
#32009=ADVANCED_FACE('',(#4328),#865,.T.);
#32010=ADVANCED_FACE('',(#4329),#1075,.T.);
#32011=ADVANCED_FACE('',(#4330),#1076,.F.);
#32012=ADVANCED_FACE('',(#4331),#721,.F.);
#32013=ADVANCED_FACE('',(#4332),#722,.F.);
#32014=ADVANCED_FACE('',(#4333),#1077,.F.);
#32015=ADVANCED_FACE('',(#4334),#866,.T.);
#32016=ADVANCED_FACE('',(#4335),#1078,.T.);
#32017=ADVANCED_FACE('',(#4336),#867,.T.);
#32018=ADVANCED_FACE('',(#4337),#1079,.F.);
#32019=ADVANCED_FACE('',(#4338),#723,.F.);
#32020=ADVANCED_FACE('',(#4339),#884,.F.);
#32021=ADVANCED_FACE('',(#4340),#868,.F.);
#32022=ADVANCED_FACE('',(#4341),#885,.F.);
#32023=ADVANCED_FACE('',(#4342),#1080,.T.);
#32024=ADVANCED_FACE('',(#4343),#724,.T.);
#32025=ADVANCED_FACE('',(#4344),#1081,.T.);
#32026=ADVANCED_FACE('',(#4345),#725,.T.);
#32027=ADVANCED_FACE('',(#4346),#869,.T.);
#32028=ADVANCED_FACE('',(#4347),#886,.T.);
#32029=ADVANCED_FACE('',(#4348,#1889),#31139,.T.);
#32030=ADVANCED_FACE('',(#4349),#887,.T.);
#32031=ADVANCED_FACE('',(#4350),#1082,.T.);
#32032=ADVANCED_FACE('',(#4351,#1890),#31140,.T.);
#32033=ADVANCED_FACE('',(#4352),#1083,.F.);
#32034=ADVANCED_FACE('',(#4353,#1891),#31141,.T.);
#32035=ADVANCED_FACE('',(#4354),#1084,.T.);
#32036=ADVANCED_FACE('',(#4355,#1892),#31142,.T.);
#32037=ADVANCED_FACE('',(#4356),#1085,.F.);
#32038=ADVANCED_FACE('',(#4357,#1893),#31143,.F.);
#32039=ADVANCED_FACE('',(#4358),#1086,.T.);
#32040=ADVANCED_FACE('',(#4359,#1894),#31144,.F.);
#32041=ADVANCED_FACE('',(#4360),#1087,.F.);
#32042=ADVANCED_FACE('',(#4361,#1895),#31145,.F.);
#32043=ADVANCED_FACE('',(#4362),#1088,.F.);
#32044=ADVANCED_FACE('',(#4363,#1896),#31146,.T.);
#32045=ADVANCED_FACE('',(#4364),#1089,.T.);
#32046=ADVANCED_FACE('',(#4365),#31147,.F.);
#32047=ADVANCED_FACE('',(#4366),#1090,.T.);
#32048=ADVANCED_FACE('',(#4367),#31148,.F.);
#32049=ADVANCED_FACE('',(#4368),#1091,.T.);
#32050=ADVANCED_FACE('',(#4369),#31149,.F.);
#32051=ADVANCED_FACE('',(#4370),#1092,.T.);
#32052=ADVANCED_FACE('',(#4371),#31150,.F.);
#32053=ADVANCED_FACE('',(#4372),#888,.F.);
#32054=ADVANCED_FACE('',(#4373),#1093,.T.);
#32055=ADVANCED_FACE('',(#4374,#1897),#31151,.T.);
#32056=ADVANCED_FACE('',(#4375),#565,.T.);
#32057=ADVANCED_FACE('',(#4376),#31152,.T.);
#32058=ADVANCED_FACE('',(#4377),#889,.T.);
#32059=ADVANCED_FACE('',(#4378,#1898),#31153,.T.);
#32060=ADVANCED_FACE('',(#4379),#1094,.T.);
#32061=ADVANCED_FACE('',(#4380),#31154,.F.);
#32062=ADVANCED_FACE('',(#4381),#31155,.F.);
#32063=ADVANCED_FACE('',(#4382),#31156,.F.);
#32064=ADVANCED_FACE('',(#4383),#31157,.F.);
#32065=ADVANCED_FACE('',(#4384),#31158,.F.);
#32066=ADVANCED_FACE('',(#4385),#31159,.F.);
#32067=ADVANCED_FACE('',(#4386),#566,.F.);
#32068=ADVANCED_FACE('',(#4387),#890,.F.);
#32069=ADVANCED_FACE('',(#4388),#1095,.T.);
#32070=ADVANCED_FACE('',(#4389,#1899),#31160,.T.);
#32071=ADVANCED_FACE('',(#4390),#567,.T.);
#32072=ADVANCED_FACE('',(#4391),#31161,.T.);
#32073=ADVANCED_FACE('',(#4392),#891,.T.);
#32074=ADVANCED_FACE('',(#4393,#1900),#31162,.T.);
#32075=ADVANCED_FACE('',(#4394),#1096,.T.);
#32076=ADVANCED_FACE('',(#4395),#31163,.F.);
#32077=ADVANCED_FACE('',(#4396),#31164,.F.);
#32078=ADVANCED_FACE('',(#4397),#31165,.F.);
#32079=ADVANCED_FACE('',(#4398),#31166,.F.);
#32080=ADVANCED_FACE('',(#4399),#31167,.F.);
#32081=ADVANCED_FACE('',(#4400),#31168,.F.);
#32082=ADVANCED_FACE('',(#4401),#568,.F.);
#32083=ADVANCED_FACE('',(#4402),#892,.F.);
#32084=ADVANCED_FACE('',(#4403),#1097,.T.);
#32085=ADVANCED_FACE('',(#4404,#1901),#31169,.T.);
#32086=ADVANCED_FACE('',(#4405),#569,.T.);
#32087=ADVANCED_FACE('',(#4406),#31170,.T.);
#32088=ADVANCED_FACE('',(#4407),#893,.T.);
#32089=ADVANCED_FACE('',(#4408,#1902),#31171,.T.);
#32090=ADVANCED_FACE('',(#4409),#1098,.T.);
#32091=ADVANCED_FACE('',(#4410),#31172,.F.);
#32092=ADVANCED_FACE('',(#4411),#31173,.F.);
#32093=ADVANCED_FACE('',(#4412),#31174,.F.);
#32094=ADVANCED_FACE('',(#4413),#31175,.F.);
#32095=ADVANCED_FACE('',(#4414),#31176,.F.);
#32096=ADVANCED_FACE('',(#4415),#31177,.F.);
#32097=ADVANCED_FACE('',(#4416),#570,.F.);
#32098=ADVANCED_FACE('',(#4417),#894,.F.);
#32099=ADVANCED_FACE('',(#4418),#1099,.T.);
#32100=ADVANCED_FACE('',(#4419,#1903),#31178,.T.);
#32101=ADVANCED_FACE('',(#4420),#571,.T.);
#32102=ADVANCED_FACE('',(#4421),#31179,.T.);
#32103=ADVANCED_FACE('',(#4422),#572,.T.);
#32104=ADVANCED_FACE('',(#4423),#573,.T.);
#32105=ADVANCED_FACE('',(#4424),#574,.T.);
#32106=ADVANCED_FACE('',(#4425),#575,.T.);
#32107=ADVANCED_FACE('',(#4426),#576,.T.);
#32108=ADVANCED_FACE('',(#4427),#577,.T.);
#32109=ADVANCED_FACE('',(#4428),#31180,.T.);
#32110=ADVANCED_FACE('',(#4429),#31181,.T.);
#32111=ADVANCED_FACE('',(#4430),#31182,.T.);
#32112=ADVANCED_FACE('',(#4431,#1904),#31183,.T.);
#32113=ADVANCED_FACE('',(#4432),#31184,.T.);
#32114=ADVANCED_FACE('',(#4433),#31185,.T.);
#32115=ADVANCED_FACE('',(#4434),#31186,.T.);
#32116=ADVANCED_FACE('',(#4435),#31187,.F.);
#32117=ADVANCED_FACE('',(#4436),#1100,.T.);
#32118=ADVANCED_FACE('',(#4437),#31188,.F.);
#32119=ADVANCED_FACE('',(#4438),#31189,.F.);
#32120=ADVANCED_FACE('',(#4439),#31190,.F.);
#32121=ADVANCED_FACE('',(#4440),#31191,.F.);
#32122=ADVANCED_FACE('',(#4441),#31192,.F.);
#32123=ADVANCED_FACE('',(#4442),#31193,.F.);
#32124=ADVANCED_FACE('',(#4443),#31194,.F.);
#32125=ADVANCED_FACE('',(#4444),#31195,.F.);
#32126=ADVANCED_FACE('',(#4445,#1905),#31196,.T.);
#32127=ADVANCED_FACE('',(#4446),#31197,.T.);
#32128=ADVANCED_FACE('',(#4447),#31198,.T.);
#32129=ADVANCED_FACE('',(#4448),#31199,.T.);
#32130=ADVANCED_FACE('',(#4449),#31200,.T.);
#32131=ADVANCED_FACE('',(#4450,#1906),#31201,.T.);
#32132=ADVANCED_FACE('',(#4451,#1907),#31202,.F.);
#32133=ADVANCED_FACE('',(#4452),#1101,.F.);
#32134=ADVANCED_FACE('',(#4453),#1102,.F.);
#32135=ADVANCED_FACE('',(#4454),#1103,.F.);
#32136=ADVANCED_FACE('',(#4455),#1104,.F.);
#32137=ADVANCED_FACE('',(#4456),#1105,.F.);
#32138=ADVANCED_FACE('',(#4457),#1106,.F.);
#32139=ADVANCED_FACE('',(#4458,#1908,#1909,#1910,#1911,#1912,#1913,#1914),
#31203,.T.);
#32140=ADVANCED_FACE('',(#4459),#31204,.T.);
#32141=ADVANCED_FACE('',(#4460),#31205,.T.);
#32142=ADVANCED_FACE('',(#4461),#31206,.T.);
#32143=ADVANCED_FACE('',(#4462),#31207,.T.);
#32144=ADVANCED_FACE('',(#4463),#31208,.T.);
#32145=ADVANCED_FACE('',(#4464),#31209,.T.);
#32146=ADVANCED_FACE('',(#4465),#31210,.F.);
#32147=ADVANCED_FACE('',(#4466),#31211,.F.);
#32148=ADVANCED_FACE('',(#4467),#31212,.F.);
#32149=ADVANCED_FACE('',(#4468),#31213,.F.);
#32150=ADVANCED_FACE('',(#4469),#31214,.F.);
#32151=ADVANCED_FACE('',(#4470),#31215,.F.);
#32152=ADVANCED_FACE('',(#4471),#31216,.F.);
#32153=ADVANCED_FACE('',(#4472),#31217,.T.);
#32154=ADVANCED_FACE('',(#4473,#1915,#1916,#1917,#1918,#1919,#1920,#1921),
#31218,.T.);
#32155=ADVANCED_FACE('',(#4474),#31219,.T.);
#32156=ADVANCED_FACE('',(#4475),#31220,.T.);
#32157=ADVANCED_FACE('',(#4476,#1922),#31221,.T.);
#32158=ADVANCED_FACE('',(#4477),#31222,.T.);
#32159=ADVANCED_FACE('',(#4478),#31223,.F.);
#32160=ADVANCED_FACE('',(#4479),#870,.F.);
#32161=ADVANCED_FACE('',(#4480),#31224,.T.);
#32162=ADVANCED_FACE('',(#4481),#31225,.T.);
#32163=ADVANCED_FACE('',(#4482),#31226,.T.);
#32164=ADVANCED_FACE('',(#4483),#31227,.T.);
#32165=ADVANCED_FACE('',(#4484),#1107,.T.);
#32166=ADVANCED_FACE('',(#4485,#1923,#1924),#1108,.T.);
#32167=ADVANCED_FACE('',(#4486),#1109,.F.);
#32168=ADVANCED_FACE('',(#4487),#1110,.F.);
#32169=ADVANCED_FACE('',(#4488),#1111,.T.);
#32170=ADVANCED_FACE('',(#4489),#31228,.T.);
#32171=ADVANCED_FACE('',(#4490),#31229,.T.);
#32172=ADVANCED_FACE('',(#4491),#1112,.T.);
#32173=ADVANCED_FACE('',(#4492,#1925,#1926),#1113,.T.);
#32174=ADVANCED_FACE('',(#4493),#31230,.T.);
#32175=ADVANCED_FACE('',(#4494,#1927),#726,.T.);
#32176=ADVANCED_FACE('',(#4495),#31231,.T.);
#32177=ADVANCED_FACE('',(#4496),#31232,.T.);
#32178=ADVANCED_FACE('',(#4497),#31233,.T.);
#32179=ADVANCED_FACE('',(#4498),#1114,.T.);
#32180=ADVANCED_FACE('',(#4499),#1115,.T.);
#32181=ADVANCED_FACE('',(#4500),#31234,.T.);
#32182=ADVANCED_FACE('',(#4501),#31235,.T.);
#32183=ADVANCED_FACE('',(#4502),#31236,.T.);
#32184=ADVANCED_FACE('',(#4503),#31237,.T.);
#32185=ADVANCED_FACE('',(#4504),#31238,.T.);
#32186=ADVANCED_FACE('',(#4505),#31239,.T.);
#32187=ADVANCED_FACE('',(#4506),#31240,.T.);
#32188=ADVANCED_FACE('',(#4507),#31241,.T.);
#32189=ADVANCED_FACE('',(#4508),#31242,.T.);
#32190=ADVANCED_FACE('',(#4509),#31243,.T.);
#32191=ADVANCED_FACE('',(#4510),#31244,.T.);
#32192=ADVANCED_FACE('',(#4511),#31245,.T.);
#32193=ADVANCED_FACE('',(#4512),#31246,.T.);
#32194=ADVANCED_FACE('',(#4513,#1928),#727,.T.);
#32195=ADVANCED_FACE('',(#4514),#31247,.T.);
#32196=ADVANCED_FACE('',(#4515),#1116,.T.);
#32197=ADVANCED_FACE('',(#4516),#1117,.T.);
#32198=ADVANCED_FACE('',(#4517),#31248,.T.);
#32199=ADVANCED_FACE('',(#4518),#1118,.T.);
#32200=ADVANCED_FACE('',(#4519),#31249,.T.);
#32201=ADVANCED_FACE('',(#4520),#1119,.T.);
#32202=ADVANCED_FACE('',(#4521),#31250,.T.);
#32203=ADVANCED_FACE('',(#4522),#1120,.T.);
#32204=ADVANCED_FACE('',(#4523),#31251,.T.);
#32205=ADVANCED_FACE('',(#4524,#1929),#31252,.T.);
#32206=ADVANCED_FACE('',(#4525,#1930,#1931,#1932),#31253,.T.);
#32207=ADVANCED_FACE('',(#4526),#1121,.T.);
#32208=ADVANCED_FACE('',(#4527),#31254,.T.);
#32209=ADVANCED_FACE('',(#4528),#1122,.T.);
#32210=ADVANCED_FACE('',(#4529),#31255,.T.);
#32211=ADVANCED_FACE('',(#4530),#1123,.T.);
#32212=ADVANCED_FACE('',(#4531),#31256,.T.);
#32213=ADVANCED_FACE('',(#4532),#1124,.T.);
#32214=ADVANCED_FACE('',(#4533),#31257,.T.);
#32215=ADVANCED_FACE('',(#4534),#31258,.T.);
#32216=ADVANCED_FACE('',(#4535,#1933),#728,.T.);
#32217=ADVANCED_FACE('',(#4536),#1125,.T.);
#32218=ADVANCED_FACE('',(#4537,#1934),#729,.T.);
#32219=ADVANCED_FACE('',(#4538),#1126,.T.);
#32220=ADVANCED_FACE('',(#4539),#31259,.T.);
#32221=ADVANCED_FACE('',(#4540),#31260,.T.);
#32222=ADVANCED_FACE('',(#4541),#31261,.T.);
#32223=ADVANCED_FACE('',(#4542),#31262,.T.);
#32224=ADVANCED_FACE('',(#4543),#31263,.T.);
#32225=ADVANCED_FACE('',(#4544),#31264,.T.);
#32226=ADVANCED_FACE('',(#4545),#31265,.T.);
#32227=ADVANCED_FACE('',(#4546),#31266,.T.);
#32228=ADVANCED_FACE('',(#4547),#31267,.T.);
#32229=ADVANCED_FACE('',(#4548),#31268,.T.);
#32230=ADVANCED_FACE('',(#4549),#31269,.T.);
#32231=ADVANCED_FACE('',(#4550),#31270,.T.);
#32232=ADVANCED_FACE('',(#4551),#31271,.T.);
#32233=ADVANCED_FACE('',(#4552),#31272,.T.);
#32234=ADVANCED_FACE('',(#4553),#31273,.T.);
#32235=ADVANCED_FACE('',(#4554),#31274,.T.);
#32236=ADVANCED_FACE('',(#4555),#31275,.T.);
#32237=ADVANCED_FACE('',(#4556),#31276,.T.);
#32238=ADVANCED_FACE('',(#4557),#31277,.T.);
#32239=ADVANCED_FACE('',(#4558),#31278,.T.);
#32240=ADVANCED_FACE('',(#4559),#31279,.T.);
#32241=ADVANCED_FACE('',(#4560),#31280,.T.);
#32242=ADVANCED_FACE('',(#4561),#31281,.T.);
#32243=ADVANCED_FACE('',(#4562),#31282,.T.);
#32244=ADVANCED_FACE('',(#4563),#31283,.T.);
#32245=ADVANCED_FACE('',(#4564),#31284,.T.);
#32246=ADVANCED_FACE('',(#4565),#31285,.T.);
#32247=ADVANCED_FACE('',(#4566),#31286,.T.);
#32248=ADVANCED_FACE('',(#4567),#31287,.T.);
#32249=ADVANCED_FACE('',(#4568),#31288,.T.);
#32250=ADVANCED_FACE('',(#4569),#31289,.T.);
#32251=ADVANCED_FACE('',(#4570),#31290,.T.);
#32252=ADVANCED_FACE('',(#4571),#31291,.T.);
#32253=ADVANCED_FACE('',(#4572),#31292,.T.);
#32254=ADVANCED_FACE('',(#4573),#31293,.T.);
#32255=ADVANCED_FACE('',(#4574),#31294,.T.);
#32256=ADVANCED_FACE('',(#4575),#1127,.T.);
#32257=ADVANCED_FACE('',(#4576),#31295,.T.);
#32258=ADVANCED_FACE('',(#4577),#31296,.T.);
#32259=ADVANCED_FACE('',(#4578),#31297,.T.);
#32260=ADVANCED_FACE('',(#4579),#1128,.T.);
#32261=ADVANCED_FACE('',(#4580),#31298,.T.);
#32262=ADVANCED_FACE('',(#4581),#31299,.T.);
#32263=ADVANCED_FACE('',(#4582),#31300,.T.);
#32264=ADVANCED_FACE('',(#4583),#31301,.T.);
#32265=ADVANCED_FACE('',(#4584),#31302,.T.);
#32266=ADVANCED_FACE('',(#4585,#1935),#31303,.T.);
#32267=ADVANCED_FACE('',(#4586),#31304,.T.);
#32268=ADVANCED_FACE('',(#4587),#31305,.T.);
#32269=ADVANCED_FACE('',(#4588),#31306,.T.);
#32270=ADVANCED_FACE('',(#4589),#31307,.T.);
#32271=ADVANCED_FACE('',(#4590),#31308,.T.);
#32272=ADVANCED_FACE('',(#4591),#31309,.T.);
#32273=ADVANCED_FACE('',(#4592),#31310,.T.);
#32274=ADVANCED_FACE('',(#4593),#31311,.T.);
#32275=ADVANCED_FACE('',(#4594),#31312,.T.);
#32276=ADVANCED_FACE('',(#4595),#31313,.T.);
#32277=ADVANCED_FACE('',(#4596),#31314,.T.);
#32278=ADVANCED_FACE('',(#4597),#31315,.T.);
#32279=ADVANCED_FACE('',(#4598),#1129,.F.);
#32280=ADVANCED_FACE('',(#4599),#31316,.T.);
#32281=ADVANCED_FACE('',(#4600),#31317,.T.);
#32282=ADVANCED_FACE('',(#4601),#31318,.T.);
#32283=ADVANCED_FACE('',(#4602,#1936),#730,.T.);
#32284=ADVANCED_FACE('',(#4603),#31319,.T.);
#32285=ADVANCED_FACE('',(#4604),#31320,.T.);
#32286=ADVANCED_FACE('',(#4605),#31321,.T.);
#32287=ADVANCED_FACE('',(#4606),#31322,.T.);
#32288=ADVANCED_FACE('',(#4607),#31323,.T.);
#32289=ADVANCED_FACE('',(#4608),#31324,.T.);
#32290=ADVANCED_FACE('',(#4609),#31325,.T.);
#32291=ADVANCED_FACE('',(#4610),#31326,.T.);
#32292=ADVANCED_FACE('',(#4611),#31327,.T.);
#32293=ADVANCED_FACE('',(#4612),#31328,.T.);
#32294=ADVANCED_FACE('',(#4613),#31329,.T.);
#32295=ADVANCED_FACE('',(#4614,#1937),#31330,.T.);
#32296=ADVANCED_FACE('',(#4615),#1130,.T.);
#32297=ADVANCED_FACE('',(#4616),#31331,.T.);
#32298=ADVANCED_FACE('',(#4617),#1131,.T.);
#32299=ADVANCED_FACE('',(#4618),#31332,.T.);
#32300=ADVANCED_FACE('',(#4619),#1132,.T.);
#32301=ADVANCED_FACE('',(#4620),#871,.F.);
#32302=ADVANCED_FACE('',(#4621),#31333,.T.);
#32303=ADVANCED_FACE('',(#4622),#872,.F.);
#32304=ADVANCED_FACE('',(#4623),#873,.F.);
#32305=ADVANCED_FACE('',(#4624),#895,.T.);
#32306=ADVANCED_FACE('',(#4625,#1938,#1939,#1940),#1133,.T.);
#32307=ADVANCED_FACE('',(#4626),#31334,.T.);
#32308=ADVANCED_FACE('',(#4627),#31335,.T.);
#32309=ADVANCED_FACE('',(#4628,#1941),#1134,.T.);
#32310=ADVANCED_FACE('',(#4629),#31336,.T.);
#32311=ADVANCED_FACE('',(#4630),#31337,.T.);
#32312=ADVANCED_FACE('',(#4631),#31338,.T.);
#32313=ADVANCED_FACE('',(#4632),#31339,.T.);
#32314=ADVANCED_FACE('',(#4633),#31340,.T.);
#32315=ADVANCED_FACE('',(#4634,#1942),#31341,.T.);
#32316=ADVANCED_FACE('',(#4635),#1135,.T.);
#32317=ADVANCED_FACE('',(#4636),#31342,.T.);
#32318=ADVANCED_FACE('',(#4637),#1136,.T.);
#32319=ADVANCED_FACE('',(#4638),#31343,.T.);
#32320=ADVANCED_FACE('',(#4639,#1943),#31344,.T.);
#32321=ADVANCED_FACE('',(#4640),#1137,.T.);
#32322=ADVANCED_FACE('',(#4641),#31345,.T.);
#32323=ADVANCED_FACE('',(#4642),#1138,.T.);
#32324=ADVANCED_FACE('',(#4643),#31346,.T.);
#32325=ADVANCED_FACE('',(#4644),#31347,.T.);
#32326=ADVANCED_FACE('',(#4645),#1139,.F.);
#32327=ADVANCED_FACE('',(#4646),#578,.F.);
#32328=ADVANCED_FACE('',(#4647),#31348,.T.);
#32329=ADVANCED_FACE('',(#4648),#1140,.F.);
#32330=ADVANCED_FACE('',(#4649),#579,.F.);
#32331=ADVANCED_FACE('',(#4650),#31349,.T.);
#32332=ADVANCED_FACE('',(#4651),#1141,.F.);
#32333=ADVANCED_FACE('',(#4652),#580,.F.);
#32334=ADVANCED_FACE('',(#4653),#31350,.T.);
#32335=ADVANCED_FACE('',(#4654),#1142,.F.);
#32336=ADVANCED_FACE('',(#4655),#581,.F.);
#32337=ADVANCED_FACE('',(#4656),#582,.T.);
#32338=ADVANCED_FACE('',(#4657,#1944,#1945,#1946,#1947,#1948,#1949,#1950,
#1951,#1952),#31351,.T.);
#32339=ADVANCED_FACE('',(#4658),#1143,.T.);
#32340=ADVANCED_FACE('',(#4659,#1953),#31352,.T.);
#32341=ADVANCED_FACE('',(#4660),#1144,.F.);
#32342=ADVANCED_FACE('',(#4661,#1954,#1955,#1956),#31353,.T.);
#32343=ADVANCED_FACE('',(#4662),#1145,.T.);
#32344=ADVANCED_FACE('',(#4663,#1957),#31354,.T.);
#32345=ADVANCED_FACE('',(#4664),#1146,.F.);
#32346=ADVANCED_FACE('',(#4665,#1958),#31355,.T.);
#32347=ADVANCED_FACE('',(#4666),#1147,.F.);
#32348=ADVANCED_FACE('',(#4667),#1148,.F.);
#32349=ADVANCED_FACE('',(#4668),#31356,.T.);
#32350=ADVANCED_FACE('',(#4669),#1149,.F.);
#32351=ADVANCED_FACE('',(#4670,#1959),#31357,.T.);
#32352=ADVANCED_FACE('',(#4671),#1150,.F.);
#32353=ADVANCED_FACE('',(#4672),#31358,.T.);
#32354=ADVANCED_FACE('',(#4673),#31359,.T.);
#32355=ADVANCED_FACE('',(#4674),#1151,.F.);
#32356=ADVANCED_FACE('',(#4675,#1960),#31360,.T.);
#32357=ADVANCED_FACE('',(#4676),#1152,.F.);
#32358=ADVANCED_FACE('',(#4677),#1153,.F.);
#32359=ADVANCED_FACE('',(#4678,#1961),#31361,.T.);
#32360=ADVANCED_FACE('',(#4679),#1154,.F.);
#32361=ADVANCED_FACE('',(#4680),#31362,.T.);
#32362=ADVANCED_FACE('',(#4681),#31363,.T.);
#32363=ADVANCED_FACE('',(#4682),#1155,.F.);
#32364=ADVANCED_FACE('',(#4683),#31364,.T.);
#32365=ADVANCED_FACE('',(#4684,#1962),#31365,.T.);
#32366=ADVANCED_FACE('',(#4685),#1156,.F.);
#32367=ADVANCED_FACE('',(#4686),#1157,.F.);
#32368=ADVANCED_FACE('',(#4687),#1158,.F.);
#32369=ADVANCED_FACE('',(#4688,#1963),#31366,.T.);
#32370=ADVANCED_FACE('',(#4689),#1159,.T.);
#32371=ADVANCED_FACE('',(#4690),#1160,.T.);
#32372=ADVANCED_FACE('',(#4691,#1964),#31367,.T.);
#32373=ADVANCED_FACE('',(#4692,#1965),#731,.T.);
#32374=ADVANCED_FACE('',(#4693,#1966),#31368,.T.);
#32375=ADVANCED_FACE('',(#4694),#1161,.T.);
#32376=ADVANCED_FACE('',(#4695),#1162,.T.);
#32377=ADVANCED_FACE('',(#4696,#1967),#732,.T.);
#32378=ADVANCED_FACE('',(#4697),#31369,.T.);
#32379=ADVANCED_FACE('',(#4698),#31370,.T.);
#32380=ADVANCED_FACE('',(#4699),#31371,.T.);
#32381=ADVANCED_FACE('',(#4700),#31372,.T.);
#32382=ADVANCED_FACE('',(#4701),#31373,.T.);
#32383=ADVANCED_FACE('',(#4702),#31374,.T.);
#32384=ADVANCED_FACE('',(#4703),#31375,.T.);
#32385=ADVANCED_FACE('',(#4704),#31376,.T.);
#32386=ADVANCED_FACE('',(#4705),#31377,.T.);
#32387=ADVANCED_FACE('',(#4706),#31378,.T.);
#32388=ADVANCED_FACE('',(#4707),#31379,.T.);
#32389=ADVANCED_FACE('',(#4708),#31380,.T.);
#32390=ADVANCED_FACE('',(#4709),#31381,.T.);
#32391=ADVANCED_FACE('',(#4710),#31382,.T.);
#32392=ADVANCED_FACE('',(#4711),#31383,.T.);
#32393=ADVANCED_FACE('',(#4712),#31384,.T.);
#32394=ADVANCED_FACE('',(#4713),#31385,.T.);
#32395=ADVANCED_FACE('',(#4714),#31386,.T.);
#32396=ADVANCED_FACE('',(#4715),#31387,.T.);
#32397=ADVANCED_FACE('',(#4716),#31388,.T.);
#32398=ADVANCED_FACE('',(#4717),#31389,.T.);
#32399=ADVANCED_FACE('',(#4718),#31390,.T.);
#32400=ADVANCED_FACE('',(#4719),#31391,.T.);
#32401=ADVANCED_FACE('',(#4720),#31392,.T.);
#32402=ADVANCED_FACE('',(#4721),#31393,.T.);
#32403=ADVANCED_FACE('',(#4722),#31394,.T.);
#32404=ADVANCED_FACE('',(#4723),#31395,.T.);
#32405=ADVANCED_FACE('',(#4724),#31396,.T.);
#32406=ADVANCED_FACE('',(#4725),#31397,.T.);
#32407=ADVANCED_FACE('',(#4726),#31398,.T.);
#32408=ADVANCED_FACE('',(#4727),#31399,.T.);
#32409=ADVANCED_FACE('',(#4728),#1163,.T.);
#32410=ADVANCED_FACE('',(#4729,#1968,#1969,#1970,#1971,#1972),#31400,.T.);
#32411=ADVANCED_FACE('',(#4730),#1164,.T.);
#32412=ADVANCED_FACE('',(#4731),#31401,.T.);
#32413=ADVANCED_FACE('',(#4732),#1165,.F.);
#32414=ADVANCED_FACE('',(#4733),#474,.T.);
#32415=ADVANCED_FACE('',(#4734),#475,.T.);
#32416=ADVANCED_FACE('',(#4735),#31402,.T.);
#32417=ADVANCED_FACE('',(#4736),#31403,.T.);
#32418=ADVANCED_FACE('',(#4737),#31404,.T.);
#32419=ADVANCED_FACE('',(#4738),#1166,.T.);
#32420=ADVANCED_FACE('',(#4739),#733,.T.);
#32421=ADVANCED_FACE('',(#4740),#734,.T.);
#32422=ADVANCED_FACE('',(#4741),#735,.T.);
#32423=ADVANCED_FACE('',(#4742),#736,.T.);
#32424=ADVANCED_FACE('',(#4743),#737,.T.);
#32425=ADVANCED_FACE('',(#4744),#738,.T.);
#32426=ADVANCED_FACE('',(#4745),#896,.T.);
#32427=ADVANCED_FACE('',(#4746),#897,.T.);
#32428=ADVANCED_FACE('',(#4747),#739,.T.);
#32429=ADVANCED_FACE('',(#4748),#740,.T.);
#32430=ADVANCED_FACE('',(#4749),#1167,.T.);
#32431=ADVANCED_FACE('',(#4750),#1168,.T.);
#32432=ADVANCED_FACE('',(#4751),#741,.T.);
#32433=ADVANCED_FACE('',(#4752),#1169,.T.);
#32434=ADVANCED_FACE('',(#4753),#1170,.T.);
#32435=ADVANCED_FACE('',(#4754),#742,.T.);
#32436=ADVANCED_FACE('',(#4755),#1171,.T.);
#32437=ADVANCED_FACE('',(#4756),#1172,.T.);
#32438=ADVANCED_FACE('',(#4757),#1173,.T.);
#32439=ADVANCED_FACE('',(#4758),#1174,.T.);
#32440=ADVANCED_FACE('',(#4759),#1175,.T.);
#32441=ADVANCED_FACE('',(#4760),#1176,.F.);
#32442=ADVANCED_FACE('',(#4761),#1177,.T.);
#32443=ADVANCED_FACE('',(#4762),#1178,.T.);
#32444=ADVANCED_FACE('',(#4763),#1179,.T.);
#32445=ADVANCED_FACE('',(#4764),#1180,.T.);
#32446=ADVANCED_FACE('',(#4765),#1181,.T.);
#32447=ADVANCED_FACE('',(#4766),#1182,.T.);
#32448=ADVANCED_FACE('',(#4767),#1183,.T.);
#32449=ADVANCED_FACE('',(#4768),#1184,.T.);
#32450=ADVANCED_FACE('',(#4769),#1185,.T.);
#32451=ADVANCED_FACE('',(#4770),#1186,.T.);
#32452=ADVANCED_FACE('',(#4771),#31405,.T.);
#32453=ADVANCED_FACE('',(#4772),#31406,.T.);
#32454=ADVANCED_FACE('',(#4773),#31407,.T.);
#32455=ADVANCED_FACE('',(#4774,#1973,#1974,#1975,#1976,#1977),#31408,.T.);
#32456=ADVANCED_FACE('',(#4775),#31409,.T.);
#32457=ADVANCED_FACE('',(#4776),#31410,.T.);
#32458=ADVANCED_FACE('',(#4777),#31411,.T.);
#32459=ADVANCED_FACE('',(#4778),#31412,.T.);
#32460=ADVANCED_FACE('',(#4779),#583,.F.);
#32461=ADVANCED_FACE('',(#4780),#1187,.F.);
#32462=ADVANCED_FACE('',(#4781),#584,.F.);
#32463=ADVANCED_FACE('',(#4782),#1188,.F.);
#32464=ADVANCED_FACE('',(#4783),#585,.F.);
#32465=ADVANCED_FACE('',(#4784),#1189,.F.);
#32466=ADVANCED_FACE('',(#4785),#586,.F.);
#32467=ADVANCED_FACE('',(#4786),#1190,.F.);
#32468=ADVANCED_FACE('',(#4787),#587,.F.);
#32469=ADVANCED_FACE('',(#4788),#588,.F.);
#32470=ADVANCED_FACE('',(#4789),#589,.F.);
#32471=ADVANCED_FACE('',(#4790),#590,.F.);
#32472=ADVANCED_FACE('',(#4791),#31413,.T.);
#32473=ADVANCED_FACE('',(#4792),#31414,.T.);
#32474=ADVANCED_FACE('',(#4793),#31415,.T.);
#32475=ADVANCED_FACE('',(#4794),#31416,.T.);
#32476=ADVANCED_FACE('',(#4795),#31417,.T.);
#32477=ADVANCED_FACE('',(#4796),#31418,.T.);
#32478=ADVANCED_FACE('',(#4797),#31419,.T.);
#32479=ADVANCED_FACE('',(#4798),#31420,.T.);
#32480=ADVANCED_FACE('',(#4799),#31421,.T.);
#32481=ADVANCED_FACE('',(#4800),#31422,.T.);
#32482=ADVANCED_FACE('',(#4801),#31423,.T.);
#32483=ADVANCED_FACE('',(#4802),#31424,.F.);
#32484=ADVANCED_FACE('',(#4803),#31425,.F.);
#32485=ADVANCED_FACE('',(#4804),#31426,.F.);
#32486=ADVANCED_FACE('',(#4805),#31427,.F.);
#32487=ADVANCED_FACE('',(#4806),#31428,.F.);
#32488=ADVANCED_FACE('',(#4807),#1191,.F.);
#32489=ADVANCED_FACE('',(#4808),#31429,.F.);
#32490=ADVANCED_FACE('',(#4809),#1192,.F.);
#32491=ADVANCED_FACE('',(#4810),#31430,.T.);
#32492=ADVANCED_FACE('',(#4811),#1193,.T.);
#32493=ADVANCED_FACE('',(#4812),#31431,.T.);
#32494=ADVANCED_FACE('',(#4813),#1194,.T.);
#32495=ADVANCED_FACE('',(#4814),#31432,.F.);
#32496=ADVANCED_FACE('',(#4815),#1195,.F.);
#32497=ADVANCED_FACE('',(#4816),#31433,.F.);
#32498=ADVANCED_FACE('',(#4817),#1196,.F.);
#32499=ADVANCED_FACE('',(#4818),#31434,.T.);
#32500=ADVANCED_FACE('',(#4819),#1197,.T.);
#32501=ADVANCED_FACE('',(#4820),#31435,.T.);
#32502=ADVANCED_FACE('',(#4821),#1198,.T.);
#32503=ADVANCED_FACE('',(#4822,#1978),#31436,.F.);
#32504=ADVANCED_FACE('',(#4823,#1979),#31437,.T.);
#32505=ADVANCED_FACE('',(#4824),#31438,.F.);
#32506=ADVANCED_FACE('',(#4825),#1199,.F.);
#32507=ADVANCED_FACE('',(#4826),#31439,.F.);
#32508=ADVANCED_FACE('',(#4827),#1200,.F.);
#32509=ADVANCED_FACE('',(#4828),#31440,.T.);
#32510=ADVANCED_FACE('',(#4829),#1201,.T.);
#32511=ADVANCED_FACE('',(#4830),#31441,.T.);
#32512=ADVANCED_FACE('',(#4831),#1202,.T.);
#32513=ADVANCED_FACE('',(#4832),#31442,.F.);
#32514=ADVANCED_FACE('',(#4833),#1203,.F.);
#32515=ADVANCED_FACE('',(#4834),#31443,.F.);
#32516=ADVANCED_FACE('',(#4835),#1204,.F.);
#32517=ADVANCED_FACE('',(#4836),#31444,.T.);
#32518=ADVANCED_FACE('',(#4837),#1205,.T.);
#32519=ADVANCED_FACE('',(#4838),#31445,.T.);
#32520=ADVANCED_FACE('',(#4839),#1206,.T.);
#32521=ADVANCED_FACE('',(#4840,#1980),#31446,.F.);
#32522=ADVANCED_FACE('',(#4841,#1981),#31447,.T.);
#32523=ADVANCED_FACE('',(#4842),#31448,.F.);
#32524=ADVANCED_FACE('',(#4843),#1207,.F.);
#32525=ADVANCED_FACE('',(#4844),#31449,.F.);
#32526=ADVANCED_FACE('',(#4845),#1208,.F.);
#32527=ADVANCED_FACE('',(#4846),#31450,.T.);
#32528=ADVANCED_FACE('',(#4847),#1209,.T.);
#32529=ADVANCED_FACE('',(#4848),#31451,.T.);
#32530=ADVANCED_FACE('',(#4849),#1210,.T.);
#32531=ADVANCED_FACE('',(#4850),#31452,.F.);
#32532=ADVANCED_FACE('',(#4851),#1211,.F.);
#32533=ADVANCED_FACE('',(#4852),#31453,.F.);
#32534=ADVANCED_FACE('',(#4853),#1212,.F.);
#32535=ADVANCED_FACE('',(#4854),#31454,.T.);
#32536=ADVANCED_FACE('',(#4855),#1213,.T.);
#32537=ADVANCED_FACE('',(#4856),#31455,.T.);
#32538=ADVANCED_FACE('',(#4857),#1214,.T.);
#32539=ADVANCED_FACE('',(#4858,#1982),#31456,.F.);
#32540=ADVANCED_FACE('',(#4859,#1983),#31457,.T.);
#32541=ADVANCED_FACE('',(#4860),#31458,.F.);
#32542=ADVANCED_FACE('',(#4861),#1215,.F.);
#32543=ADVANCED_FACE('',(#4862),#31459,.F.);
#32544=ADVANCED_FACE('',(#4863),#1216,.F.);
#32545=ADVANCED_FACE('',(#4864),#31460,.T.);
#32546=ADVANCED_FACE('',(#4865),#1217,.T.);
#32547=ADVANCED_FACE('',(#4866),#31461,.T.);
#32548=ADVANCED_FACE('',(#4867),#1218,.T.);
#32549=ADVANCED_FACE('',(#4868),#31462,.F.);
#32550=ADVANCED_FACE('',(#4869),#1219,.F.);
#32551=ADVANCED_FACE('',(#4870),#31463,.F.);
#32552=ADVANCED_FACE('',(#4871),#1220,.F.);
#32553=ADVANCED_FACE('',(#4872),#31464,.T.);
#32554=ADVANCED_FACE('',(#4873),#1221,.T.);
#32555=ADVANCED_FACE('',(#4874),#31465,.T.);
#32556=ADVANCED_FACE('',(#4875),#1222,.T.);
#32557=ADVANCED_FACE('',(#4876,#1984),#31466,.F.);
#32558=ADVANCED_FACE('',(#4877,#1985),#31467,.T.);
#32559=ADVANCED_FACE('',(#4878,#1986),#31468,.F.);
#32560=ADVANCED_FACE('',(#4879),#31469,.F.);
#32561=ADVANCED_FACE('',(#4880),#1223,.F.);
#32562=ADVANCED_FACE('',(#4881),#31470,.F.);
#32563=ADVANCED_FACE('',(#4882),#1224,.F.);
#32564=ADVANCED_FACE('',(#4883),#1225,.T.);
#32565=ADVANCED_FACE('',(#4884),#1226,.T.);
#32566=ADVANCED_FACE('',(#4885),#31471,.T.);
#32567=ADVANCED_FACE('',(#4886,#1987),#31472,.F.);
#32568=ADVANCED_FACE('',(#4887),#31473,.F.);
#32569=ADVANCED_FACE('',(#4888),#1227,.T.);
#32570=ADVANCED_FACE('',(#4889),#1228,.F.);
#32571=ADVANCED_FACE('',(#4890),#31474,.F.);
#32572=ADVANCED_FACE('',(#4891),#1229,.F.);
#32573=ADVANCED_FACE('',(#4892),#31475,.T.);
#32574=ADVANCED_FACE('',(#4893),#31476,.T.);
#32575=ADVANCED_FACE('',(#4894),#1230,.T.);
#32576=ADVANCED_FACE('',(#4895),#31477,.T.);
#32577=ADVANCED_FACE('',(#4896,#1988),#31478,.F.);
#32578=ADVANCED_FACE('',(#4897),#31479,.F.);
#32579=ADVANCED_FACE('',(#4898),#1231,.F.);
#32580=ADVANCED_FACE('',(#4899),#31480,.F.);
#32581=ADVANCED_FACE('',(#4900),#1232,.F.);
#32582=ADVANCED_FACE('',(#4901),#1233,.T.);
#32583=ADVANCED_FACE('',(#4902),#31481,.T.);
#32584=ADVANCED_FACE('',(#4903),#1234,.T.);
#32585=ADVANCED_FACE('',(#4904),#31482,.T.);
#32586=ADVANCED_FACE('',(#4905,#1989),#31483,.F.);
#32587=ADVANCED_FACE('',(#4906),#31484,.F.);
#32588=ADVANCED_FACE('',(#4907),#1235,.T.);
#32589=ADVANCED_FACE('',(#4908),#1236,.F.);
#32590=ADVANCED_FACE('',(#4909),#31485,.F.);
#32591=ADVANCED_FACE('',(#4910),#1237,.F.);
#32592=ADVANCED_FACE('',(#4911),#31486,.T.);
#32593=ADVANCED_FACE('',(#4912),#1238,.T.);
#32594=ADVANCED_FACE('',(#4913),#31487,.T.);
#32595=ADVANCED_FACE('',(#4914,#1990),#31488,.F.);
#32596=ADVANCED_FACE('',(#4915),#31489,.F.);
#32597=ADVANCED_FACE('',(#4916),#1239,.F.);
#32598=ADVANCED_FACE('',(#4917),#31490,.F.);
#32599=ADVANCED_FACE('',(#4918),#1240,.F.);
#32600=ADVANCED_FACE('',(#4919),#31491,.T.);
#32601=ADVANCED_FACE('',(#4920),#1241,.T.);
#32602=ADVANCED_FACE('',(#4921),#31492,.T.);
#32603=ADVANCED_FACE('',(#4922),#1242,.T.);
#32604=ADVANCED_FACE('',(#4923,#1991),#31493,.F.);
#32605=ADVANCED_FACE('',(#4924),#31494,.F.);
#32606=ADVANCED_FACE('',(#4925),#31495,.T.);
#32607=ADVANCED_FACE('',(#4926),#1243,.F.);
#32608=ADVANCED_FACE('',(#4927),#31496,.F.);
#32609=ADVANCED_FACE('',(#4928),#1244,.F.);
#32610=ADVANCED_FACE('',(#4929),#1245,.T.);
#32611=ADVANCED_FACE('',(#4930),#31497,.T.);
#32612=ADVANCED_FACE('',(#4931),#1246,.T.);
#32613=ADVANCED_FACE('',(#4932,#1992),#31498,.F.);
#32614=ADVANCED_FACE('',(#4933),#31499,.F.);
#32615=ADVANCED_FACE('',(#4934),#1247,.F.);
#32616=ADVANCED_FACE('',(#4935),#31500,.F.);
#32617=ADVANCED_FACE('',(#4936),#1248,.F.);
#32618=ADVANCED_FACE('',(#4937),#31501,.T.);
#32619=ADVANCED_FACE('',(#4938),#1249,.T.);
#32620=ADVANCED_FACE('',(#4939),#31502,.T.);
#32621=ADVANCED_FACE('',(#4940),#1250,.T.);
#32622=ADVANCED_FACE('',(#4941,#1993),#31503,.F.);
#32623=ADVANCED_FACE('',(#4942),#31504,.F.);
#32624=ADVANCED_FACE('',(#4943),#31505,.T.);
#32625=ADVANCED_FACE('',(#4944),#1251,.F.);
#32626=ADVANCED_FACE('',(#4945),#31506,.F.);
#32627=ADVANCED_FACE('',(#4946),#1252,.F.);
#32628=ADVANCED_FACE('',(#4947),#1253,.T.);
#32629=ADVANCED_FACE('',(#4948),#31507,.T.);
#32630=ADVANCED_FACE('',(#4949),#1254,.T.);
#32631=ADVANCED_FACE('',(#4950),#31508,.F.);
#32632=ADVANCED_FACE('',(#4951),#1255,.F.);
#32633=ADVANCED_FACE('',(#4952),#31509,.F.);
#32634=ADVANCED_FACE('',(#4953),#1256,.F.);
#32635=ADVANCED_FACE('',(#4954),#31510,.T.);
#32636=ADVANCED_FACE('',(#4955),#1257,.T.);
#32637=ADVANCED_FACE('',(#4956),#31511,.T.);
#32638=ADVANCED_FACE('',(#4957),#1258,.T.);
#32639=ADVANCED_FACE('',(#4958),#31512,.F.);
#32640=ADVANCED_FACE('',(#4959),#1259,.F.);
#32641=ADVANCED_FACE('',(#4960),#31513,.F.);
#32642=ADVANCED_FACE('',(#4961),#1260,.F.);
#32643=ADVANCED_FACE('',(#4962),#31514,.T.);
#32644=ADVANCED_FACE('',(#4963),#1261,.T.);
#32645=ADVANCED_FACE('',(#4964),#31515,.T.);
#32646=ADVANCED_FACE('',(#4965),#1262,.T.);
#32647=ADVANCED_FACE('',(#4966,#1994),#31516,.F.);
#32648=ADVANCED_FACE('',(#4967,#1995),#31517,.T.);
#32649=ADVANCED_FACE('',(#4968),#31518,.F.);
#32650=ADVANCED_FACE('',(#4969),#1263,.F.);
#32651=ADVANCED_FACE('',(#4970),#31519,.F.);
#32652=ADVANCED_FACE('',(#4971),#1264,.F.);
#32653=ADVANCED_FACE('',(#4972),#31520,.T.);
#32654=ADVANCED_FACE('',(#4973),#1265,.T.);
#32655=ADVANCED_FACE('',(#4974),#31521,.T.);
#32656=ADVANCED_FACE('',(#4975),#1266,.T.);
#32657=ADVANCED_FACE('',(#4976),#31522,.F.);
#32658=ADVANCED_FACE('',(#4977),#1267,.F.);
#32659=ADVANCED_FACE('',(#4978),#31523,.F.);
#32660=ADVANCED_FACE('',(#4979),#1268,.F.);
#32661=ADVANCED_FACE('',(#4980),#31524,.T.);
#32662=ADVANCED_FACE('',(#4981),#1269,.T.);
#32663=ADVANCED_FACE('',(#4982),#31525,.T.);
#32664=ADVANCED_FACE('',(#4983),#1270,.T.);
#32665=ADVANCED_FACE('',(#4984,#1996),#31526,.F.);
#32666=ADVANCED_FACE('',(#4985,#1997),#31527,.T.);
#32667=ADVANCED_FACE('',(#4986),#31528,.F.);
#32668=ADVANCED_FACE('',(#4987),#1271,.F.);
#32669=ADVANCED_FACE('',(#4988),#31529,.F.);
#32670=ADVANCED_FACE('',(#4989),#1272,.F.);
#32671=ADVANCED_FACE('',(#4990),#31530,.T.);
#32672=ADVANCED_FACE('',(#4991),#1273,.T.);
#32673=ADVANCED_FACE('',(#4992),#31531,.T.);
#32674=ADVANCED_FACE('',(#4993),#1274,.T.);
#32675=ADVANCED_FACE('',(#4994),#31532,.F.);
#32676=ADVANCED_FACE('',(#4995),#1275,.F.);
#32677=ADVANCED_FACE('',(#4996),#31533,.F.);
#32678=ADVANCED_FACE('',(#4997),#1276,.F.);
#32679=ADVANCED_FACE('',(#4998),#31534,.T.);
#32680=ADVANCED_FACE('',(#4999),#1277,.T.);
#32681=ADVANCED_FACE('',(#5000),#31535,.T.);
#32682=ADVANCED_FACE('',(#5001),#1278,.T.);
#32683=ADVANCED_FACE('',(#5002,#1998),#31536,.F.);
#32684=ADVANCED_FACE('',(#5003,#1999),#31537,.T.);
#32685=ADVANCED_FACE('',(#5004),#1279,.F.);
#32686=ADVANCED_FACE('',(#5005),#31538,.F.);
#32687=ADVANCED_FACE('',(#5006),#1280,.F.);
#32688=ADVANCED_FACE('',(#5007),#31539,.F.);
#32689=ADVANCED_FACE('',(#5008),#1281,.F.);
#32690=ADVANCED_FACE('',(#5009),#31540,.F.);
#32691=ADVANCED_FACE('',(#5010),#1282,.F.);
#32692=ADVANCED_FACE('',(#5011),#31541,.F.);
#32693=ADVANCED_FACE('',(#5012),#1283,.T.);
#32694=ADVANCED_FACE('',(#5013),#31542,.T.);
#32695=ADVANCED_FACE('',(#5014),#1284,.T.);
#32696=ADVANCED_FACE('',(#5015),#31543,.T.);
#32697=ADVANCED_FACE('',(#5016),#1285,.T.);
#32698=ADVANCED_FACE('',(#5017),#31544,.T.);
#32699=ADVANCED_FACE('',(#5018),#1286,.T.);
#32700=ADVANCED_FACE('',(#5019),#31545,.T.);
#32701=ADVANCED_FACE('',(#5020,#2000),#31546,.F.);
#32702=ADVANCED_FACE('',(#5021,#2001),#31547,.T.);
#32703=ADVANCED_FACE('',(#5022),#1287,.F.);
#32704=ADVANCED_FACE('',(#5023),#31548,.F.);
#32705=ADVANCED_FACE('',(#5024),#1288,.F.);
#32706=ADVANCED_FACE('',(#5025),#31549,.F.);
#32707=ADVANCED_FACE('',(#5026),#1289,.F.);
#32708=ADVANCED_FACE('',(#5027),#31550,.F.);
#32709=ADVANCED_FACE('',(#5028),#1290,.F.);
#32710=ADVANCED_FACE('',(#5029),#31551,.F.);
#32711=ADVANCED_FACE('',(#5030),#1291,.T.);
#32712=ADVANCED_FACE('',(#5031),#31552,.T.);
#32713=ADVANCED_FACE('',(#5032),#1292,.T.);
#32714=ADVANCED_FACE('',(#5033),#31553,.T.);
#32715=ADVANCED_FACE('',(#5034),#1293,.T.);
#32716=ADVANCED_FACE('',(#5035),#31554,.T.);
#32717=ADVANCED_FACE('',(#5036),#1294,.T.);
#32718=ADVANCED_FACE('',(#5037),#31555,.T.);
#32719=ADVANCED_FACE('',(#5038,#2002),#31556,.F.);
#32720=ADVANCED_FACE('',(#5039,#2003),#31557,.T.);
#32721=ADVANCED_FACE('',(#5040),#1295,.F.);
#32722=ADVANCED_FACE('',(#5041),#31558,.F.);
#32723=ADVANCED_FACE('',(#5042),#1296,.F.);
#32724=ADVANCED_FACE('',(#5043),#31559,.F.);
#32725=ADVANCED_FACE('',(#5044),#1297,.F.);
#32726=ADVANCED_FACE('',(#5045),#31560,.F.);
#32727=ADVANCED_FACE('',(#5046),#1298,.F.);
#32728=ADVANCED_FACE('',(#5047),#31561,.F.);
#32729=ADVANCED_FACE('',(#5048),#1299,.T.);
#32730=ADVANCED_FACE('',(#5049),#31562,.T.);
#32731=ADVANCED_FACE('',(#5050),#1300,.T.);
#32732=ADVANCED_FACE('',(#5051),#31563,.T.);
#32733=ADVANCED_FACE('',(#5052),#1301,.T.);
#32734=ADVANCED_FACE('',(#5053),#31564,.T.);
#32735=ADVANCED_FACE('',(#5054),#1302,.T.);
#32736=ADVANCED_FACE('',(#5055),#31565,.T.);
#32737=ADVANCED_FACE('',(#5056,#2004),#31566,.F.);
#32738=ADVANCED_FACE('',(#5057,#2005),#31567,.T.);
#32739=ADVANCED_FACE('',(#5058),#1303,.F.);
#32740=ADVANCED_FACE('',(#5059),#31568,.F.);
#32741=ADVANCED_FACE('',(#5060),#1304,.F.);
#32742=ADVANCED_FACE('',(#5061),#31569,.F.);
#32743=ADVANCED_FACE('',(#5062),#1305,.F.);
#32744=ADVANCED_FACE('',(#5063),#31570,.F.);
#32745=ADVANCED_FACE('',(#5064),#1306,.F.);
#32746=ADVANCED_FACE('',(#5065),#31571,.F.);
#32747=ADVANCED_FACE('',(#5066),#1307,.T.);
#32748=ADVANCED_FACE('',(#5067),#31572,.T.);
#32749=ADVANCED_FACE('',(#5068),#1308,.T.);
#32750=ADVANCED_FACE('',(#5069),#31573,.T.);
#32751=ADVANCED_FACE('',(#5070),#1309,.T.);
#32752=ADVANCED_FACE('',(#5071),#31574,.T.);
#32753=ADVANCED_FACE('',(#5072),#1310,.T.);
#32754=ADVANCED_FACE('',(#5073),#31575,.T.);
#32755=ADVANCED_FACE('',(#5074,#2006),#31576,.F.);
#32756=ADVANCED_FACE('',(#5075,#2007),#31577,.T.);
#32757=ADVANCED_FACE('',(#5076),#1311,.F.);
#32758=ADVANCED_FACE('',(#5077),#1312,.F.);
#32759=ADVANCED_FACE('',(#5078),#1313,.F.);
#32760=ADVANCED_FACE('',(#5079),#1314,.F.);
#32761=ADVANCED_FACE('',(#5080),#1315,.F.);
#32762=ADVANCED_FACE('',(#5081),#1316,.F.);
#32763=ADVANCED_FACE('',(#5082),#1317,.F.);
#32764=ADVANCED_FACE('',(#5083),#1318,.F.);
#32765=ADVANCED_FACE('',(#5084),#1319,.F.);
#32766=ADVANCED_FACE('',(#5085),#1320,.F.);
#32767=ADVANCED_FACE('',(#5086),#1321,.F.);
#32768=ADVANCED_FACE('',(#5087),#1322,.F.);
#32769=ADVANCED_FACE('',(#5088),#1323,.F.);
#32770=ADVANCED_FACE('',(#5089),#1324,.F.);
#32771=ADVANCED_FACE('',(#5090),#1325,.F.);
#32772=ADVANCED_FACE('',(#5091),#1326,.F.);
#32773=ADVANCED_FACE('',(#5092,#2008,#2009,#2010,#2011,#2012,#2013,#2014,
#2015),#31578,.F.);
#32774=ADVANCED_FACE('',(#5093),#31579,.F.);
#32775=ADVANCED_FACE('',(#5094,#2016,#2017,#2018,#2019,#2020,#2021,#2022,
#2023),#31580,.F.);
#32776=ADVANCED_FACE('',(#5095),#31581,.F.);
#32777=ADVANCED_FACE('',(#5096,#2024),#31582,.T.);
#32778=ADVANCED_FACE('',(#5097,#2025,#2026,#2027,#2028,#2029,#2030,#2031,
#2032),#31583,.T.);
#32779=ADVANCED_FACE('',(#5098),#31584,.T.);
#32780=ADVANCED_FACE('',(#5099,#2033,#2034,#2035,#2036,#2037,#2038,#2039,
#2040),#31585,.T.);
#32781=ADVANCED_FACE('',(#5100),#31586,.T.);
#32782=ADVANCED_FACE('',(#5101,#2041),#31587,.T.);
#32783=ADVANCED_FACE('',(#5102,#2042,#2043,#2044),#31588,.F.);
#32784=ADVANCED_FACE('',(#5103,#2045,#2046,#2047),#31589,.F.);
#32785=ADVANCED_FACE('',(#5104),#31590,.T.);
#32786=ADVANCED_FACE('',(#5105),#591,.F.);
#32787=ADVANCED_FACE('',(#5106),#1327,.F.);
#32788=ADVANCED_FACE('',(#5107),#592,.F.);
#32789=ADVANCED_FACE('',(#5108),#1328,.F.);
#32790=ADVANCED_FACE('',(#5109),#593,.F.);
#32791=ADVANCED_FACE('',(#5110),#1329,.F.);
#32792=ADVANCED_FACE('',(#5111),#594,.F.);
#32793=ADVANCED_FACE('',(#5112),#1330,.F.);
#32794=ADVANCED_FACE('',(#5113),#595,.F.);
#32795=ADVANCED_FACE('',(#5114),#1331,.F.);
#32796=ADVANCED_FACE('',(#5115),#596,.F.);
#32797=ADVANCED_FACE('',(#5116),#1332,.F.);
#32798=ADVANCED_FACE('',(#5117),#1333,.F.);
#32799=ADVANCED_FACE('',(#5118),#1334,.F.);
#32800=ADVANCED_FACE('',(#5119),#1335,.F.);
#32801=ADVANCED_FACE('',(#5120),#1336,.F.);
#32802=ADVANCED_FACE('',(#5121),#1337,.F.);
#32803=ADVANCED_FACE('',(#5122),#1338,.F.);
#32804=ADVANCED_FACE('',(#5123),#1339,.F.);
#32805=ADVANCED_FACE('',(#5124),#1340,.F.);
#32806=ADVANCED_FACE('',(#5125),#1341,.F.);
#32807=ADVANCED_FACE('',(#5126),#1342,.F.);
#32808=ADVANCED_FACE('',(#5127,#2048,#2049,#2050,#2051,#2052,#2053,#2054,
#2055,#2056,#2057),#31591,.T.);
#32809=ADVANCED_FACE('',(#5128),#31592,.T.);
#32810=ADVANCED_FACE('',(#5129,#2058,#2059,#2060,#2061,#2062,#2063,#2064,
#2065,#2066,#2067),#31593,.T.);
#32811=ADVANCED_FACE('',(#5130,#2068,#2069,#2070),#31594,.F.);
#32812=ADVANCED_FACE('',(#5131,#2071,#2072,#2073),#31595,.F.);
#32813=ADVANCED_FACE('',(#5132),#31596,.T.);
#32814=ADVANCED_FACE('',(#5133),#597,.F.);
#32815=ADVANCED_FACE('',(#5134),#1343,.F.);
#32816=ADVANCED_FACE('',(#5135),#598,.F.);
#32817=ADVANCED_FACE('',(#5136),#1344,.F.);
#32818=ADVANCED_FACE('',(#5137),#599,.F.);
#32819=ADVANCED_FACE('',(#5138),#1345,.F.);
#32820=ADVANCED_FACE('',(#5139),#600,.F.);
#32821=ADVANCED_FACE('',(#5140),#1346,.F.);
#32822=ADVANCED_FACE('',(#5141),#601,.F.);
#32823=ADVANCED_FACE('',(#5142),#1347,.F.);
#32824=ADVANCED_FACE('',(#5143),#602,.F.);
#32825=ADVANCED_FACE('',(#5144),#1348,.F.);
#32826=ADVANCED_FACE('',(#5145),#1349,.F.);
#32827=ADVANCED_FACE('',(#5146),#1350,.F.);
#32828=ADVANCED_FACE('',(#5147),#1351,.F.);
#32829=ADVANCED_FACE('',(#5148),#1352,.F.);
#32830=ADVANCED_FACE('',(#5149),#1353,.F.);
#32831=ADVANCED_FACE('',(#5150),#1354,.F.);
#32832=ADVANCED_FACE('',(#5151),#1355,.F.);
#32833=ADVANCED_FACE('',(#5152),#1356,.F.);
#32834=ADVANCED_FACE('',(#5153),#1357,.F.);
#32835=ADVANCED_FACE('',(#5154),#1358,.F.);
#32836=ADVANCED_FACE('',(#5155,#2074,#2075,#2076,#2077,#2078,#2079,#2080,
#2081,#2082,#2083),#31597,.T.);
#32837=ADVANCED_FACE('',(#5156),#31598,.T.);
#32838=ADVANCED_FACE('',(#5157,#2084,#2085,#2086,#2087,#2088,#2089,#2090,
#2091,#2092,#2093),#31599,.T.);
#32839=ADVANCED_FACE('',(#5158),#1359,.F.);
#32840=ADVANCED_FACE('',(#5159),#1360,.F.);
#32841=ADVANCED_FACE('',(#5160),#1361,.F.);
#32842=ADVANCED_FACE('',(#5161),#1362,.F.);
#32843=ADVANCED_FACE('',(#5162),#1363,.F.);
#32844=ADVANCED_FACE('',(#5163),#1364,.F.);
#32845=ADVANCED_FACE('',(#5164),#31600,.T.);
#32846=ADVANCED_FACE('',(#5165),#31601,.T.);
#32847=ADVANCED_FACE('',(#5166),#31602,.T.);
#32848=ADVANCED_FACE('',(#5167),#31603,.T.);
#32849=ADVANCED_FACE('',(#5168,#2094,#2095,#2096,#2097,#2098,#2099),#31604,
 .T.);
#32850=ADVANCED_FACE('',(#5169,#2100,#2101,#2102,#2103,#2104,#2105),#31605,
 .F.);
#32851=ADVANCED_FACE('',(#5170),#31606,.F.);
#32852=ADVANCED_FACE('',(#5171),#31607,.F.);
#32853=ADVANCED_FACE('',(#5172),#31608,.T.);
#32854=ADVANCED_FACE('',(#5173),#1365,.F.);
#32855=ADVANCED_FACE('',(#5174),#31609,.T.);
#32856=ADVANCED_FACE('',(#5175),#31610,.T.);
#32857=ADVANCED_FACE('',(#5176),#31611,.T.);
#32858=ADVANCED_FACE('',(#5177),#31612,.T.);
#32859=ADVANCED_FACE('',(#5178),#31613,.T.);
#32860=ADVANCED_FACE('',(#5179),#31614,.T.);
#32861=ADVANCED_FACE('',(#5180),#1366,.F.);
#32862=ADVANCED_FACE('',(#5181),#1367,.F.);
#32863=ADVANCED_FACE('',(#5182),#1368,.F.);
#32864=ADVANCED_FACE('',(#5183),#1369,.F.);
#32865=ADVANCED_FACE('',(#5184),#31615,.F.);
#32866=ADVANCED_FACE('',(#5185),#31616,.F.);
#32867=ADVANCED_FACE('',(#5186),#31617,.F.);
#32868=ADVANCED_FACE('',(#5187),#31618,.F.);
#32869=ADVANCED_FACE('',(#5188),#31619,.T.);
#32870=ADVANCED_FACE('',(#5189),#31620,.T.);
#32871=ADVANCED_FACE('',(#5190),#31621,.T.);
#32872=ADVANCED_FACE('',(#5191),#31622,.T.);
#32873=ADVANCED_FACE('',(#5192,#2106,#2107,#2108,#2109,#2110),#31623,.T.);
#32874=ADVANCED_FACE('',(#5193,#2111,#2112,#2113,#2114,#2115),#31624,.F.);
#32875=ADVANCED_FACE('',(#5194),#1370,.T.);
#32876=ADVANCED_FACE('',(#5195),#1371,.F.);
#32877=ADVANCED_FACE('',(#5196),#31625,.F.);
#32878=ADVANCED_FACE('',(#5197),#31626,.F.);
#32879=ADVANCED_FACE('',(#5198),#1372,.F.);
#32880=ADVANCED_FACE('',(#5199),#31627,.F.);
#32881=ADVANCED_FACE('',(#5200),#898,.F.);
#32882=ADVANCED_FACE('',(#5201,#2116),#31628,.T.);
#32883=ADVANCED_FACE('',(#5202,#2117),#1373,.T.);
#32884=ADVANCED_FACE('',(#5203),#899,.F.);
#32885=ADVANCED_FACE('',(#5204,#2118),#31629,.T.);
#32886=ADVANCED_FACE('',(#5205),#1374,.T.);
#32887=ADVANCED_FACE('',(#5206),#603,.T.);
#32888=ADVANCED_FACE('',(#5207),#1375,.T.);
#32889=ADVANCED_FACE('',(#5208),#604,.T.);
#32890=ADVANCED_FACE('',(#5209),#1376,.T.);
#32891=ADVANCED_FACE('',(#5210),#605,.T.);
#32892=ADVANCED_FACE('',(#5211),#31630,.T.);
#32893=ADVANCED_FACE('',(#5212),#1377,.F.);
#32894=ADVANCED_FACE('',(#5213),#31631,.F.);
#32895=ADVANCED_FACE('',(#5214),#31632,.F.);
#32896=ADVANCED_FACE('',(#5215),#1378,.F.);
#32897=ADVANCED_FACE('',(#5216),#31633,.T.);
#32898=ADVANCED_FACE('',(#5217),#1379,.T.);
#32899=ADVANCED_FACE('',(#5218),#606,.T.);
#32900=ADVANCED_FACE('',(#5219),#31634,.T.);
#32901=ADVANCED_FACE('',(#5220),#900,.F.);
#32902=ADVANCED_FACE('',(#5221,#2119),#31635,.T.);
#32903=ADVANCED_FACE('',(#5222),#607,.T.);
#32904=ADVANCED_FACE('',(#5223),#608,.T.);
#32905=ADVANCED_FACE('',(#5224,#2120),#31636,.T.);
#32906=ADVANCED_FACE('',(#5225),#901,.F.);
#32907=ADVANCED_FACE('',(#5226),#1380,.T.);
#32908=ADVANCED_FACE('',(#5227),#609,.T.);
#32909=ADVANCED_FACE('',(#5228,#2121),#1381,.T.);
#32910=ADVANCED_FACE('',(#5229),#31637,.T.);
#32911=ADVANCED_FACE('',(#5230),#610,.T.);
#32912=ADVANCED_FACE('',(#5231),#1382,.T.);
#32913=ADVANCED_FACE('',(#5232,#2122),#31638,.T.);
#32914=ADVANCED_FACE('',(#5233),#31639,.F.);
#32915=ADVANCED_FACE('',(#5234),#1383,.F.);
#32916=ADVANCED_FACE('',(#5235),#31640,.F.);
#32917=ADVANCED_FACE('',(#5236),#1384,.F.);
#32918=ADVANCED_FACE('',(#5237),#31641,.F.);
#32919=ADVANCED_FACE('',(#5238),#611,.T.);
#32920=ADVANCED_FACE('',(#5239,#2123),#31642,.T.);
#32921=ADVANCED_FACE('',(#5240),#1385,.T.);
#32922=ADVANCED_FACE('',(#5241),#902,.F.);
#32923=ADVANCED_FACE('',(#5242),#1386,.T.);
#32924=ADVANCED_FACE('',(#5243),#903,.F.);
#32925=ADVANCED_FACE('',(#5244,#2124),#31643,.T.);
#32926=ADVANCED_FACE('',(#5245),#612,.T.);
#32927=ADVANCED_FACE('',(#5246),#1387,.T.);
#32928=ADVANCED_FACE('',(#5247),#613,.T.);
#32929=ADVANCED_FACE('',(#5248),#31644,.T.);
#32930=ADVANCED_FACE('',(#5249),#1388,.F.);
#32931=ADVANCED_FACE('',(#5250),#31645,.F.);
#32932=ADVANCED_FACE('',(#5251),#31646,.F.);
#32933=ADVANCED_FACE('',(#5252),#1389,.F.);
#32934=ADVANCED_FACE('',(#5253),#31647,.T.);
#32935=ADVANCED_FACE('',(#5254),#1390,.T.);
#32936=ADVANCED_FACE('',(#5255),#904,.F.);
#32937=ADVANCED_FACE('',(#5256,#2125),#31648,.T.);
#32938=ADVANCED_FACE('',(#5257),#614,.T.);
#32939=ADVANCED_FACE('',(#5258),#615,.T.);
#32940=ADVANCED_FACE('',(#5259,#2126),#31649,.T.);
#32941=ADVANCED_FACE('',(#5260),#905,.F.);
#32942=ADVANCED_FACE('',(#5261),#31650,.F.);
#32943=ADVANCED_FACE('',(#5262),#31651,.F.);
#32944=ADVANCED_FACE('',(#5263),#31652,.F.);
#32945=ADVANCED_FACE('',(#5264,#2127),#31653,.T.);
#32946=ADVANCED_FACE('',(#5265),#1391,.F.);
#32947=ADVANCED_FACE('',(#5266),#1392,.T.);
#32948=ADVANCED_FACE('',(#5267,#2128),#31654,.F.);
#32949=ADVANCED_FACE('',(#5268),#1393,.F.);
#32950=ADVANCED_FACE('',(#5269),#1394,.T.);
#32951=ADVANCED_FACE('',(#5270,#2129),#31655,.F.);
#32952=ADVANCED_FACE('',(#5271,#2130),#31656,.T.);
#32953=ADVANCED_FACE('',(#5272),#906,.T.);
#32954=ADVANCED_FACE('',(#5273),#1395,.T.);
#32955=ADVANCED_FACE('',(#5274,#2131),#31657,.T.);
#32956=ADVANCED_FACE('',(#5275),#907,.F.);
#32957=ADVANCED_FACE('',(#5276,#2132),#31658,.F.);
#32958=ADVANCED_FACE('',(#5277),#31659,.F.);
#32959=ADVANCED_FACE('',(#5278),#31660,.F.);
#32960=ADVANCED_FACE('',(#5279),#1396,.F.);
#32961=ADVANCED_FACE('',(#5280),#31661,.F.);
#32962=ADVANCED_FACE('',(#5281),#1397,.T.);
#32963=ADVANCED_FACE('',(#5282),#1398,.T.);
#32964=ADVANCED_FACE('',(#5283),#1399,.T.);
#32965=ADVANCED_FACE('',(#5284),#1400,.T.);
#32966=ADVANCED_FACE('',(#5285),#1401,.T.);
#32967=ADVANCED_FACE('',(#5286),#1402,.T.);
#32968=ADVANCED_FACE('',(#5287),#1403,.T.);
#32969=ADVANCED_FACE('',(#5288),#1404,.T.);
#32970=ADVANCED_FACE('',(#5289),#1405,.T.);
#32971=ADVANCED_FACE('',(#5290),#1406,.T.);
#32972=ADVANCED_FACE('',(#5291),#1407,.T.);
#32973=ADVANCED_FACE('',(#5292),#1408,.T.);
#32974=ADVANCED_FACE('',(#5293),#1409,.T.);
#32975=ADVANCED_FACE('',(#5294),#1410,.T.);
#32976=ADVANCED_FACE('',(#5295),#1411,.T.);
#32977=ADVANCED_FACE('',(#5296),#1412,.T.);
#32978=ADVANCED_FACE('',(#5297),#1413,.T.);
#32979=ADVANCED_FACE('',(#5298),#1414,.T.);
#32980=ADVANCED_FACE('',(#5299),#1415,.T.);
#32981=ADVANCED_FACE('',(#5300),#1416,.T.);
#32982=ADVANCED_FACE('',(#5301),#1417,.T.);
#32983=ADVANCED_FACE('',(#5302),#1418,.T.);
#32984=ADVANCED_FACE('',(#5303),#1419,.T.);
#32985=ADVANCED_FACE('',(#5304),#1420,.T.);
#32986=ADVANCED_FACE('',(#5305),#1421,.T.);
#32987=ADVANCED_FACE('',(#5306),#1422,.T.);
#32988=ADVANCED_FACE('',(#5307),#1423,.T.);
#32989=ADVANCED_FACE('',(#5308),#1424,.T.);
#32990=ADVANCED_FACE('',(#5309),#1425,.T.);
#32991=ADVANCED_FACE('',(#5310),#1426,.T.);
#32992=ADVANCED_FACE('',(#5311),#1427,.T.);
#32993=ADVANCED_FACE('',(#5312),#1428,.T.);
#32994=ADVANCED_FACE('',(#5313),#1429,.T.);
#32995=ADVANCED_FACE('',(#5314),#1430,.T.);
#32996=ADVANCED_FACE('',(#5315),#1431,.T.);
#32997=ADVANCED_FACE('',(#5316),#1432,.T.);
#32998=ADVANCED_FACE('',(#5317),#1433,.T.);
#32999=ADVANCED_FACE('',(#5318),#1434,.T.);
#33000=ADVANCED_FACE('',(#5319),#1435,.T.);
#33001=ADVANCED_FACE('',(#5320),#1436,.T.);
#33002=ADVANCED_FACE('',(#5321),#1437,.T.);
#33003=ADVANCED_FACE('',(#5322),#1438,.T.);
#33004=ADVANCED_FACE('',(#5323),#1439,.T.);
#33005=ADVANCED_FACE('',(#5324),#1440,.T.);
#33006=ADVANCED_FACE('',(#5325),#1441,.T.);
#33007=ADVANCED_FACE('',(#5326),#1442,.T.);
#33008=ADVANCED_FACE('',(#5327),#1443,.T.);
#33009=ADVANCED_FACE('',(#5328),#1444,.T.);
#33010=ADVANCED_FACE('',(#5329),#1445,.T.);
#33011=ADVANCED_FACE('',(#5330),#1446,.T.);
#33012=ADVANCED_FACE('',(#5331),#1447,.T.);
#33013=ADVANCED_FACE('',(#5332),#1448,.T.);
#33014=ADVANCED_FACE('',(#5333),#1449,.T.);
#33015=ADVANCED_FACE('',(#5334),#1450,.T.);
#33016=ADVANCED_FACE('',(#5335),#1451,.T.);
#33017=ADVANCED_FACE('',(#5336),#1452,.T.);
#33018=ADVANCED_FACE('',(#5337),#1453,.T.);
#33019=ADVANCED_FACE('',(#5338),#1454,.T.);
#33020=ADVANCED_FACE('',(#5339),#1455,.T.);
#33021=ADVANCED_FACE('',(#5340),#1456,.T.);
#33022=ADVANCED_FACE('',(#5341),#1457,.T.);
#33023=ADVANCED_FACE('',(#5342),#1458,.T.);
#33024=ADVANCED_FACE('',(#5343),#1459,.T.);
#33025=ADVANCED_FACE('',(#5344),#1460,.T.);
#33026=ADVANCED_FACE('',(#5345),#1461,.T.);
#33027=ADVANCED_FACE('',(#5346),#1462,.T.);
#33028=ADVANCED_FACE('',(#5347),#1463,.T.);
#33029=ADVANCED_FACE('',(#5348),#1464,.T.);
#33030=ADVANCED_FACE('',(#5349),#1465,.T.);
#33031=ADVANCED_FACE('',(#5350),#1466,.T.);
#33032=ADVANCED_FACE('',(#5351),#1467,.T.);
#33033=ADVANCED_FACE('',(#5352),#1468,.T.);
#33034=ADVANCED_FACE('',(#5353),#1469,.T.);
#33035=ADVANCED_FACE('',(#5354),#1470,.T.);
#33036=ADVANCED_FACE('',(#5355),#1471,.T.);
#33037=ADVANCED_FACE('',(#5356),#1472,.T.);
#33038=ADVANCED_FACE('',(#5357),#1473,.T.);
#33039=ADVANCED_FACE('',(#5358),#1474,.T.);
#33040=ADVANCED_FACE('',(#5359),#1475,.T.);
#33041=ADVANCED_FACE('',(#5360),#1476,.T.);
#33042=ADVANCED_FACE('',(#5361),#1477,.T.);
#33043=ADVANCED_FACE('',(#5362),#1478,.T.);
#33044=ADVANCED_FACE('',(#5363),#1479,.T.);
#33045=ADVANCED_FACE('',(#5364),#1480,.T.);
#33046=ADVANCED_FACE('',(#5365),#1481,.T.);
#33047=ADVANCED_FACE('',(#5366),#1482,.T.);
#33048=ADVANCED_FACE('',(#5367),#1483,.T.);
#33049=ADVANCED_FACE('',(#5368),#1484,.T.);
#33050=ADVANCED_FACE('',(#5369),#1485,.T.);
#33051=ADVANCED_FACE('',(#5370),#1486,.T.);
#33052=ADVANCED_FACE('',(#5371),#1487,.T.);
#33053=ADVANCED_FACE('',(#5372),#1488,.T.);
#33054=ADVANCED_FACE('',(#5373),#1489,.T.);
#33055=ADVANCED_FACE('',(#5374),#1490,.T.);
#33056=ADVANCED_FACE('',(#5375),#1491,.T.);
#33057=ADVANCED_FACE('',(#5376),#1492,.T.);
#33058=ADVANCED_FACE('',(#5377),#1493,.T.);
#33059=ADVANCED_FACE('',(#5378),#1494,.T.);
#33060=ADVANCED_FACE('',(#5379),#1495,.T.);
#33061=ADVANCED_FACE('',(#5380),#1496,.T.);
#33062=ADVANCED_FACE('',(#5381),#1497,.T.);
#33063=ADVANCED_FACE('',(#5382),#1498,.T.);
#33064=ADVANCED_FACE('',(#5383),#1499,.T.);
#33065=ADVANCED_FACE('',(#5384),#1500,.T.);
#33066=ADVANCED_FACE('',(#5385),#1501,.T.);
#33067=ADVANCED_FACE('',(#5386),#1502,.T.);
#33068=ADVANCED_FACE('',(#5387),#1503,.T.);
#33069=ADVANCED_FACE('',(#5388),#1504,.T.);
#33070=ADVANCED_FACE('',(#5389),#1505,.T.);
#33071=ADVANCED_FACE('',(#5390),#1506,.T.);
#33072=ADVANCED_FACE('',(#5391),#1507,.T.);
#33073=ADVANCED_FACE('',(#5392),#1508,.T.);
#33074=ADVANCED_FACE('',(#5393),#1509,.T.);
#33075=ADVANCED_FACE('',(#5394),#1510,.T.);
#33076=ADVANCED_FACE('',(#5395),#1511,.T.);
#33077=ADVANCED_FACE('',(#5396),#1512,.T.);
#33078=ADVANCED_FACE('',(#5397),#1513,.T.);
#33079=ADVANCED_FACE('',(#5398),#1514,.T.);
#33080=ADVANCED_FACE('',(#5399),#1515,.T.);
#33081=ADVANCED_FACE('',(#5400),#1516,.T.);
#33082=ADVANCED_FACE('',(#5401),#1517,.T.);
#33083=ADVANCED_FACE('',(#5402),#1518,.T.);
#33084=ADVANCED_FACE('',(#5403),#1519,.T.);
#33085=ADVANCED_FACE('',(#5404),#1520,.T.);
#33086=ADVANCED_FACE('',(#5405),#1521,.T.);
#33087=ADVANCED_FACE('',(#5406),#1522,.T.);
#33088=ADVANCED_FACE('',(#5407),#1523,.T.);
#33089=ADVANCED_FACE('',(#5408),#1524,.T.);
#33090=ADVANCED_FACE('',(#5409),#1525,.T.);
#33091=ADVANCED_FACE('',(#5410),#1526,.T.);
#33092=ADVANCED_FACE('',(#5411),#1527,.T.);
#33093=ADVANCED_FACE('',(#5412),#1528,.T.);
#33094=ADVANCED_FACE('',(#5413),#1529,.T.);
#33095=ADVANCED_FACE('',(#5414),#1530,.T.);
#33096=ADVANCED_FACE('',(#5415),#1531,.T.);
#33097=ADVANCED_FACE('',(#5416),#1532,.T.);
#33098=ADVANCED_FACE('',(#5417),#1533,.T.);
#33099=ADVANCED_FACE('',(#5418),#1534,.T.);
#33100=ADVANCED_FACE('',(#5419),#1535,.T.);
#33101=ADVANCED_FACE('',(#5420),#1536,.T.);
#33102=ADVANCED_FACE('',(#5421),#1537,.T.);
#33103=ADVANCED_FACE('',(#5422),#1538,.T.);
#33104=ADVANCED_FACE('',(#5423),#1539,.T.);
#33105=ADVANCED_FACE('',(#5424),#1540,.T.);
#33106=ADVANCED_FACE('',(#5425),#1541,.T.);
#33107=ADVANCED_FACE('',(#5426),#1542,.T.);
#33108=ADVANCED_FACE('',(#5427),#1543,.T.);
#33109=ADVANCED_FACE('',(#5428),#1544,.T.);
#33110=ADVANCED_FACE('',(#5429),#1545,.T.);
#33111=ADVANCED_FACE('',(#5430),#1546,.T.);
#33112=ADVANCED_FACE('',(#5431),#1547,.T.);
#33113=ADVANCED_FACE('',(#5432),#1548,.T.);
#33114=ADVANCED_FACE('',(#5433),#1549,.T.);
#33115=ADVANCED_FACE('',(#5434),#1550,.T.);
#33116=ADVANCED_FACE('',(#5435),#1551,.T.);
#33117=ADVANCED_FACE('',(#5436),#1552,.T.);
#33118=ADVANCED_FACE('',(#5437),#1553,.T.);
#33119=ADVANCED_FACE('',(#5438),#1554,.T.);
#33120=ADVANCED_FACE('',(#5439),#1555,.T.);
#33121=ADVANCED_FACE('',(#5440),#1556,.T.);
#33122=ADVANCED_FACE('',(#5441),#1557,.T.);
#33123=ADVANCED_FACE('',(#5442),#1558,.T.);
#33124=ADVANCED_FACE('',(#5443),#1559,.T.);
#33125=ADVANCED_FACE('',(#5444),#1560,.T.);
#33126=ADVANCED_FACE('',(#5445),#1561,.T.);
#33127=ADVANCED_FACE('',(#5446),#1562,.T.);
#33128=ADVANCED_FACE('',(#5447),#1563,.T.);
#33129=ADVANCED_FACE('',(#5448),#1564,.T.);
#33130=ADVANCED_FACE('',(#5449),#1565,.T.);
#33131=ADVANCED_FACE('',(#5450),#1566,.T.);
#33132=ADVANCED_FACE('',(#5451),#1567,.T.);
#33133=ADVANCED_FACE('',(#5452),#1568,.T.);
#33134=ADVANCED_FACE('',(#5453),#1569,.T.);
#33135=ADVANCED_FACE('',(#5454),#1570,.T.);
#33136=ADVANCED_FACE('',(#5455),#1571,.T.);
#33137=ADVANCED_FACE('',(#5456),#1572,.T.);
#33138=ADVANCED_FACE('',(#5457),#1573,.T.);
#33139=ADVANCED_FACE('',(#5458),#1574,.T.);
#33140=ADVANCED_FACE('',(#5459),#1575,.T.);
#33141=ADVANCED_FACE('',(#5460),#1576,.T.);
#33142=ADVANCED_FACE('',(#5461),#1577,.T.);
#33143=ADVANCED_FACE('',(#5462),#1578,.T.);
#33144=ADVANCED_FACE('',(#5463),#1579,.T.);
#33145=ADVANCED_FACE('',(#5464),#1580,.T.);
#33146=ADVANCED_FACE('',(#5465),#1581,.T.);
#33147=ADVANCED_FACE('',(#5466),#1582,.T.);
#33148=ADVANCED_FACE('',(#5467),#1583,.T.);
#33149=ADVANCED_FACE('',(#5468),#1584,.T.);
#33150=ADVANCED_FACE('',(#5469),#1585,.T.);
#33151=ADVANCED_FACE('',(#5470),#1586,.T.);
#33152=ADVANCED_FACE('',(#5471),#1587,.T.);
#33153=ADVANCED_FACE('',(#5472),#1588,.T.);
#33154=ADVANCED_FACE('',(#5473,#2133),#31662,.T.);
#33155=ADVANCED_FACE('',(#5474),#908,.T.);
#33156=ADVANCED_FACE('',(#5475),#1589,.T.);
#33157=ADVANCED_FACE('',(#5476,#2134),#31663,.T.);
#33158=ADVANCED_FACE('',(#5477),#909,.F.);
#33159=ADVANCED_FACE('',(#5478,#2135),#31664,.F.);
#33160=ADVANCED_FACE('',(#5479),#31665,.F.);
#33161=ADVANCED_FACE('',(#5480),#31666,.F.);
#33162=ADVANCED_FACE('',(#5481),#1590,.F.);
#33163=ADVANCED_FACE('',(#5482),#31667,.F.);
#33164=ADVANCED_FACE('',(#5483),#1591,.T.);
#33165=ADVANCED_FACE('',(#5484),#1592,.T.);
#33166=ADVANCED_FACE('',(#5485),#1593,.T.);
#33167=ADVANCED_FACE('',(#5486),#1594,.T.);
#33168=ADVANCED_FACE('',(#5487),#1595,.T.);
#33169=ADVANCED_FACE('',(#5488),#1596,.T.);
#33170=ADVANCED_FACE('',(#5489),#1597,.T.);
#33171=ADVANCED_FACE('',(#5490),#1598,.T.);
#33172=ADVANCED_FACE('',(#5491),#1599,.T.);
#33173=ADVANCED_FACE('',(#5492),#1600,.T.);
#33174=ADVANCED_FACE('',(#5493),#1601,.T.);
#33175=ADVANCED_FACE('',(#5494),#1602,.T.);
#33176=ADVANCED_FACE('',(#5495),#1603,.T.);
#33177=ADVANCED_FACE('',(#5496),#1604,.T.);
#33178=ADVANCED_FACE('',(#5497),#1605,.T.);
#33179=ADVANCED_FACE('',(#5498),#1606,.T.);
#33180=ADVANCED_FACE('',(#5499),#1607,.T.);
#33181=ADVANCED_FACE('',(#5500),#1608,.T.);
#33182=ADVANCED_FACE('',(#5501),#1609,.T.);
#33183=ADVANCED_FACE('',(#5502),#1610,.T.);
#33184=ADVANCED_FACE('',(#5503),#1611,.T.);
#33185=ADVANCED_FACE('',(#5504),#1612,.T.);
#33186=ADVANCED_FACE('',(#5505),#1613,.T.);
#33187=ADVANCED_FACE('',(#5506),#1614,.T.);
#33188=ADVANCED_FACE('',(#5507),#1615,.T.);
#33189=ADVANCED_FACE('',(#5508),#1616,.T.);
#33190=ADVANCED_FACE('',(#5509),#1617,.T.);
#33191=ADVANCED_FACE('',(#5510),#1618,.T.);
#33192=ADVANCED_FACE('',(#5511),#1619,.T.);
#33193=ADVANCED_FACE('',(#5512),#1620,.T.);
#33194=ADVANCED_FACE('',(#5513),#1621,.T.);
#33195=ADVANCED_FACE('',(#5514),#1622,.T.);
#33196=ADVANCED_FACE('',(#5515),#1623,.T.);
#33197=ADVANCED_FACE('',(#5516),#1624,.T.);
#33198=ADVANCED_FACE('',(#5517),#1625,.T.);
#33199=ADVANCED_FACE('',(#5518),#1626,.T.);
#33200=ADVANCED_FACE('',(#5519),#1627,.T.);
#33201=ADVANCED_FACE('',(#5520),#1628,.T.);
#33202=ADVANCED_FACE('',(#5521),#1629,.T.);
#33203=ADVANCED_FACE('',(#5522),#1630,.T.);
#33204=ADVANCED_FACE('',(#5523),#1631,.T.);
#33205=ADVANCED_FACE('',(#5524),#1632,.T.);
#33206=ADVANCED_FACE('',(#5525),#1633,.T.);
#33207=ADVANCED_FACE('',(#5526),#1634,.T.);
#33208=ADVANCED_FACE('',(#5527),#1635,.T.);
#33209=ADVANCED_FACE('',(#5528),#1636,.T.);
#33210=ADVANCED_FACE('',(#5529),#1637,.T.);
#33211=ADVANCED_FACE('',(#5530),#1638,.T.);
#33212=ADVANCED_FACE('',(#5531),#1639,.T.);
#33213=ADVANCED_FACE('',(#5532),#1640,.T.);
#33214=ADVANCED_FACE('',(#5533),#1641,.T.);
#33215=ADVANCED_FACE('',(#5534),#1642,.T.);
#33216=ADVANCED_FACE('',(#5535),#1643,.T.);
#33217=ADVANCED_FACE('',(#5536),#1644,.T.);
#33218=ADVANCED_FACE('',(#5537),#1645,.T.);
#33219=ADVANCED_FACE('',(#5538),#1646,.T.);
#33220=ADVANCED_FACE('',(#5539),#1647,.T.);
#33221=ADVANCED_FACE('',(#5540),#1648,.T.);
#33222=ADVANCED_FACE('',(#5541),#1649,.T.);
#33223=ADVANCED_FACE('',(#5542),#1650,.T.);
#33224=ADVANCED_FACE('',(#5543),#1651,.T.);
#33225=ADVANCED_FACE('',(#5544),#1652,.T.);
#33226=ADVANCED_FACE('',(#5545),#1653,.T.);
#33227=ADVANCED_FACE('',(#5546),#1654,.T.);
#33228=ADVANCED_FACE('',(#5547),#1655,.T.);
#33229=ADVANCED_FACE('',(#5548),#1656,.T.);
#33230=ADVANCED_FACE('',(#5549),#1657,.T.);
#33231=ADVANCED_FACE('',(#5550),#1658,.T.);
#33232=ADVANCED_FACE('',(#5551),#1659,.T.);
#33233=ADVANCED_FACE('',(#5552),#1660,.T.);
#33234=ADVANCED_FACE('',(#5553),#1661,.T.);
#33235=ADVANCED_FACE('',(#5554),#1662,.T.);
#33236=ADVANCED_FACE('',(#5555),#1663,.T.);
#33237=ADVANCED_FACE('',(#5556),#1664,.T.);
#33238=ADVANCED_FACE('',(#5557),#1665,.T.);
#33239=ADVANCED_FACE('',(#5558),#1666,.T.);
#33240=ADVANCED_FACE('',(#5559),#1667,.T.);
#33241=ADVANCED_FACE('',(#5560),#1668,.T.);
#33242=ADVANCED_FACE('',(#5561),#1669,.T.);
#33243=ADVANCED_FACE('',(#5562),#1670,.T.);
#33244=ADVANCED_FACE('',(#5563),#1671,.T.);
#33245=ADVANCED_FACE('',(#5564),#1672,.T.);
#33246=ADVANCED_FACE('',(#5565),#1673,.T.);
#33247=ADVANCED_FACE('',(#5566),#1674,.T.);
#33248=ADVANCED_FACE('',(#5567),#1675,.T.);
#33249=ADVANCED_FACE('',(#5568),#1676,.T.);
#33250=ADVANCED_FACE('',(#5569),#1677,.T.);
#33251=ADVANCED_FACE('',(#5570),#1678,.T.);
#33252=ADVANCED_FACE('',(#5571),#1679,.T.);
#33253=ADVANCED_FACE('',(#5572),#1680,.T.);
#33254=ADVANCED_FACE('',(#5573),#1681,.T.);
#33255=ADVANCED_FACE('',(#5574),#1682,.T.);
#33256=ADVANCED_FACE('',(#5575),#1683,.T.);
#33257=ADVANCED_FACE('',(#5576),#1684,.T.);
#33258=ADVANCED_FACE('',(#5577),#1685,.T.);
#33259=ADVANCED_FACE('',(#5578),#1686,.T.);
#33260=ADVANCED_FACE('',(#5579),#1687,.T.);
#33261=ADVANCED_FACE('',(#5580),#1688,.T.);
#33262=ADVANCED_FACE('',(#5581),#1689,.T.);
#33263=ADVANCED_FACE('',(#5582),#1690,.T.);
#33264=ADVANCED_FACE('',(#5583),#1691,.T.);
#33265=ADVANCED_FACE('',(#5584),#1692,.T.);
#33266=ADVANCED_FACE('',(#5585),#1693,.T.);
#33267=ADVANCED_FACE('',(#5586),#1694,.T.);
#33268=ADVANCED_FACE('',(#5587),#1695,.T.);
#33269=ADVANCED_FACE('',(#5588),#1696,.T.);
#33270=ADVANCED_FACE('',(#5589),#1697,.T.);
#33271=ADVANCED_FACE('',(#5590),#1698,.T.);
#33272=ADVANCED_FACE('',(#5591),#1699,.T.);
#33273=ADVANCED_FACE('',(#5592),#1700,.T.);
#33274=ADVANCED_FACE('',(#5593),#1701,.T.);
#33275=ADVANCED_FACE('',(#5594),#1702,.T.);
#33276=ADVANCED_FACE('',(#5595),#1703,.T.);
#33277=ADVANCED_FACE('',(#5596),#1704,.T.);
#33278=ADVANCED_FACE('',(#5597),#1705,.T.);
#33279=ADVANCED_FACE('',(#5598),#1706,.T.);
#33280=ADVANCED_FACE('',(#5599),#1707,.T.);
#33281=ADVANCED_FACE('',(#5600),#1708,.T.);
#33282=ADVANCED_FACE('',(#5601),#1709,.T.);
#33283=ADVANCED_FACE('',(#5602),#1710,.T.);
#33284=ADVANCED_FACE('',(#5603),#1711,.T.);
#33285=ADVANCED_FACE('',(#5604),#1712,.T.);
#33286=ADVANCED_FACE('',(#5605),#1713,.T.);
#33287=ADVANCED_FACE('',(#5606),#1714,.T.);
#33288=ADVANCED_FACE('',(#5607),#1715,.T.);
#33289=ADVANCED_FACE('',(#5608),#1716,.T.);
#33290=ADVANCED_FACE('',(#5609),#1717,.T.);
#33291=ADVANCED_FACE('',(#5610),#1718,.T.);
#33292=ADVANCED_FACE('',(#5611),#1719,.T.);
#33293=ADVANCED_FACE('',(#5612),#1720,.T.);
#33294=ADVANCED_FACE('',(#5613),#1721,.T.);
#33295=ADVANCED_FACE('',(#5614),#1722,.T.);
#33296=ADVANCED_FACE('',(#5615),#1723,.T.);
#33297=ADVANCED_FACE('',(#5616),#1724,.T.);
#33298=ADVANCED_FACE('',(#5617),#1725,.T.);
#33299=ADVANCED_FACE('',(#5618),#1726,.T.);
#33300=ADVANCED_FACE('',(#5619),#1727,.T.);
#33301=ADVANCED_FACE('',(#5620),#1728,.T.);
#33302=ADVANCED_FACE('',(#5621),#1729,.T.);
#33303=ADVANCED_FACE('',(#5622),#1730,.T.);
#33304=ADVANCED_FACE('',(#5623),#1731,.T.);
#33305=ADVANCED_FACE('',(#5624),#1732,.T.);
#33306=ADVANCED_FACE('',(#5625),#1733,.T.);
#33307=ADVANCED_FACE('',(#5626),#1734,.T.);
#33308=ADVANCED_FACE('',(#5627),#1735,.T.);
#33309=ADVANCED_FACE('',(#5628),#1736,.T.);
#33310=ADVANCED_FACE('',(#5629),#1737,.T.);
#33311=ADVANCED_FACE('',(#5630),#1738,.T.);
#33312=ADVANCED_FACE('',(#5631),#1739,.T.);
#33313=ADVANCED_FACE('',(#5632),#1740,.T.);
#33314=ADVANCED_FACE('',(#5633),#1741,.T.);
#33315=ADVANCED_FACE('',(#5634),#1742,.T.);
#33316=ADVANCED_FACE('',(#5635),#1743,.T.);
#33317=ADVANCED_FACE('',(#5636),#1744,.T.);
#33318=ADVANCED_FACE('',(#5637),#1745,.T.);
#33319=ADVANCED_FACE('',(#5638),#1746,.T.);
#33320=ADVANCED_FACE('',(#5639),#1747,.T.);
#33321=ADVANCED_FACE('',(#5640),#1748,.T.);
#33322=ADVANCED_FACE('',(#5641),#1749,.T.);
#33323=ADVANCED_FACE('',(#5642),#1750,.T.);
#33324=ADVANCED_FACE('',(#5643,#2136),#31668,.T.);
#33325=ADVANCED_FACE('',(#5644),#616,.T.);
#33326=ADVANCED_FACE('',(#5645),#31669,.T.);
#33327=ADVANCED_FACE('',(#5646),#617,.F.);
#33328=ADVANCED_FACE('',(#5647),#1751,.F.);
#33329=ADVANCED_FACE('',(#5648),#1752,.T.);
#33330=ADVANCED_FACE('',(#5649,#2137),#31670,.T.);
#33331=ADVANCED_FACE('',(#5650,#2138),#31671,.T.);
#33332=ADVANCED_FACE('',(#5651),#1753,.F.);
#33333=ADVANCED_FACE('',(#5652),#618,.T.);
#33334=ADVANCED_FACE('',(#5653),#31672,.T.);
#33335=ADVANCED_FACE('',(#5654),#619,.F.);
#33336=ADVANCED_FACE('',(#5655),#1754,.F.);
#33337=ADVANCED_FACE('',(#5656),#1755,.T.);
#33338=ADVANCED_FACE('',(#5657,#2139),#31673,.T.);
#33339=ADVANCED_FACE('',(#5658,#2140),#31674,.T.);
#33340=ADVANCED_FACE('',(#5659),#1756,.F.);
#33341=ADVANCED_FACE('',(#5660),#620,.T.);
#33342=ADVANCED_FACE('',(#5661),#31675,.T.);
#33343=ADVANCED_FACE('',(#5662),#1757,.F.);
#33344=ADVANCED_FACE('',(#5663),#621,.F.);
#33345=ADVANCED_FACE('',(#5664),#1758,.T.);
#33346=ADVANCED_FACE('',(#5665,#2141),#31676,.T.);
#33347=ADVANCED_FACE('',(#5666),#1759,.F.);
#33348=ADVANCED_FACE('',(#5667,#2142),#31677,.T.);
#33349=ADVANCED_FACE('',(#5668),#1760,.T.);
#33350=ADVANCED_FACE('',(#5669,#2143),#31678,.T.);
#33351=ADVANCED_FACE('',(#5670),#1761,.F.);
#33352=ADVANCED_FACE('',(#5671,#2144),#31679,.T.);
#33353=ADVANCED_FACE('',(#5672),#622,.T.);
#33354=ADVANCED_FACE('',(#5673),#31680,.T.);
#33355=ADVANCED_FACE('',(#5674),#1762,.F.);
#33356=ADVANCED_FACE('',(#5675),#623,.F.);
#33357=ADVANCED_FACE('',(#5676),#1763,.T.);
#33358=ADVANCED_FACE('',(#5677,#2145),#31681,.T.);
#33359=ADVANCED_FACE('',(#5678),#1764,.F.);
#33360=ADVANCED_FACE('',(#5679,#2146),#31682,.T.);
#33361=ADVANCED_FACE('',(#5680),#624,.T.);
#33362=ADVANCED_FACE('',(#5681),#31683,.T.);
#33363=ADVANCED_FACE('',(#5682),#1765,.F.);
#33364=ADVANCED_FACE('',(#5683),#625,.F.);
#33365=ADVANCED_FACE('',(#5684),#31684,.T.);
#33366=ADVANCED_FACE('',(#5685),#626,.T.);
#33367=ADVANCED_FACE('',(#5686),#31685,.T.);
#33368=ADVANCED_FACE('',(#5687),#627,.T.);
#33369=ADVANCED_FACE('',(#5688),#31686,.T.);
#33370=ADVANCED_FACE('',(#5689),#31687,.T.);
#33371=ADVANCED_FACE('',(#5690),#31688,.T.);
#33372=ADVANCED_FACE('',(#5691),#31689,.T.);
#33373=ADVANCED_FACE('',(#5692),#31690,.T.);
#33374=ADVANCED_FACE('',(#5693,#2147),#31691,.T.);
#33375=ADVANCED_FACE('',(#5694),#1766,.F.);
#33376=ADVANCED_FACE('',(#5695),#31692,.T.);
#33377=ADVANCED_FACE('',(#5696,#2148,#2149,#2150,#2151),#31693,.T.);
#33378=ADVANCED_FACE('',(#5697),#1767,.F.);
#33379=ADVANCED_FACE('',(#5698),#31694,.T.);
#33380=ADVANCED_FACE('',(#5699),#31695,.T.);
#33381=ADVANCED_FACE('',(#5700),#1768,.F.);
#33382=ADVANCED_FACE('',(#5701),#31696,.T.);
#33383=ADVANCED_FACE('',(#5702),#31697,.T.);
#33384=ADVANCED_FACE('',(#5703),#1769,.F.);
#33385=ADVANCED_FACE('',(#5704),#31698,.T.);
#33386=ADVANCED_FACE('',(#5705),#31699,.T.);
#33387=ADVANCED_FACE('',(#5706),#1770,.F.);
#33388=ADVANCED_FACE('',(#5707),#1771,.T.);
#33389=ADVANCED_FACE('',(#5708),#31700,.T.);
#33390=ADVANCED_FACE('',(#5709),#31701,.T.);
#33391=ADVANCED_FACE('',(#5710),#31702,.T.);
#33392=ADVANCED_FACE('',(#5711),#31703,.T.);
#33393=ADVANCED_FACE('',(#5712),#31704,.T.);
#33394=ADVANCED_FACE('',(#5713),#31705,.T.);
#33395=ADVANCED_FACE('',(#5714),#628,.T.);
#33396=ADVANCED_FACE('',(#5715,#2152),#31706,.T.);
#33397=ADVANCED_FACE('',(#5716),#1772,.F.);
#33398=ADVANCED_FACE('',(#5717),#1773,.F.);
#33399=ADVANCED_FACE('',(#5718),#1774,.F.);
#33400=ADVANCED_FACE('',(#5719),#1775,.F.);
#33401=ADVANCED_FACE('',(#5720),#31707,.T.);
#33402=ADVANCED_FACE('',(#5721),#31708,.T.);
#33403=ADVANCED_FACE('',(#5722),#31709,.T.);
#33404=ADVANCED_FACE('',(#5723,#2153),#31710,.T.);
#33405=ADVANCED_FACE('',(#5724),#31711,.T.);
#33406=ADVANCED_FACE('',(#5725),#1776,.T.);
#33407=ADVANCED_FACE('',(#5726),#31712,.T.);
#33408=ADVANCED_FACE('',(#5727),#31713,.T.);
#33409=ADVANCED_FACE('',(#5728),#31714,.T.);
#33410=ADVANCED_FACE('',(#5729),#31715,.T.);
#33411=ADVANCED_FACE('',(#5730),#31716,.T.);
#33412=ADVANCED_FACE('',(#5731),#629,.T.);
#33413=ADVANCED_FACE('',(#5732),#630,.T.);
#33414=ADVANCED_FACE('',(#5733),#631,.T.);
#33415=ADVANCED_FACE('',(#5734),#632,.T.);
#33416=ADVANCED_FACE('',(#5735),#633,.T.);
#33417=ADVANCED_FACE('',(#5736),#31717,.T.);
#33418=ADVANCED_FACE('',(#5737),#31718,.T.);
#33419=ADVANCED_FACE('',(#5738),#634,.T.);
#33420=ADVANCED_FACE('',(#5739),#31719,.T.);
#33421=ADVANCED_FACE('',(#5740),#31720,.T.);
#33422=ADVANCED_FACE('',(#5741),#31721,.T.);
#33423=ADVANCED_FACE('',(#5742),#31722,.T.);
#33424=ADVANCED_FACE('',(#5743),#31723,.T.);
#33425=ADVANCED_FACE('',(#5744),#635,.T.);
#33426=ADVANCED_FACE('',(#5745),#636,.T.);
#33427=ADVANCED_FACE('',(#5746),#637,.T.);
#33428=ADVANCED_FACE('',(#5747),#638,.T.);
#33429=ADVANCED_FACE('',(#5748),#639,.T.);
#33430=ADVANCED_FACE('',(#5749),#31724,.T.);
#33431=ADVANCED_FACE('',(#5750),#31725,.T.);
#33432=ADVANCED_FACE('',(#5751),#640,.T.);
#33433=ADVANCED_FACE('',(#5752),#31726,.T.);
#33434=ADVANCED_FACE('',(#5753),#31727,.T.);
#33435=ADVANCED_FACE('',(#5754),#31728,.T.);
#33436=ADVANCED_FACE('',(#5755),#31729,.T.);
#33437=ADVANCED_FACE('',(#5756),#31730,.T.);
#33438=ADVANCED_FACE('',(#5757),#31731,.T.);
#33439=ADVANCED_FACE('',(#5758),#31732,.T.);
#33440=ADVANCED_FACE('',(#5759),#31733,.T.);
#33441=ADVANCED_FACE('',(#5760),#31734,.T.);
#33442=ADVANCED_FACE('',(#5761),#31735,.T.);
#33443=ADVANCED_FACE('',(#5762),#641,.T.);
#33444=ADVANCED_FACE('',(#5763),#642,.T.);
#33445=ADVANCED_FACE('',(#5764),#643,.T.);
#33446=ADVANCED_FACE('',(#5765),#31736,.T.);
#33447=ADVANCED_FACE('',(#5766),#31737,.T.);
#33448=ADVANCED_FACE('',(#5767),#31738,.T.);
#33449=ADVANCED_FACE('',(#5768),#31739,.T.);
#33450=ADVANCED_FACE('',(#5769),#31740,.T.);
#33451=ADVANCED_FACE('',(#5770),#31741,.T.);
#33452=ADVANCED_FACE('',(#5771),#31742,.T.);
#33453=ADVANCED_FACE('',(#5772),#644,.T.);
#33454=ADVANCED_FACE('',(#5773,#2154),#31743,.T.);
#33455=ADVANCED_FACE('',(#5774),#31744,.T.);
#33456=ADVANCED_FACE('',(#5775),#31745,.T.);
#33457=ADVANCED_FACE('',(#5776),#31746,.T.);
#33458=ADVANCED_FACE('',(#5777),#31747,.T.);
#33459=ADVANCED_FACE('',(#5778),#31748,.T.);
#33460=ADVANCED_FACE('',(#5779),#31749,.T.);
#33461=ADVANCED_FACE('',(#5780),#31750,.T.);
#33462=ADVANCED_FACE('',(#5781),#645,.T.);
#33463=ADVANCED_FACE('',(#5782,#2155),#31751,.T.);
#33464=ADVANCED_FACE('',(#5783),#31752,.T.);
#33465=ADVANCED_FACE('',(#5784),#31753,.T.);
#33466=ADVANCED_FACE('',(#5785),#31754,.T.);
#33467=ADVANCED_FACE('',(#5786,#2156),#31755,.T.);
#33468=ADVANCED_FACE('',(#5787),#646,.T.);
#33469=ADVANCED_FACE('',(#5788),#647,.F.);
#33470=ADVANCED_FACE('',(#5789),#1777,.F.);
#33471=ADVANCED_FACE('',(#5790),#648,.F.);
#33472=ADVANCED_FACE('',(#5791),#649,.F.);
#33473=ADVANCED_FACE('',(#5792),#1778,.F.);
#33474=ADVANCED_FACE('',(#5793),#650,.F.);
#33475=ADVANCED_FACE('',(#5794),#651,.F.);
#33476=ADVANCED_FACE('',(#5795),#1779,.F.);
#33477=ADVANCED_FACE('',(#5796),#652,.F.);
#33478=ADVANCED_FACE('',(#5797),#653,.F.);
#33479=ADVANCED_FACE('',(#5798),#1780,.F.);
#33480=ADVANCED_FACE('',(#5799),#654,.F.);
#33481=ADVANCED_FACE('',(#5800),#655,.F.);
#33482=ADVANCED_FACE('',(#5801),#1781,.F.);
#33483=ADVANCED_FACE('',(#5802),#656,.F.);
#33484=ADVANCED_FACE('',(#5803),#657,.F.);
#33485=ADVANCED_FACE('',(#5804),#1782,.F.);
#33486=ADVANCED_FACE('',(#5805),#658,.F.);
#33487=ADVANCED_FACE('',(#5806),#659,.F.);
#33488=ADVANCED_FACE('',(#5807),#1783,.F.);
#33489=ADVANCED_FACE('',(#5808),#660,.F.);
#33490=ADVANCED_FACE('',(#5809),#661,.F.);
#33491=ADVANCED_FACE('',(#5810),#662,.F.);
#33492=ADVANCED_FACE('',(#5811),#663,.F.);
#33493=ADVANCED_FACE('',(#5812),#664,.F.);
#33494=ADVANCED_FACE('',(#5813),#665,.F.);
#33495=ADVANCED_FACE('',(#5814),#666,.F.);
#33496=ADVANCED_FACE('',(#5815),#667,.F.);
#33497=ADVANCED_FACE('',(#5816),#668,.F.);
#33498=ADVANCED_FACE('',(#5817),#31756,.T.);
#33499=ADVANCED_FACE('',(#5818),#31757,.T.);
#33500=ADVANCED_FACE('',(#5819),#31758,.T.);
#33501=ADVANCED_FACE('',(#5820),#31759,.T.);
#33502=ADVANCED_FACE('',(#5821),#31760,.T.);
#33503=ADVANCED_FACE('',(#5822),#31761,.T.);
#33504=ADVANCED_FACE('',(#5823),#31762,.T.);
#33505=ADVANCED_FACE('',(#5824),#31763,.T.);
#33506=ADVANCED_FACE('',(#5825,#2157),#31764,.T.);
#33507=ADVANCED_FACE('',(#5826,#2158),#31765,.T.);
#33508=ADVANCED_FACE('',(#5827),#1784,.F.);
#33509=ADVANCED_FACE('',(#5828),#669,.F.);
#33510=ADVANCED_FACE('',(#5829,#2159,#2160,#2161,#2162),#31766,.T.);
#33511=ADVANCED_FACE('',(#5830),#31767,.T.);
#33512=ADVANCED_FACE('',(#5831),#31768,.T.);
#33513=ADVANCED_FACE('',(#5832),#31769,.T.);
#33514=ADVANCED_FACE('',(#5833),#31770,.T.);
#33515=ADVANCED_FACE('',(#5834),#31771,.T.);
#33516=ADVANCED_FACE('',(#5835),#31772,.T.);
#33517=ADVANCED_FACE('',(#5836),#31773,.T.);
#33518=ADVANCED_FACE('',(#5837,#2163,#2164,#2165,#2166,#2167),#31774,.T.);
#33519=ADVANCED_FACE('',(#5838),#31775,.T.);
#33520=ADVANCED_FACE('',(#5839),#31776,.T.);
#33521=ADVANCED_FACE('',(#5840),#670,.T.);
#33522=ADVANCED_FACE('',(#5841),#671,.F.);
#33523=ADVANCED_FACE('',(#5842),#1785,.F.);
#33524=ADVANCED_FACE('',(#5843),#672,.F.);
#33525=ADVANCED_FACE('',(#5844),#1786,.F.);
#33526=ADVANCED_FACE('',(#5845),#673,.T.);
#33527=ADVANCED_FACE('',(#5846),#674,.T.);
#33528=ADVANCED_FACE('',(#5847),#1787,.F.);
#33529=ADVANCED_FACE('',(#5848),#675,.F.);
#33530=ADVANCED_FACE('',(#5849,#2168,#2169,#2170,#2171,#2172),#31777,.T.);
#33531=ADVANCED_FACE('',(#5850,#2173),#31778,.T.);
#33532=ADVANCED_FACE('',(#5851),#1788,.T.);
#33533=ADVANCED_FACE('',(#5852,#2174),#31779,.T.);
#33534=ADVANCED_FACE('',(#5853),#1789,.F.);
#33535=ADVANCED_FACE('',(#5854),#676,.T.);
#33536=ADVANCED_FACE('',(#5855,#2175),#31780,.T.);
#33537=ADVANCED_FACE('',(#5856),#677,.F.);
#33538=ADVANCED_FACE('',(#5857,#2176),#31781,.T.);
#33539=ADVANCED_FACE('',(#5858,#2177,#2178),#1790,.F.);
#33540=ADVANCED_FACE('',(#5859),#1791,.F.);
#33541=ADVANCED_FACE('',(#5860,#2179,#2180),#31782,.T.);
#33542=ADVANCED_FACE('',(#5861),#31783,.T.);
#33543=ADVANCED_FACE('',(#5862),#31784,.T.);
#33544=ADVANCED_FACE('',(#5863),#31785,.T.);
#33545=ADVANCED_FACE('',(#5864),#31786,.T.);
#33546=ADVANCED_FACE('',(#5865),#31787,.T.);
#33547=ADVANCED_FACE('',(#5866),#31788,.T.);
#33548=ADVANCED_FACE('',(#5867),#31789,.T.);
#33549=ADVANCED_FACE('',(#5868),#31790,.T.);
#33550=ADVANCED_FACE('',(#5869),#31791,.T.);
#33551=ADVANCED_FACE('',(#5870),#31792,.T.);
#33552=ADVANCED_FACE('',(#5871),#31793,.T.);
#33553=ADVANCED_FACE('',(#5872),#31794,.T.);
#33554=ADVANCED_FACE('',(#5873),#31795,.T.);
#33555=ADVANCED_FACE('',(#5874),#31796,.T.);
#33556=ADVANCED_FACE('',(#5875,#2181),#31797,.T.);
#33557=ADVANCED_FACE('',(#5876),#678,.T.);
#33558=ADVANCED_FACE('',(#5877),#1792,.T.);
#33559=ADVANCED_FACE('',(#5878),#679,.T.);
#33560=ADVANCED_FACE('',(#5879),#31798,.T.);
#33561=ADVANCED_FACE('',(#5880,#2182),#31799,.T.);
#33562=ADVANCED_FACE('',(#5881),#680,.T.);
#33563=ADVANCED_FACE('',(#5882),#31800,.T.);
#33564=ADVANCED_FACE('',(#5883),#31801,.T.);
#33565=ADVANCED_FACE('',(#5884),#31802,.T.);
#33566=ADVANCED_FACE('',(#5885),#31803,.T.);
#33567=ADVANCED_FACE('',(#5886),#31804,.T.);
#33568=ADVANCED_FACE('',(#5887),#31805,.T.);
#33569=ADVANCED_FACE('',(#5888),#31806,.T.);
#33570=ADVANCED_FACE('',(#5889),#31807,.T.);
#33571=ADVANCED_FACE('',(#5890),#31808,.T.);
#33572=ADVANCED_FACE('',(#5891),#31809,.T.);
#33573=ADVANCED_FACE('',(#5892),#31810,.T.);
#33574=ADVANCED_FACE('',(#5893),#31811,.T.);
#33575=ADVANCED_FACE('',(#5894),#31812,.T.);
#33576=ADVANCED_FACE('',(#5895),#31813,.T.);
#33577=ADVANCED_FACE('',(#5896,#2183),#31814,.T.);
#33578=ADVANCED_FACE('',(#5897),#681,.T.);
#33579=ADVANCED_FACE('',(#5898),#1793,.T.);
#33580=ADVANCED_FACE('',(#5899),#682,.T.);
#33581=ADVANCED_FACE('',(#5900),#31815,.T.);
#33582=ADVANCED_FACE('',(#5901,#2184),#31816,.T.);
#33583=ADVANCED_FACE('',(#5902),#683,.T.);
#33584=ADVANCED_FACE('',(#5903),#1794,.T.);
#33585=ADVANCED_FACE('',(#5904),#684,.T.);
#33586=ADVANCED_FACE('',(#5905),#31817,.T.);
#33587=ADVANCED_FACE('',(#5906),#1795,.F.);
#33588=ADVANCED_FACE('',(#5907),#1796,.F.);
#33589=ADVANCED_FACE('',(#5908),#31818,.T.);
#33590=ADVANCED_FACE('',(#5909),#685,.T.);
#33591=ADVANCED_FACE('',(#5910),#1797,.T.);
#33592=ADVANCED_FACE('',(#5911,#2185,#2186),#1798,.T.);
#33593=ADVANCED_FACE('',(#5912),#686,.T.);
#33594=ADVANCED_FACE('',(#5913),#31819,.T.);
#33595=ADVANCED_FACE('',(#5914),#687,.F.);
#33596=ADVANCED_FACE('',(#5915),#31820,.T.);
#33597=ADVANCED_FACE('',(#5916,#2187,#2188),#1799,.T.);
#33598=ADVANCED_FACE('',(#5917,#2189),#31821,.T.);
#33599=ADVANCED_FACE('',(#5918,#2190),#31822,.T.);
#33600=ADVANCED_FACE('',(#5919),#1800,.T.);
#33601=ADVANCED_FACE('',(#5920),#1801,.T.);
#33602=ADVANCED_FACE('',(#5921,#2191),#31823,.T.);
#33603=ADVANCED_FACE('',(#5922,#2192),#31824,.T.);
#33604=ADVANCED_FACE('',(#5923),#1802,.T.);
#33605=ADVANCED_FACE('',(#5924),#31825,.T.);
#33606=ADVANCED_FACE('',(#5925),#688,.T.);
#33607=ADVANCED_FACE('',(#5926),#31826,.T.);
#33608=ADVANCED_FACE('',(#5927),#31827,.T.);
#33609=ADVANCED_FACE('',(#5928),#689,.T.);
#33610=ADVANCED_FACE('',(#5929),#690,.T.);
#33611=ADVANCED_FACE('',(#5930),#691,.T.);
#33612=ADVANCED_FACE('',(#5931),#692,.T.);
#33613=ADVANCED_FACE('',(#5932),#693,.T.);
#33614=ADVANCED_FACE('',(#5933),#31828,.T.);
#33615=ADVANCED_FACE('',(#5934),#31829,.T.);
#33616=ADVANCED_FACE('',(#5935),#31830,.T.);
#33617=ADVANCED_FACE('',(#5936),#31831,.T.);
#33618=ADVANCED_FACE('',(#5937),#31832,.T.);
#33619=ADVANCED_FACE('',(#5938),#694,.T.);
#33620=ADVANCED_FACE('',(#5939),#31833,.T.);
#33621=ADVANCED_FACE('',(#5940),#31834,.T.);
#33622=ADVANCED_FACE('',(#5941),#695,.T.);
#33623=ADVANCED_FACE('',(#5942),#696,.T.);
#33624=ADVANCED_FACE('',(#5943),#697,.T.);
#33625=ADVANCED_FACE('',(#5944),#698,.T.);
#33626=ADVANCED_FACE('',(#5945),#699,.T.);
#33627=ADVANCED_FACE('',(#5946),#31835,.T.);
#33628=ADVANCED_FACE('',(#5947),#31836,.T.);
#33629=ADVANCED_FACE('',(#5948),#31837,.T.);
#33630=ADVANCED_FACE('',(#5949),#31838,.T.);
#33631=ADVANCED_FACE('',(#5950,#2193),#31839,.T.);
#33632=ADVANCED_FACE('',(#5951,#2194),#31840,.T.);
#33633=ADVANCED_FACE('',(#5952,#2195),#31841,.T.);
#33634=ADVANCED_FACE('',(#5953),#1803,.F.);
#33635=ADVANCED_FACE('',(#5954),#1804,.F.);
#33636=ADVANCED_FACE('',(#5955),#1805,.F.);
#33637=ADVANCED_FACE('',(#5956),#1806,.F.);
#33638=ADVANCED_FACE('',(#5957),#1807,.F.);
#33639=ADVANCED_FACE('',(#5958),#1808,.F.);
#33640=ADVANCED_FACE('',(#5959),#1809,.F.);
#33641=ADVANCED_FACE('',(#5960),#31842,.T.);
#33642=ADVANCED_FACE('',(#5961),#31843,.T.);
#33643=ADVANCED_FACE('',(#5962),#1810,.F.);
#33644=ADVANCED_FACE('',(#5963),#1811,.F.);
#33645=ADVANCED_FACE('',(#5964),#1812,.F.);
#33646=ADVANCED_FACE('',(#5965),#31844,.T.);
#33647=ADVANCED_FACE('',(#5966),#1813,.F.);
#33648=ADVANCED_FACE('',(#5967),#1814,.T.);
#33649=ADVANCED_FACE('',(#5968),#1815,.F.);
#33650=ADVANCED_FACE('',(#5969),#31845,.T.);
#33651=ADVANCED_FACE('',(#5970),#31846,.T.);
#33652=ADVANCED_FACE('',(#5971),#1816,.F.);
#33653=ADVANCED_FACE('',(#5972),#1817,.F.);
#33654=ADVANCED_FACE('',(#5973),#1818,.F.);
#33655=ADVANCED_FACE('',(#5974),#31847,.T.);
#33656=ADVANCED_FACE('',(#5975),#1819,.F.);
#33657=ADVANCED_FACE('',(#5976),#1820,.T.);
#33658=ADVANCED_FACE('',(#5977),#1821,.F.);
#33659=ADVANCED_FACE('',(#5978),#31848,.T.);
#33660=ADVANCED_FACE('',(#5979),#31849,.T.);
#33661=ADVANCED_FACE('',(#5980),#1822,.F.);
#33662=ADVANCED_FACE('',(#5981),#1823,.F.);
#33663=ADVANCED_FACE('',(#5982),#1824,.F.);
#33664=ADVANCED_FACE('',(#5983),#31850,.T.);
#33665=ADVANCED_FACE('',(#5984),#1825,.F.);
#33666=ADVANCED_FACE('',(#5985),#1826,.T.);
#33667=ADVANCED_FACE('',(#5986),#1827,.F.);
#33668=ADVANCED_FACE('',(#5987),#31851,.T.);
#33669=ADVANCED_FACE('',(#5988),#1828,.F.);
#33670=ADVANCED_FACE('',(#5989),#1829,.F.);
#33671=ADVANCED_FACE('',(#5990),#1830,.F.);
#33672=ADVANCED_FACE('',(#5991),#1831,.F.);
#33673=ADVANCED_FACE('',(#5992),#31852,.T.);
#33674=ADVANCED_FACE('',(#5993),#1832,.F.);
#33675=ADVANCED_FACE('',(#5994),#31853,.T.);
#33676=ADVANCED_FACE('',(#5995),#1833,.F.);
#33677=ADVANCED_FACE('',(#5996),#31854,.T.);
#33678=ADVANCED_FACE('',(#5997,#2196),#31855,.T.);
#33679=ADVANCED_FACE('',(#5998,#2197),#31856,.T.);
#33680=ADVANCED_FACE('',(#5999,#2198),#31857,.T.);
#33681=ADVANCED_FACE('',(#6000),#700,.T.);
#33682=ADVANCED_FACE('',(#6001),#31858,.T.);
#33683=ADVANCED_FACE('',(#6002),#31859,.T.);
#33684=ADVANCED_FACE('',(#6003),#31860,.T.);
#33685=ADVANCED_FACE('',(#6004),#31861,.T.);
#33686=ADVANCED_FACE('',(#6005),#31862,.T.);
#33687=ADVANCED_FACE('',(#6006),#701,.F.);
#33688=ADVANCED_FACE('',(#6007),#31863,.T.);
#33689=ADVANCED_FACE('',(#6008),#702,.F.);
#33690=ADVANCED_FACE('',(#6009),#31864,.T.);
#33691=ADVANCED_FACE('',(#6010),#703,.F.);
#33692=ADVANCED_FACE('',(#6011),#31865,.T.);
#33693=ADVANCED_FACE('',(#6012),#704,.F.);
#33694=ADVANCED_FACE('',(#6013,#2199),#31866,.T.);
#33695=ADVANCED_FACE('',(#6014),#31867,.T.);
#33696=ADVANCED_FACE('',(#6015),#1834,.T.);
#33697=ADVANCED_FACE('',(#6016),#31868,.T.);
#33698=ADVANCED_FACE('',(#6017),#31869,.T.);
#33699=ADVANCED_FACE('',(#6018),#1835,.T.);
#33700=ADVANCED_FACE('',(#6019),#31870,.T.);
#33701=ADVANCED_FACE('',(#6020),#31871,.T.);
#33702=ADVANCED_FACE('',(#6021),#1836,.T.);
#33703=ADVANCED_FACE('',(#6022),#31872,.T.);
#33704=ADVANCED_FACE('',(#6023),#31873,.T.);
#33705=ADVANCED_FACE('',(#6024),#1837,.T.);
#33706=ADVANCED_FACE('',(#6025),#31874,.T.);
#33707=ADVANCED_FACE('',(#6026,#2200),#31875,.T.);
#33708=ADVANCED_FACE('',(#6027),#1838,.F.);
#33709=ADVANCED_FACE('',(#6028),#31876,.T.);
#33710=ADVANCED_FACE('',(#6029),#1839,.F.);
#33711=ADVANCED_FACE('',(#6030),#31877,.T.);
#33712=ADVANCED_FACE('',(#6031),#1840,.F.);
#33713=ADVANCED_FACE('',(#6032),#1841,.T.);
#33714=ADVANCED_FACE('',(#6033),#1842,.F.);
#33715=ADVANCED_FACE('',(#6034),#31878,.T.);
#33716=ADVANCED_FACE('',(#6035),#1843,.F.);
#33717=ADVANCED_FACE('',(#6036),#1844,.F.);
#33718=ADVANCED_FACE('',(#6037),#31879,.T.);
#33719=ADVANCED_FACE('',(#6038),#31880,.T.);
#33720=ADVANCED_FACE('',(#6039),#1845,.F.);
#33721=ADVANCED_FACE('',(#6040),#1846,.T.);
#33722=ADVANCED_FACE('',(#6041),#1847,.F.);
#33723=ADVANCED_FACE('',(#6042),#31881,.T.);
#33724=ADVANCED_FACE('',(#6043),#1848,.F.);
#33725=ADVANCED_FACE('',(#6044),#1849,.F.);
#33726=ADVANCED_FACE('',(#6045),#1850,.F.);
#33727=ADVANCED_FACE('',(#6046),#31882,.T.);
#33728=ADVANCED_FACE('',(#6047),#1851,.F.);
#33729=ADVANCED_FACE('',(#6048),#1852,.F.);
#33730=ADVANCED_FACE('',(#6049),#31883,.T.);
#33731=ADVANCED_FACE('',(#6050),#1853,.F.);
#33732=ADVANCED_FACE('',(#6051),#1854,.T.);
#33733=ADVANCED_FACE('',(#6052),#1855,.F.);
#33734=ADVANCED_FACE('',(#6053),#31884,.T.);
#33735=ADVANCED_FACE('',(#6054),#1856,.F.);
#33736=ADVANCED_FACE('',(#6055),#31885,.T.);
#33737=ADVANCED_FACE('',(#6056),#1857,.F.);
#33738=ADVANCED_FACE('',(#6057),#1858,.F.);
#33739=ADVANCED_FACE('',(#6058),#31886,.T.);
#33740=ADVANCED_FACE('',(#6059),#1859,.F.);
#33741=ADVANCED_FACE('',(#6060),#1860,.T.);
#33742=ADVANCED_FACE('',(#6061),#1861,.F.);
#33743=ADVANCED_FACE('',(#6062),#31887,.T.);
#33744=ADVANCED_FACE('',(#6063),#1862,.F.);
#33745=ADVANCED_FACE('',(#6064),#31888,.T.);
#33746=ADVANCED_FACE('',(#6065),#1863,.T.);
#33747=ADVANCED_FACE('',(#6066),#1864,.F.);
#33748=ADVANCED_FACE('',(#6067),#31889,.T.);
#33749=ADVANCED_FACE('',(#6068),#1865,.F.);
#33750=ADVANCED_FACE('',(#6069),#1866,.F.);
#33751=ADVANCED_FACE('',(#6070),#1867,.F.);
#33752=ADVANCED_FACE('',(#6071),#1868,.F.);
#33753=ADVANCED_FACE('',(#6072),#31890,.T.);
#33754=ADVANCED_FACE('',(#6073),#910,.T.);
#33755=ADVANCED_FACE('',(#6074,#2201,#2202,#2203,#2204,#2205,#2206,#2207),
#31891,.T.);
#33756=ADVANCED_FACE('',(#6075),#31892,.T.);
#33757=ADVANCED_FACE('',(#6076),#31893,.T.);
#33758=ADVANCED_FACE('',(#6077),#31894,.T.);
#33759=ADVANCED_FACE('',(#6078),#31895,.T.);
#33760=ADVANCED_FACE('',(#6079),#31896,.T.);
#33761=ADVANCED_FACE('',(#6080,#2208,#2209,#2210,#2211,#2212,#2213,#2214,
#2215,#2216,#2217,#2218,#2219,#2220,#2221,#2222),#31897,.T.);
#33762=ADVANCED_FACE('',(#6081),#31898,.T.);
#33763=ADVANCED_FACE('',(#6082),#31899,.T.);
#33764=ADVANCED_FACE('',(#6083),#31900,.T.);
#33765=ADVANCED_FACE('',(#6084,#2223),#31901,.T.);
#33766=ADVANCED_FACE('',(#6085),#705,.T.);
#33767=ADVANCED_FACE('',(#6086),#1869,.T.);
#33768=ADVANCED_FACE('',(#6087),#706,.T.);
#33769=ADVANCED_FACE('',(#6088),#31902,.T.);
#33770=ADVANCED_FACE('',(#6089),#31903,.T.);
#33771=ADVANCED_FACE('',(#6090),#31904,.T.);
#33772=ADVANCED_FACE('',(#6091),#31905,.T.);
#33773=ADVANCED_FACE('',(#6092),#31906,.T.);
#33774=ADVANCED_FACE('',(#6093),#31907,.T.);
#33775=ADVANCED_FACE('',(#6094),#31908,.T.);
#33776=ADVANCED_FACE('',(#6095,#2224),#31909,.T.);
#33777=ADVANCED_FACE('',(#6096,#2225,#2226),#1870,.F.);
#33778=ADVANCED_FACE('',(#6097),#1871,.F.);
#33779=ADVANCED_FACE('',(#6098),#1872,.F.);
#33780=ADVANCED_FACE('',(#6099),#1873,.F.);
#33781=ADVANCED_FACE('',(#6100),#1874,.F.);
#33782=ADVANCED_FACE('',(#6101,#2227),#31910,.T.);
#33783=ADVANCED_FACE('',(#6102,#2228,#2229),#1875,.F.);
#33784=ADVANCED_FACE('',(#6103,#2230,#2231),#1876,.T.);
#33785=ADVANCED_FACE('',(#6104),#707,.T.);
#33786=ADVANCED_FACE('',(#6105,#2232),#31911,.T.);
#33787=ADVANCED_FACE('',(#6106),#708,.T.);
#33788=ADVANCED_FACE('',(#6107,#2233,#2234),#1877,.T.);
#33789=ADVANCED_FACE('',(#6108,#2235),#31912,.T.);
#33790=ADVANCED_FACE('',(#6109),#709,.T.);
#33791=CLOSED_SHELL('',(#31913,#31914,#31915,#31916,#31917,#31918,#31919,
#31920,#31921,#31922,#31923,#31924,#31925,#31926,#31927,#31928,#31929,#31930,
#31931,#31932,#31933));
#33792=CLOSED_SHELL('',(#31934,#31935,#31936,#31937,#31938,#31939,#31940,
#31941,#31942,#31943,#31944,#31945,#31946,#31947,#31948,#31949,#31950,#31951,
#31952,#31953,#31954,#31955,#31956,#31957,#31958,#31959,#31960,#31961,#31962,
#31963,#31964,#31965,#31966,#31967,#31968,#31969,#31970,#31971,#31972,#31973,
#31974,#31975,#31976,#31977,#31978,#31979,#31980,#31981,#31982,#31983,#31984,
#31985,#31986,#31987,#31988,#31989,#31990,#31991,#31992,#31993,#31994,#31995,
#31996,#31997,#31998,#31999,#32000,#32001,#32002,#32003,#32004,#32005,#32006,
#32007,#32008,#32009,#32010,#32011,#32012,#32013,#32014,#32015,#32016,#32017,
#32018,#32019,#32020,#32021,#32022,#32023,#32024,#32025,#32026,#32027,#32028,
#32029,#32030,#32031,#32032,#32033,#32034,#32035,#32036,#32037,#32038,#32039,
#32040,#32041,#32042,#32043,#32044,#32045,#32046,#32047,#32048,#32049,#32050,
#32051,#32052));
#33793=CLOSED_SHELL('',(#32053,#32054,#32055,#32056,#32057,#32058,#32059,
#32060,#32061,#32062,#32063,#32064,#32065,#32066,#32067));
#33794=CLOSED_SHELL('',(#32068,#32069,#32070,#32071,#32072,#32073,#32074,
#32075,#32076,#32077,#32078,#32079,#32080,#32081,#32082));
#33795=CLOSED_SHELL('',(#32083,#32084,#32085,#32086,#32087,#32088,#32089,
#32090,#32091,#32092,#32093,#32094,#32095,#32096,#32097));
#33796=CLOSED_SHELL('',(#32098,#32099,#32100,#32101,#32102,#32103,#32104,
#32105,#32106,#32107,#32108,#32109,#32110,#32111,#32112,#32113,#32114,#32115,
#32116,#32117));
#33797=CLOSED_SHELL('',(#32118,#32119,#32120,#32121,#32122,#32123,#32124,
#32125,#32126,#32127,#32128,#32129,#32130,#32131,#32132));
#33798=CLOSED_SHELL('',(#32133,#32134,#32135,#32136,#32137,#32138,#32139,
#32140,#32141,#32142,#32143,#32144,#32145,#32146,#32147,#32148,#32149,#32150,
#32151,#32152,#32153,#32154,#32155,#32156,#32157,#32158,#32159));
#33799=CLOSED_SHELL('',(#32160,#32161,#32162,#32163,#32164,#32165,#32166,
#32167,#32168,#32169,#32170,#32171,#32172,#32173,#32174,#32175,#32176,#32177,
#32178,#32179,#32180,#32181,#32182,#32183,#32184,#32185,#32186,#32187,#32188,
#32189,#32190,#32191,#32192,#32193,#32194,#32195,#32196,#32197,#32198,#32199,
#32200,#32201,#32202,#32203,#32204,#32205,#32206,#32207,#32208,#32209,#32210,
#32211,#32212,#32213,#32214,#32215,#32216,#32217,#32218,#32219,#32220,#32221,
#32222,#32223,#32224,#32225,#32226,#32227,#32228,#32229,#32230,#32231,#32232,
#32233,#32234,#32235,#32236,#32237,#32238,#32239,#32240,#32241,#32242,#32243,
#32244,#32245,#32246,#32247,#32248,#32249,#32250,#32251,#32252,#32253,#32254,
#32255,#32256,#32257,#32258,#32259,#32260,#32261,#32262,#32263,#32264,#32265,
#32266,#32267,#32268,#32269,#32270,#32271,#32272,#32273,#32274,#32275,#32276,
#32277,#32278,#32279,#32280,#32281,#32282,#32283,#32284,#32285,#32286,#32287,
#32288,#32289,#32290,#32291,#32292,#32293,#32294,#32295,#32296,#32297,#32298,
#32299,#32300,#32301,#32302,#32303,#32304,#32305,#32306,#32307,#32308,#32309,
#32310,#32311,#32312,#32313,#32314,#32315,#32316,#32317,#32318,#32319,#32320,
#32321,#32322,#32323,#32324,#32325,#32326,#32327,#32328,#32329,#32330,#32331,
#32332,#32333,#32334,#32335,#32336,#32337,#32338,#32339,#32340,#32341,#32342,
#32343,#32344,#32345,#32346,#32347,#32348,#32349,#32350,#32351,#32352,#32353,
#32354,#32355,#32356,#32357,#32358,#32359,#32360,#32361,#32362,#32363,#32364,
#32365,#32366,#32367,#32368,#32369,#32370,#32371,#32372,#32373,#32374,#32375,
#32376,#32377,#32378,#32379,#32380,#32381,#32382,#32383,#32384,#32385,#32386,
#32387,#32388,#32389,#32390,#32391,#32392,#32393,#32394,#32395,#32396,#32397,
#32398,#32399,#32400,#32401,#32402,#32403,#32404,#32405,#32406,#32407,#32408));
#33800=CLOSED_SHELL('',(#32409,#32410,#32411,#32412,#32413,#32414,#32415,
#32416,#32417,#32418,#32419,#32420,#32421,#32422,#32423,#32424,#32425,#32426,
#32427,#32428,#32429,#32430,#32431,#32432,#32433,#32434,#32435,#32436,#32437,
#32438,#32439,#32440,#32441,#32442,#32443,#32444,#32445,#32446,#32447,#32448,
#32449,#32450,#32451,#32452,#32453,#32454,#32455,#32456,#32457,#32458,#32459,
#32460,#32461,#32462,#32463,#32464,#32465,#32466,#32467,#32468,#32469,#32470,
#32471,#32472,#32473,#32474,#32475,#32476,#32477,#32478,#32479,#32480,#32481,
#32482,#32483,#32484,#32485,#32486));
#33801=CLOSED_SHELL('',(#32487,#32488,#32489,#32490,#32491,#32492,#32493,
#32494,#32495,#32496,#32497,#32498,#32499,#32500,#32501,#32502,#32503,#32504));
#33802=CLOSED_SHELL('',(#32505,#32506,#32507,#32508,#32509,#32510,#32511,
#32512,#32513,#32514,#32515,#32516,#32517,#32518,#32519,#32520,#32521,#32522));
#33803=CLOSED_SHELL('',(#32523,#32524,#32525,#32526,#32527,#32528,#32529,
#32530,#32531,#32532,#32533,#32534,#32535,#32536,#32537,#32538,#32539,#32540));
#33804=CLOSED_SHELL('',(#32541,#32542,#32543,#32544,#32545,#32546,#32547,
#32548,#32549,#32550,#32551,#32552,#32553,#32554,#32555,#32556,#32557,#32558));
#33805=CLOSED_SHELL('',(#32559,#32560,#32561,#32562,#32563,#32564,#32565,
#32566,#32567,#32568,#32569,#32570,#32571,#32572,#32573,#32574,#32575,#32576));
#33806=CLOSED_SHELL('',(#32577,#32578,#32579,#32580,#32581,#32582,#32583,
#32584,#32585,#32586,#32587,#32588,#32589,#32590,#32591,#32592,#32593,#32594));
#33807=CLOSED_SHELL('',(#32595,#32596,#32597,#32598,#32599,#32600,#32601,
#32602,#32603,#32604,#32605,#32606,#32607,#32608,#32609,#32610,#32611,#32612));
#33808=CLOSED_SHELL('',(#32613,#32614,#32615,#32616,#32617,#32618,#32619,
#32620,#32621,#32622,#32623,#32624,#32625,#32626,#32627,#32628,#32629,#32630));
#33809=CLOSED_SHELL('',(#32631,#32632,#32633,#32634,#32635,#32636,#32637,
#32638,#32639,#32640,#32641,#32642,#32643,#32644,#32645,#32646,#32647,#32648));
#33810=CLOSED_SHELL('',(#32649,#32650,#32651,#32652,#32653,#32654,#32655,
#32656,#32657,#32658,#32659,#32660,#32661,#32662,#32663,#32664,#32665,#32666));
#33811=CLOSED_SHELL('',(#32667,#32668,#32669,#32670,#32671,#32672,#32673,
#32674,#32675,#32676,#32677,#32678,#32679,#32680,#32681,#32682,#32683,#32684));
#33812=CLOSED_SHELL('',(#32685,#32686,#32687,#32688,#32689,#32690,#32691,
#32692,#32693,#32694,#32695,#32696,#32697,#32698,#32699,#32700,#32701,#32702));
#33813=CLOSED_SHELL('',(#32703,#32704,#32705,#32706,#32707,#32708,#32709,
#32710,#32711,#32712,#32713,#32714,#32715,#32716,#32717,#32718,#32719,#32720));
#33814=CLOSED_SHELL('',(#32721,#32722,#32723,#32724,#32725,#32726,#32727,
#32728,#32729,#32730,#32731,#32732,#32733,#32734,#32735,#32736,#32737,#32738));
#33815=CLOSED_SHELL('',(#32739,#32740,#32741,#32742,#32743,#32744,#32745,
#32746,#32747,#32748,#32749,#32750,#32751,#32752,#32753,#32754,#32755,#32756));
#33816=CLOSED_SHELL('',(#32757,#32758,#32759,#32760,#32761,#32762,#32763,
#32764,#32765,#32766,#32767,#32768,#32769,#32770,#32771,#32772,#32773,#32774,
#32775,#32776,#32777,#32778,#32779,#32780,#32781,#32782));
#33817=CLOSED_SHELL('',(#32783,#32784,#32785,#32786,#32787,#32788,#32789,
#32790,#32791,#32792,#32793,#32794,#32795,#32796,#32797,#32798,#32799,#32800,
#32801,#32802,#32803,#32804,#32805,#32806,#32807,#32808,#32809,#32810));
#33818=CLOSED_SHELL('',(#32811,#32812,#32813,#32814,#32815,#32816,#32817,
#32818,#32819,#32820,#32821,#32822,#32823,#32824,#32825,#32826,#32827,#32828,
#32829,#32830,#32831,#32832,#32833,#32834,#32835,#32836,#32837,#32838));
#33819=CLOSED_SHELL('',(#32839,#32840,#32841,#32842,#32843,#32844,#32845,
#32846,#32847,#32848,#32849,#32850));
#33820=CLOSED_SHELL('',(#32851,#32852,#32853,#32854,#32855,#32856,#32857,
#32858,#32859,#32860));
#33821=CLOSED_SHELL('',(#32861,#32862,#32863,#32864,#32865,#32866,#32867,
#32868,#32869,#32870,#32871,#32872,#32873,#32874));
#33822=CLOSED_SHELL('',(#32875,#32876,#32877,#32878,#32879,#32880,#32881,
#32882,#32883,#32884,#32885,#32886,#32887,#32888,#32889,#32890,#32891,#32892,
#32893,#32894,#32895,#32896,#32897,#32898,#32899,#32900,#32901,#32902,#32903,
#32904,#32905,#32906));
#33823=CLOSED_SHELL('',(#32907,#32908,#32909,#32910,#32911,#32912,#32913,
#32914,#32915,#32916,#32917,#32918,#32919,#32920,#32921,#32922,#32923,#32924,
#32925,#32926,#32927,#32928,#32929,#32930,#32931,#32932,#32933,#32934,#32935,
#32936,#32937,#32938,#32939,#32940,#32941));
#33824=CLOSED_SHELL('',(#32942,#32943,#32944,#32945,#32946,#32947,#32948));
#33825=CLOSED_SHELL('',(#32949,#32950,#32951,#32952));
#33826=CLOSED_SHELL('',(#32953,#32954,#32955,#32956,#32957,#32958,#32959,
#32960,#32961,#32962,#32963,#32964,#32965,#32966,#32967,#32968,#32969,#32970,
#32971,#32972,#32973,#32974,#32975,#32976,#32977,#32978,#32979,#32980,#32981,
#32982,#32983,#32984,#32985,#32986,#32987,#32988,#32989,#32990,#32991,#32992,
#32993,#32994,#32995,#32996,#32997,#32998,#32999,#33000,#33001,#33002,#33003,
#33004,#33005,#33006,#33007,#33008,#33009,#33010,#33011,#33012,#33013,#33014,
#33015,#33016,#33017,#33018,#33019,#33020,#33021,#33022,#33023,#33024,#33025,
#33026,#33027,#33028,#33029,#33030,#33031,#33032,#33033,#33034,#33035,#33036,
#33037,#33038,#33039,#33040,#33041,#33042,#33043,#33044,#33045,#33046,#33047,
#33048,#33049,#33050,#33051,#33052,#33053,#33054,#33055,#33056,#33057,#33058,
#33059,#33060,#33061,#33062,#33063,#33064,#33065,#33066,#33067,#33068,#33069,
#33070,#33071,#33072,#33073,#33074,#33075,#33076,#33077,#33078,#33079,#33080,
#33081,#33082,#33083,#33084,#33085,#33086,#33087,#33088,#33089,#33090,#33091,
#33092,#33093,#33094,#33095,#33096,#33097,#33098,#33099,#33100,#33101,#33102,
#33103,#33104,#33105,#33106,#33107,#33108,#33109,#33110,#33111,#33112,#33113,
#33114,#33115,#33116,#33117,#33118,#33119,#33120,#33121,#33122,#33123,#33124,
#33125,#33126,#33127,#33128,#33129,#33130,#33131,#33132,#33133,#33134,#33135,
#33136,#33137,#33138,#33139,#33140,#33141,#33142,#33143,#33144,#33145,#33146,
#33147,#33148,#33149,#33150,#33151,#33152,#33153,#33154));
#33827=CLOSED_SHELL('',(#33155,#33156,#33157,#33158,#33159,#33160,#33161,
#33162,#33163,#33164,#33165,#33166,#33167,#33168,#33169,#33170,#33171,#33172,
#33173,#33174,#33175,#33176,#33177,#33178,#33179,#33180,#33181,#33182,#33183,
#33184,#33185,#33186,#33187,#33188,#33189,#33190,#33191,#33192,#33193,#33194,
#33195,#33196,#33197,#33198,#33199,#33200,#33201,#33202,#33203,#33204,#33205,
#33206,#33207,#33208,#33209,#33210,#33211,#33212,#33213,#33214,#33215,#33216,
#33217,#33218,#33219,#33220,#33221,#33222,#33223,#33224,#33225,#33226,#33227,
#33228,#33229,#33230,#33231,#33232,#33233,#33234,#33235,#33236,#33237,#33238,
#33239,#33240,#33241,#33242,#33243,#33244,#33245,#33246,#33247,#33248,#33249,
#33250,#33251,#33252,#33253,#33254,#33255,#33256,#33257,#33258,#33259,#33260,
#33261,#33262,#33263,#33264,#33265,#33266,#33267,#33268,#33269,#33270,#33271,
#33272,#33273,#33274,#33275,#33276,#33277,#33278,#33279,#33280,#33281,#33282,
#33283,#33284,#33285,#33286,#33287,#33288,#33289,#33290,#33291,#33292,#33293,
#33294,#33295,#33296,#33297,#33298,#33299,#33300,#33301,#33302,#33303,#33304,
#33305,#33306,#33307,#33308,#33309,#33310,#33311,#33312,#33313,#33314,#33315,
#33316,#33317,#33318,#33319,#33320,#33321,#33322,#33323,#33324));
#33828=CLOSED_SHELL('',(#33325,#33326,#33327,#33328));
#33829=CLOSED_SHELL('',(#33329,#33330,#33331,#33332));
#33830=CLOSED_SHELL('',(#33333,#33334,#33335,#33336));
#33831=CLOSED_SHELL('',(#33337,#33338,#33339,#33340));
#33832=CLOSED_SHELL('',(#33341,#33342,#33343,#33344));
#33833=CLOSED_SHELL('',(#33345,#33346,#33347,#33348));
#33834=CLOSED_SHELL('',(#33349,#33350,#33351,#33352));
#33835=CLOSED_SHELL('',(#33353,#33354,#33355,#33356));
#33836=CLOSED_SHELL('',(#33357,#33358,#33359,#33360));
#33837=CLOSED_SHELL('',(#33361,#33362,#33363,#33364));
#33838=CLOSED_SHELL('',(#33365,#33366,#33367,#33368,#33369,#33370,#33371,
#33372,#33373,#33374,#33375,#33376,#33377,#33378,#33379,#33380,#33381,#33382,
#33383,#33384,#33385,#33386,#33387,#33388,#33389,#33390,#33391,#33392,#33393,
#33394,#33395,#33396,#33397,#33398,#33399,#33400,#33401,#33402,#33403,#33404,
#33405,#33406,#33407,#33408,#33409,#33410,#33411,#33412,#33413,#33414,#33415,
#33416,#33417,#33418,#33419,#33420,#33421,#33422,#33423,#33424,#33425,#33426,
#33427,#33428,#33429,#33430,#33431,#33432,#33433,#33434,#33435,#33436,#33437,
#33438,#33439,#33440,#33441,#33442,#33443,#33444,#33445,#33446,#33447,#33448,
#33449,#33450,#33451,#33452,#33453,#33454,#33455,#33456,#33457,#33458,#33459,
#33460,#33461,#33462,#33463,#33464,#33465,#33466,#33467,#33468,#33469,#33470,
#33471,#33472,#33473,#33474,#33475,#33476,#33477,#33478,#33479,#33480,#33481,
#33482,#33483,#33484,#33485,#33486,#33487,#33488,#33489,#33490,#33491,#33492,
#33493,#33494,#33495,#33496,#33497,#33498,#33499,#33500,#33501,#33502,#33503,
#33504,#33505,#33506,#33507,#33508,#33509,#33510,#33511,#33512,#33513,#33514,
#33515,#33516,#33517,#33518,#33519,#33520,#33521,#33522,#33523,#33524,#33525,
#33526,#33527,#33528,#33529,#33530,#33531,#33532,#33533,#33534,#33535,#33536,
#33537,#33538,#33539,#33540,#33541,#33542,#33543,#33544,#33545,#33546,#33547,
#33548,#33549,#33550,#33551,#33552,#33553,#33554,#33555,#33556,#33557,#33558,
#33559,#33560,#33561,#33562,#33563,#33564,#33565,#33566,#33567,#33568,#33569,
#33570,#33571,#33572,#33573,#33574,#33575,#33576,#33577,#33578,#33579,#33580,
#33581,#33582,#33583,#33584,#33585,#33586,#33587,#33588,#33589,#33590,#33591,
#33592,#33593,#33594,#33595,#33596,#33597,#33598,#33599,#33600,#33601,#33602,
#33603,#33604,#33605,#33606,#33607,#33608,#33609,#33610,#33611,#33612,#33613,
#33614,#33615,#33616,#33617,#33618,#33619,#33620,#33621,#33622,#33623,#33624,
#33625,#33626,#33627,#33628,#33629,#33630,#33631,#33632,#33633,#33634,#33635,
#33636,#33637,#33638,#33639,#33640,#33641,#33642,#33643,#33644,#33645,#33646,
#33647,#33648,#33649,#33650,#33651,#33652,#33653,#33654,#33655,#33656,#33657,
#33658,#33659,#33660,#33661,#33662,#33663,#33664,#33665,#33666,#33667,#33668,
#33669,#33670,#33671,#33672,#33673,#33674,#33675,#33676,#33677,#33678,#33679,
#33680,#33681,#33682,#33683,#33684,#33685,#33686,#33687,#33688,#33689,#33690,
#33691,#33692,#33693,#33694,#33695,#33696,#33697,#33698,#33699,#33700,#33701,
#33702,#33703,#33704,#33705,#33706,#33707,#33708,#33709,#33710,#33711,#33712,
#33713,#33714,#33715,#33716,#33717,#33718,#33719,#33720,#33721,#33722,#33723,
#33724,#33725,#33726,#33727,#33728,#33729,#33730,#33731,#33732,#33733,#33734,
#33735,#33736,#33737,#33738,#33739,#33740,#33741,#33742,#33743,#33744,#33745,
#33746,#33747,#33748,#33749,#33750,#33751,#33752,#33753,#33754,#33755,#33756,
#33757,#33758,#33759,#33760,#33761,#33762,#33763,#33764,#33765,#33766,#33767,
#33768,#33769,#33770,#33771,#33772,#33773,#33774,#33775,#33776));
#33839=CLOSED_SHELL('',(#33777,#33778,#33779,#33780,#33781,#33782,#33783,
#33784,#33785,#33786,#33787,#33788,#33789,#33790));
#33840=DERIVED_UNIT_ELEMENT(#33890,1.);
#33841=DERIVED_UNIT_ELEMENT(#61813,-3.);
#33842=DERIVED_UNIT_ELEMENT(#33890,1.);
#33843=DERIVED_UNIT_ELEMENT(#61813,-3.);
#33844=DERIVED_UNIT_ELEMENT(#33890,1.);
#33845=DERIVED_UNIT_ELEMENT(#61813,-3.);
#33846=DERIVED_UNIT_ELEMENT(#33890,1.);
#33847=DERIVED_UNIT_ELEMENT(#61813,-3.);
#33848=DERIVED_UNIT_ELEMENT(#33890,1.);
#33849=DERIVED_UNIT_ELEMENT(#61813,-3.);
#33850=DERIVED_UNIT_ELEMENT(#33890,1.);
#33851=DERIVED_UNIT_ELEMENT(#61813,-3.);
#33852=DERIVED_UNIT_ELEMENT(#33890,1.);
#33853=DERIVED_UNIT_ELEMENT(#61813,-3.);
#33854=DERIVED_UNIT_ELEMENT(#33890,1.);
#33855=DERIVED_UNIT_ELEMENT(#61813,-3.);
#33856=DERIVED_UNIT_ELEMENT(#33890,1.);
#33857=DERIVED_UNIT_ELEMENT(#61813,-3.);
#33858=DERIVED_UNIT_ELEMENT(#33890,1.);
#33859=DERIVED_UNIT_ELEMENT(#61813,-3.);
#33860=DERIVED_UNIT_ELEMENT(#33890,1.);
#33861=DERIVED_UNIT_ELEMENT(#61813,-3.);
#33862=DERIVED_UNIT_ELEMENT(#33890,1.);
#33863=DERIVED_UNIT_ELEMENT(#61813,-3.);
#33864=DERIVED_UNIT_ELEMENT(#33890,1.);
#33865=DERIVED_UNIT_ELEMENT(#61813,-3.);
#33866=DERIVED_UNIT_ELEMENT(#33890,1.);
#33867=DERIVED_UNIT_ELEMENT(#61813,-3.);
#33868=DERIVED_UNIT_ELEMENT(#33890,1.);
#33869=DERIVED_UNIT_ELEMENT(#61813,-3.);
#33870=DERIVED_UNIT_ELEMENT(#33890,1.);
#33871=DERIVED_UNIT_ELEMENT(#61813,-3.);
#33872=DERIVED_UNIT_ELEMENT(#33890,1.);
#33873=DERIVED_UNIT_ELEMENT(#61813,-3.);
#33874=DERIVED_UNIT_ELEMENT(#33890,1.);
#33875=DERIVED_UNIT_ELEMENT(#61813,-3.);
#33876=DERIVED_UNIT_ELEMENT(#33890,1.);
#33877=DERIVED_UNIT_ELEMENT(#61813,-3.);
#33878=DERIVED_UNIT_ELEMENT(#33890,1.);
#33879=DERIVED_UNIT_ELEMENT(#61813,-3.);
#33880=DERIVED_UNIT_ELEMENT(#33890,1.);
#33881=DERIVED_UNIT_ELEMENT(#61813,-3.);
#33882=DERIVED_UNIT_ELEMENT(#33890,1.);
#33883=DERIVED_UNIT_ELEMENT(#61813,-3.);
#33884=DERIVED_UNIT_ELEMENT(#33890,1.);
#33885=DERIVED_UNIT_ELEMENT(#61813,-3.);
#33886=DERIVED_UNIT_ELEMENT(#33890,1.);
#33887=DERIVED_UNIT_ELEMENT(#61813,-3.);
#33888=DERIVED_UNIT_ELEMENT(#33890,1.);
#33889=DERIVED_UNIT_ELEMENT(#61813,-3.);
#33890=(
MASS_UNIT()
NAMED_UNIT(*)
SI_UNIT(.KILO.,.GRAM.)
);
#33891=DERIVED_UNIT((#33840,#33841));
#33892=DERIVED_UNIT((#33842,#33843));
#33893=DERIVED_UNIT((#33844,#33845));
#33894=DERIVED_UNIT((#33846,#33847));
#33895=DERIVED_UNIT((#33848,#33849));
#33896=DERIVED_UNIT((#33850,#33851));
#33897=DERIVED_UNIT((#33852,#33853));
#33898=DERIVED_UNIT((#33854,#33855));
#33899=DERIVED_UNIT((#33856,#33857));
#33900=DERIVED_UNIT((#33858,#33859));
#33901=DERIVED_UNIT((#33860,#33861));
#33902=DERIVED_UNIT((#33862,#33863));
#33903=DERIVED_UNIT((#33864,#33865));
#33904=DERIVED_UNIT((#33866,#33867));
#33905=DERIVED_UNIT((#33868,#33869));
#33906=DERIVED_UNIT((#33870,#33871));
#33907=DERIVED_UNIT((#33872,#33873));
#33908=DERIVED_UNIT((#33874,#33875));
#33909=DERIVED_UNIT((#33876,#33877));
#33910=DERIVED_UNIT((#33878,#33879));
#33911=DERIVED_UNIT((#33880,#33881));
#33912=DERIVED_UNIT((#33882,#33883));
#33913=DERIVED_UNIT((#33884,#33885));
#33914=DERIVED_UNIT((#33886,#33887));
#33915=DERIVED_UNIT((#33888,#33889));
#33916=MEASURE_REPRESENTATION_ITEM('density measure',
POSITIVE_RATIO_MEASURE(7850.),#33891);
#33917=MEASURE_REPRESENTATION_ITEM('density measure',
POSITIVE_RATIO_MEASURE(7850.),#33892);
#33918=MEASURE_REPRESENTATION_ITEM('density measure',
POSITIVE_RATIO_MEASURE(7850.),#33893);
#33919=MEASURE_REPRESENTATION_ITEM('density measure',
POSITIVE_RATIO_MEASURE(7850.),#33894);
#33920=MEASURE_REPRESENTATION_ITEM('density measure',
POSITIVE_RATIO_MEASURE(7850.),#33895);
#33921=MEASURE_REPRESENTATION_ITEM('density measure',
POSITIVE_RATIO_MEASURE(7850.),#33896);
#33922=MEASURE_REPRESENTATION_ITEM('density measure',
POSITIVE_RATIO_MEASURE(7850.),#33897);
#33923=MEASURE_REPRESENTATION_ITEM('density measure',
POSITIVE_RATIO_MEASURE(7850.),#33898);
#33924=MEASURE_REPRESENTATION_ITEM('density measure',
POSITIVE_RATIO_MEASURE(7850.),#33899);
#33925=MEASURE_REPRESENTATION_ITEM('density measure',
POSITIVE_RATIO_MEASURE(7850.),#33900);
#33926=MEASURE_REPRESENTATION_ITEM('density measure',
POSITIVE_RATIO_MEASURE(7850.),#33901);
#33927=MEASURE_REPRESENTATION_ITEM('density measure',
POSITIVE_RATIO_MEASURE(7850.),#33902);
#33928=MEASURE_REPRESENTATION_ITEM('density measure',
POSITIVE_RATIO_MEASURE(7850.),#33903);
#33929=MEASURE_REPRESENTATION_ITEM('density measure',
POSITIVE_RATIO_MEASURE(7850.),#33904);
#33930=MEASURE_REPRESENTATION_ITEM('density measure',
POSITIVE_RATIO_MEASURE(7850.),#33905);
#33931=MEASURE_REPRESENTATION_ITEM('density measure',
POSITIVE_RATIO_MEASURE(7850.),#33906);
#33932=MEASURE_REPRESENTATION_ITEM('density measure',
POSITIVE_RATIO_MEASURE(7850.),#33907);
#33933=MEASURE_REPRESENTATION_ITEM('density measure',
POSITIVE_RATIO_MEASURE(7850.),#33908);
#33934=MEASURE_REPRESENTATION_ITEM('density measure',
POSITIVE_RATIO_MEASURE(7850.),#33909);
#33935=MEASURE_REPRESENTATION_ITEM('density measure',
POSITIVE_RATIO_MEASURE(7850.),#33910);
#33936=MEASURE_REPRESENTATION_ITEM('density measure',
POSITIVE_RATIO_MEASURE(7850.),#33911);
#33937=MEASURE_REPRESENTATION_ITEM('density measure',
POSITIVE_RATIO_MEASURE(7850.),#33912);
#33938=MEASURE_REPRESENTATION_ITEM('density measure',
POSITIVE_RATIO_MEASURE(7850.),#33913);
#33939=MEASURE_REPRESENTATION_ITEM('density measure',
POSITIVE_RATIO_MEASURE(7850.),#33914);
#33940=MEASURE_REPRESENTATION_ITEM('density measure',
POSITIVE_RATIO_MEASURE(7850.),#33915);
#33941=PROPERTY_DEFINITION_REPRESENTATION(#34066,#33991);
#33942=PROPERTY_DEFINITION_REPRESENTATION(#34067,#33992);
#33943=PROPERTY_DEFINITION_REPRESENTATION(#34068,#33993);
#33944=PROPERTY_DEFINITION_REPRESENTATION(#34069,#33994);
#33945=PROPERTY_DEFINITION_REPRESENTATION(#34070,#33995);
#33946=PROPERTY_DEFINITION_REPRESENTATION(#34071,#33996);
#33947=PROPERTY_DEFINITION_REPRESENTATION(#34072,#33997);
#33948=PROPERTY_DEFINITION_REPRESENTATION(#34073,#33998);
#33949=PROPERTY_DEFINITION_REPRESENTATION(#34074,#33999);
#33950=PROPERTY_DEFINITION_REPRESENTATION(#34075,#34000);
#33951=PROPERTY_DEFINITION_REPRESENTATION(#34076,#34001);
#33952=PROPERTY_DEFINITION_REPRESENTATION(#34077,#34002);
#33953=PROPERTY_DEFINITION_REPRESENTATION(#34078,#34003);
#33954=PROPERTY_DEFINITION_REPRESENTATION(#34079,#34004);
#33955=PROPERTY_DEFINITION_REPRESENTATION(#34080,#34005);
#33956=PROPERTY_DEFINITION_REPRESENTATION(#34081,#34006);
#33957=PROPERTY_DEFINITION_REPRESENTATION(#34082,#34007);
#33958=PROPERTY_DEFINITION_REPRESENTATION(#34083,#34008);
#33959=PROPERTY_DEFINITION_REPRESENTATION(#34084,#34009);
#33960=PROPERTY_DEFINITION_REPRESENTATION(#34085,#34010);
#33961=PROPERTY_DEFINITION_REPRESENTATION(#34086,#34011);
#33962=PROPERTY_DEFINITION_REPRESENTATION(#34087,#34012);
#33963=PROPERTY_DEFINITION_REPRESENTATION(#34088,#34013);
#33964=PROPERTY_DEFINITION_REPRESENTATION(#34089,#34014);
#33965=PROPERTY_DEFINITION_REPRESENTATION(#34090,#34015);
#33966=PROPERTY_DEFINITION_REPRESENTATION(#34091,#34016);
#33967=PROPERTY_DEFINITION_REPRESENTATION(#34092,#34017);
#33968=PROPERTY_DEFINITION_REPRESENTATION(#34093,#34018);
#33969=PROPERTY_DEFINITION_REPRESENTATION(#34094,#34019);
#33970=PROPERTY_DEFINITION_REPRESENTATION(#34095,#34020);
#33971=PROPERTY_DEFINITION_REPRESENTATION(#34096,#34021);
#33972=PROPERTY_DEFINITION_REPRESENTATION(#34097,#34022);
#33973=PROPERTY_DEFINITION_REPRESENTATION(#34098,#34023);
#33974=PROPERTY_DEFINITION_REPRESENTATION(#34099,#34024);
#33975=PROPERTY_DEFINITION_REPRESENTATION(#34100,#34025);
#33976=PROPERTY_DEFINITION_REPRESENTATION(#34101,#34026);
#33977=PROPERTY_DEFINITION_REPRESENTATION(#34102,#34027);
#33978=PROPERTY_DEFINITION_REPRESENTATION(#34103,#34028);
#33979=PROPERTY_DEFINITION_REPRESENTATION(#34104,#34029);
#33980=PROPERTY_DEFINITION_REPRESENTATION(#34105,#34030);
#33981=PROPERTY_DEFINITION_REPRESENTATION(#34106,#34031);
#33982=PROPERTY_DEFINITION_REPRESENTATION(#34107,#34032);
#33983=PROPERTY_DEFINITION_REPRESENTATION(#34108,#34033);
#33984=PROPERTY_DEFINITION_REPRESENTATION(#34109,#34034);
#33985=PROPERTY_DEFINITION_REPRESENTATION(#34110,#34035);
#33986=PROPERTY_DEFINITION_REPRESENTATION(#34111,#34036);
#33987=PROPERTY_DEFINITION_REPRESENTATION(#34112,#34037);
#33988=PROPERTY_DEFINITION_REPRESENTATION(#34113,#34038);
#33989=PROPERTY_DEFINITION_REPRESENTATION(#34114,#34039);
#33990=PROPERTY_DEFINITION_REPRESENTATION(#34115,#34040);
#33991=REPRESENTATION('material name',(#34041),#61782);
#33992=REPRESENTATION('density',(#33916),#61782);
#33993=REPRESENTATION('material name',(#34042),#61783);
#33994=REPRESENTATION('density',(#33917),#61783);
#33995=REPRESENTATION('material name',(#34043),#61784);
#33996=REPRESENTATION('density',(#33918),#61784);
#33997=REPRESENTATION('material name',(#34044),#61785);
#33998=REPRESENTATION('density',(#33919),#61785);
#33999=REPRESENTATION('material name',(#34045),#61786);
#34000=REPRESENTATION('density',(#33920),#61786);
#34001=REPRESENTATION('material name',(#34046),#61787);
#34002=REPRESENTATION('density',(#33921),#61787);
#34003=REPRESENTATION('material name',(#34047),#61788);
#34004=REPRESENTATION('density',(#33922),#61788);
#34005=REPRESENTATION('material name',(#34048),#61789);
#34006=REPRESENTATION('density',(#33923),#61789);
#34007=REPRESENTATION('material name',(#34049),#61790);
#34008=REPRESENTATION('density',(#33924),#61790);
#34009=REPRESENTATION('material name',(#34050),#61791);
#34010=REPRESENTATION('density',(#33925),#61791);
#34011=REPRESENTATION('material name',(#34051),#61792);
#34012=REPRESENTATION('density',(#33926),#61792);
#34013=REPRESENTATION('material name',(#34052),#61794);
#34014=REPRESENTATION('density',(#33927),#61794);
#34015=REPRESENTATION('material name',(#34053),#61795);
#34016=REPRESENTATION('density',(#33928),#61795);
#34017=REPRESENTATION('material name',(#34054),#61796);
#34018=REPRESENTATION('density',(#33929),#61796);
#34019=REPRESENTATION('material name',(#34055),#61797);
#34020=REPRESENTATION('density',(#33930),#61797);
#34021=REPRESENTATION('material name',(#34056),#61798);
#34022=REPRESENTATION('density',(#33931),#61798);
#34023=REPRESENTATION('material name',(#34057),#61799);
#34024=REPRESENTATION('density',(#33932),#61799);
#34025=REPRESENTATION('material name',(#34058),#61801);
#34026=REPRESENTATION('density',(#33933),#61801);
#34027=REPRESENTATION('material name',(#34059),#61802);
#34028=REPRESENTATION('density',(#33934),#61802);
#34029=REPRESENTATION('material name',(#34060),#61803);
#34030=REPRESENTATION('density',(#33935),#61803);
#34031=REPRESENTATION('material name',(#34061),#61804);
#34032=REPRESENTATION('density',(#33936),#61804);
#34033=REPRESENTATION('material name',(#34062),#61806);
#34034=REPRESENTATION('density',(#33937),#61806);
#34035=REPRESENTATION('material name',(#34063),#61807);
#34036=REPRESENTATION('density',(#33938),#61807);
#34037=REPRESENTATION('material name',(#34064),#61809);
#34038=REPRESENTATION('density',(#33939),#61809);
#34039=REPRESENTATION('material name',(#34065),#61810);
#34040=REPRESENTATION('density',(#33940),#61810);
#34041=DESCRIPTIVE_REPRESENTATION_ITEM('Steel','Steel');
#34042=DESCRIPTIVE_REPRESENTATION_ITEM('Steel','Steel');
#34043=DESCRIPTIVE_REPRESENTATION_ITEM('Steel','Steel');
#34044=DESCRIPTIVE_REPRESENTATION_ITEM('Steel','Steel');
#34045=DESCRIPTIVE_REPRESENTATION_ITEM('Steel','Steel');
#34046=DESCRIPTIVE_REPRESENTATION_ITEM('Steel','Steel');
#34047=DESCRIPTIVE_REPRESENTATION_ITEM('Steel','Steel');
#34048=DESCRIPTIVE_REPRESENTATION_ITEM('Steel','Steel');
#34049=DESCRIPTIVE_REPRESENTATION_ITEM('Steel','Steel');
#34050=DESCRIPTIVE_REPRESENTATION_ITEM('Steel','Steel');
#34051=DESCRIPTIVE_REPRESENTATION_ITEM('Steel','Steel');
#34052=DESCRIPTIVE_REPRESENTATION_ITEM('Steel','Steel');
#34053=DESCRIPTIVE_REPRESENTATION_ITEM('Steel','Steel');
#34054=DESCRIPTIVE_REPRESENTATION_ITEM('Steel','Steel');
#34055=DESCRIPTIVE_REPRESENTATION_ITEM('Steel','Steel');
#34056=DESCRIPTIVE_REPRESENTATION_ITEM('Steel','Steel');
#34057=DESCRIPTIVE_REPRESENTATION_ITEM('Steel','Steel');
#34058=DESCRIPTIVE_REPRESENTATION_ITEM('Steel','Steel');
#34059=DESCRIPTIVE_REPRESENTATION_ITEM('Steel','Steel');
#34060=DESCRIPTIVE_REPRESENTATION_ITEM('Steel','Steel');
#34061=DESCRIPTIVE_REPRESENTATION_ITEM('Steel','Steel');
#34062=DESCRIPTIVE_REPRESENTATION_ITEM('Steel','Steel');
#34063=DESCRIPTIVE_REPRESENTATION_ITEM('Steel','Steel');
#34064=DESCRIPTIVE_REPRESENTATION_ITEM('Steel','Steel');
#34065=DESCRIPTIVE_REPRESENTATION_ITEM('Steel','Steel');
#34066=PROPERTY_DEFINITION('material property','material name',#62000);
#34067=PROPERTY_DEFINITION('material property','density of part',#62000);
#34068=PROPERTY_DEFINITION('material property','material name',#62001);
#34069=PROPERTY_DEFINITION('material property','density of part',#62001);
#34070=PROPERTY_DEFINITION('material property','material name',#62002);
#34071=PROPERTY_DEFINITION('material property','density of part',#62002);
#34072=PROPERTY_DEFINITION('material property','material name',#62003);
#34073=PROPERTY_DEFINITION('material property','density of part',#62003);
#34074=PROPERTY_DEFINITION('material property','material name',#62004);
#34075=PROPERTY_DEFINITION('material property','density of part',#62004);
#34076=PROPERTY_DEFINITION('material property','material name',#62005);
#34077=PROPERTY_DEFINITION('material property','density of part',#62005);
#34078=PROPERTY_DEFINITION('material property','material name',#62006);
#34079=PROPERTY_DEFINITION('material property','density of part',#62006);
#34080=PROPERTY_DEFINITION('material property','material name',#62007);
#34081=PROPERTY_DEFINITION('material property','density of part',#62007);
#34082=PROPERTY_DEFINITION('material property','material name',#62008);
#34083=PROPERTY_DEFINITION('material property','density of part',#62008);
#34084=PROPERTY_DEFINITION('material property','material name',#62009);
#34085=PROPERTY_DEFINITION('material property','density of part',#62009);
#34086=PROPERTY_DEFINITION('material property','material name',#62010);
#34087=PROPERTY_DEFINITION('material property','density of part',#62010);
#34088=PROPERTY_DEFINITION('material property','material name',#62012);
#34089=PROPERTY_DEFINITION('material property','density of part',#62012);
#34090=PROPERTY_DEFINITION('material property','material name',#62013);
#34091=PROPERTY_DEFINITION('material property','density of part',#62013);
#34092=PROPERTY_DEFINITION('material property','material name',#62014);
#34093=PROPERTY_DEFINITION('material property','density of part',#62014);
#34094=PROPERTY_DEFINITION('material property','material name',#62015);
#34095=PROPERTY_DEFINITION('material property','density of part',#62015);
#34096=PROPERTY_DEFINITION('material property','material name',#62016);
#34097=PROPERTY_DEFINITION('material property','density of part',#62016);
#34098=PROPERTY_DEFINITION('material property','material name',#62017);
#34099=PROPERTY_DEFINITION('material property','density of part',#62017);
#34100=PROPERTY_DEFINITION('material property','material name',#62019);
#34101=PROPERTY_DEFINITION('material property','density of part',#62019);
#34102=PROPERTY_DEFINITION('material property','material name',#62020);
#34103=PROPERTY_DEFINITION('material property','density of part',#62020);
#34104=PROPERTY_DEFINITION('material property','material name',#62021);
#34105=PROPERTY_DEFINITION('material property','density of part',#62021);
#34106=PROPERTY_DEFINITION('material property','material name',#62022);
#34107=PROPERTY_DEFINITION('material property','density of part',#62022);
#34108=PROPERTY_DEFINITION('material property','material name',#62024);
#34109=PROPERTY_DEFINITION('material property','density of part',#62024);
#34110=PROPERTY_DEFINITION('material property','material name',#62025);
#34111=PROPERTY_DEFINITION('material property','density of part',#62025);
#34112=PROPERTY_DEFINITION('material property','material name',#62027);
#34113=PROPERTY_DEFINITION('material property','density of part',#62027);
#34114=PROPERTY_DEFINITION('material property','material name',#62028);
#34115=PROPERTY_DEFINITION('material property','density of part',#62028);
#34116=AXIS2_PLACEMENT_3D('',#48837,#38174,#38175);
#34117=AXIS2_PLACEMENT_3D('',#48838,#38176,#38177);
#34118=AXIS2_PLACEMENT_3D('',#48839,#38178,#38179);
#34119=AXIS2_PLACEMENT_3D('',#48848,#38184,#38185);
#34120=AXIS2_PLACEMENT_3D('',#48857,#38190,#38191);
#34121=AXIS2_PLACEMENT_3D('',#48860,#38194,#38195);
#34122=AXIS2_PLACEMENT_3D('',#48867,#38198,#38199);
#34123=AXIS2_PLACEMENT_3D('',#48871,#38201,#38202);
#34124=AXIS2_PLACEMENT_3D('',#48877,#38205,#38206);
#34125=AXIS2_PLACEMENT_3D('',#48881,#38208,#38209);
#34126=AXIS2_PLACEMENT_3D('',#48887,#38212,#38213);
#34127=AXIS2_PLACEMENT_3D('',#48890,#38215,#38216);
#34128=AXIS2_PLACEMENT_3D('',#48891,#38217,#38218);
#34129=AXIS2_PLACEMENT_3D('',#48892,#38219,#38220);
#34130=AXIS2_PLACEMENT_3D('',#48893,#38221,#38222);
#34131=AXIS2_PLACEMENT_3D('',#48894,#38223,#38224);
#34132=AXIS2_PLACEMENT_3D('',#48900,#38228,#38229);
#34133=AXIS2_PLACEMENT_3D('',#48903,#38231,#38232);
#34134=AXIS2_PLACEMENT_3D('',#48904,#38233,#38234);
#34135=AXIS2_PLACEMENT_3D('',#48908,#38237,#38238);
#34136=AXIS2_PLACEMENT_3D('',#48912,#38241,#38242);
#34137=AXIS2_PLACEMENT_3D('',#48918,#38246,#38247);
#34138=AXIS2_PLACEMENT_3D('',#48921,#38249,#38250);
#34139=AXIS2_PLACEMENT_3D('',#48922,#38251,#38252);
#34140=AXIS2_PLACEMENT_3D('',#48926,#38255,#38256);
#34141=AXIS2_PLACEMENT_3D('',#48930,#38259,#38260);
#34142=AXIS2_PLACEMENT_3D('',#48932,#38261,#38262);
#34143=AXIS2_PLACEMENT_3D('',#48934,#38264,#38265);
#34144=AXIS2_PLACEMENT_3D('',#48935,#38266,#38267);
#34145=AXIS2_PLACEMENT_3D('',#48936,#38268,#38269);
#34146=AXIS2_PLACEMENT_3D('',#48940,#38271,#38272);
#34147=AXIS2_PLACEMENT_3D('',#48942,#38274,#38275);
#34148=AXIS2_PLACEMENT_3D('',#48946,#38278,#38279);
#34149=AXIS2_PLACEMENT_3D('',#48948,#38281,#38282);
#34150=AXIS2_PLACEMENT_3D('',#48952,#38285,#38286);
#34151=AXIS2_PLACEMENT_3D('',#48953,#38287,#38288);
#34152=AXIS2_PLACEMENT_3D('',#48954,#38289,#38290);
#34153=AXIS2_PLACEMENT_3D('',#48955,#38291,#38292);
#34154=AXIS2_PLACEMENT_3D('',#48956,#38293,#38294);
#34155=AXIS2_PLACEMENT_3D('',#48959,#38295,#38296);
#34156=AXIS2_PLACEMENT_3D('',#48963,#38298,#38299);
#34157=AXIS2_PLACEMENT_3D('',#48967,#38301,#38302);
#34158=AXIS2_PLACEMENT_3D('',#48971,#38304,#38305);
#34159=AXIS2_PLACEMENT_3D('',#48974,#38307,#38308);
#34160=AXIS2_PLACEMENT_3D('',#48976,#38309,#38310);
#34161=AXIS2_PLACEMENT_3D('',#48978,#38311,#38312);
#34162=AXIS2_PLACEMENT_3D('',#48980,#38313,#38314);
#34163=AXIS2_PLACEMENT_3D('',#48983,#38315,#38316);
#34164=AXIS2_PLACEMENT_3D('',#48987,#38318,#38319);
#34165=AXIS2_PLACEMENT_3D('',#48991,#38321,#38322);
#34166=AXIS2_PLACEMENT_3D('',#48995,#38324,#38325);
#34167=AXIS2_PLACEMENT_3D('',#48997,#38327,#38328);
#34168=AXIS2_PLACEMENT_3D('',#49000,#38329,#38330);
#34169=AXIS2_PLACEMENT_3D('',#49003,#38333,#38334);
#34170=AXIS2_PLACEMENT_3D('',#49005,#38335,#38336);
#34171=AXIS2_PLACEMENT_3D('',#49007,#38337,#38338);
#34172=AXIS2_PLACEMENT_3D('',#49008,#38339,#38340);
#34173=AXIS2_PLACEMENT_3D('',#49009,#38341,#38342);
#34174=AXIS2_PLACEMENT_3D('',#49013,#38344,#38345);
#34175=AXIS2_PLACEMENT_3D('',#49015,#38347,#38348);
#34176=AXIS2_PLACEMENT_3D('',#49018,#38349,#38350);
#34177=AXIS2_PLACEMENT_3D('',#49024,#38353,#38354);
#34178=AXIS2_PLACEMENT_3D('',#49029,#38357,#38358);
#34179=AXIS2_PLACEMENT_3D('',#49030,#38359,#38360);
#34180=AXIS2_PLACEMENT_3D('',#49033,#38361,#38362);
#34181=AXIS2_PLACEMENT_3D('',#49039,#38365,#38366);
#34182=AXIS2_PLACEMENT_3D('',#49044,#38369,#38370);
#34183=AXIS2_PLACEMENT_3D('',#49045,#38371,#38372);
#34184=AXIS2_PLACEMENT_3D('',#49048,#38373,#38374);
#34185=AXIS2_PLACEMENT_3D('',#49054,#38378,#38379);
#34186=AXIS2_PLACEMENT_3D('',#49055,#38380,#38381);
#34187=AXIS2_PLACEMENT_3D('',#49058,#38382,#38383);
#34188=AXIS2_PLACEMENT_3D('',#49064,#38386,#38387);
#34189=AXIS2_PLACEMENT_3D('',#49069,#38390,#38391);
#34190=AXIS2_PLACEMENT_3D('',#49070,#38392,#38393);
#34191=AXIS2_PLACEMENT_3D('',#49072,#38395,#38396);
#34192=AXIS2_PLACEMENT_3D('',#49074,#38398,#38399);
#34193=AXIS2_PLACEMENT_3D('',#49076,#38401,#38402);
#34194=AXIS2_PLACEMENT_3D('',#49078,#38404,#38405);
#34195=AXIS2_PLACEMENT_3D('',#49080,#38406,#38407);
#34196=AXIS2_PLACEMENT_3D('',#49082,#38408,#38409);
#34197=AXIS2_PLACEMENT_3D('',#49083,#38410,#38411);
#34198=AXIS2_PLACEMENT_3D('',#49131,#38412,#38413);
#34199=AXIS2_PLACEMENT_3D('',#49154,#38414,#38415);
#34200=AXIS2_PLACEMENT_3D('',#49157,#38416,#38417);
#34201=AXIS2_PLACEMENT_3D('',#49160,#38419,#38420);
#34202=AXIS2_PLACEMENT_3D('',#49172,#38421,#38422);
#34203=AXIS2_PLACEMENT_3D('',#49184,#38423,#38424);
#34204=AXIS2_PLACEMENT_3D('',#49196,#38425,#38426);
#34205=AXIS2_PLACEMENT_3D('',#49208,#38427,#38428);
#34206=AXIS2_PLACEMENT_3D('',#49220,#38429,#38430);
#34207=AXIS2_PLACEMENT_3D('',#49232,#38431,#38432);
#34208=AXIS2_PLACEMENT_3D('',#49243,#38433,#38434);
#34209=AXIS2_PLACEMENT_3D('',#49244,#38435,#38436);
#34210=AXIS2_PLACEMENT_3D('',#49245,#38437,#38438);
#34211=AXIS2_PLACEMENT_3D('',#49248,#38439,#38440);
#34212=AXIS2_PLACEMENT_3D('',#49249,#38441,#38442);
#34213=AXIS2_PLACEMENT_3D('',#49250,#38443,#38444);
#34214=AXIS2_PLACEMENT_3D('',#49251,#38445,#38446);
#34215=AXIS2_PLACEMENT_3D('',#49257,#38450,#38451);
#34216=AXIS2_PLACEMENT_3D('',#49260,#38452,#38453);
#34217=AXIS2_PLACEMENT_3D('',#49266,#38457,#38458);
#34218=AXIS2_PLACEMENT_3D('',#49269,#38459,#38460);
#34219=AXIS2_PLACEMENT_3D('',#49275,#38464,#38465);
#34220=AXIS2_PLACEMENT_3D('',#49278,#38466,#38467);
#34221=AXIS2_PLACEMENT_3D('',#49284,#38471,#38472);
#34222=AXIS2_PLACEMENT_3D('',#49285,#38473,#38474);
#34223=AXIS2_PLACEMENT_3D('',#49343,#38476,#38477);
#34224=AXIS2_PLACEMENT_3D('',#49344,#38478,#38479);
#34225=AXIS2_PLACEMENT_3D('',#49345,#38480,#38481);
#34226=AXIS2_PLACEMENT_3D('',#49346,#38482,#38483);
#34227=AXIS2_PLACEMENT_3D('',#49348,#38484,#38485);
#34228=AXIS2_PLACEMENT_3D('',#49349,#38486,#38487);
#34229=AXIS2_PLACEMENT_3D('',#49350,#38488,#38489);
#34230=AXIS2_PLACEMENT_3D('',#49353,#38491,#38492);
#34231=AXIS2_PLACEMENT_3D('',#49354,#38493,#38494);
#34232=AXIS2_PLACEMENT_3D('',#49356,#38495,#38496);
#34233=AXIS2_PLACEMENT_3D('',#49357,#38497,#38498);
#34234=AXIS2_PLACEMENT_3D('',#49358,#38499,#38500);
#34235=AXIS2_PLACEMENT_3D('',#49361,#38503,#38504);
#34236=AXIS2_PLACEMENT_3D('',#49391,#38509,#38510);
#34237=AXIS2_PLACEMENT_3D('',#49392,#38511,#38512);
#34238=AXIS2_PLACEMENT_3D('',#49393,#38513,#38514);
#34239=AXIS2_PLACEMENT_3D('',#49394,#38515,#38516);
#34240=AXIS2_PLACEMENT_3D('',#49396,#38517,#38518);
#34241=AXIS2_PLACEMENT_3D('',#49397,#38519,#38520);
#34242=AXIS2_PLACEMENT_3D('',#49398,#38521,#38522);
#34243=AXIS2_PLACEMENT_3D('',#49400,#38524,#38525);
#34244=AXIS2_PLACEMENT_3D('',#49578,#38528,#38529);
#34245=AXIS2_PLACEMENT_3D('',#49579,#38530,#38531);
#34246=AXIS2_PLACEMENT_3D('',#49581,#38532,#38533);
#34247=AXIS2_PLACEMENT_3D('',#49583,#38535,#38536);
#34248=AXIS2_PLACEMENT_3D('',#49584,#38537,#38538);
#34249=AXIS2_PLACEMENT_3D('',#49585,#38539,#38540);
#34250=AXIS2_PLACEMENT_3D('',#49644,#38541,#38542);
#34251=AXIS2_PLACEMENT_3D('',#49645,#38543,#38544);
#34252=AXIS2_PLACEMENT_3D('',#49646,#38545,#38546);
#34253=AXIS2_PLACEMENT_3D('',#49647,#38547,#38548);
#34254=AXIS2_PLACEMENT_3D('',#49648,#38549,#38550);
#34255=AXIS2_PLACEMENT_3D('',#49649,#38551,#38552);
#34256=AXIS2_PLACEMENT_3D('',#49650,#38553,#38554);
#34257=AXIS2_PLACEMENT_3D('',#49651,#38555,#38556);
#34258=AXIS2_PLACEMENT_3D('',#49689,#38557,#38558);
#34259=AXIS2_PLACEMENT_3D('',#49699,#38559,#38560);
#34260=AXIS2_PLACEMENT_3D('',#49702,#38562,#38563);
#34261=AXIS2_PLACEMENT_3D('',#49703,#38564,#38565);
#34262=AXIS2_PLACEMENT_3D('',#49704,#38566,#38567);
#34263=AXIS2_PLACEMENT_3D('',#49813,#38568,#38569);
#34264=AXIS2_PLACEMENT_3D('',#49814,#38570,#38571);
#34265=AXIS2_PLACEMENT_3D('',#49815,#38572,#38573);
#34266=AXIS2_PLACEMENT_3D('',#49968,#38574,#38575);
#34267=AXIS2_PLACEMENT_3D('',#49970,#38576,#38577);
#34268=AXIS2_PLACEMENT_3D('',#49972,#38579,#38580);
#34269=AXIS2_PLACEMENT_3D('',#49973,#38581,#38582);
#34270=AXIS2_PLACEMENT_3D('',#49974,#38583,#38584);
#34271=AXIS2_PLACEMENT_3D('',#50020,#38585,#38586);
#34272=AXIS2_PLACEMENT_3D('',#50021,#38587,#38588);
#34273=AXIS2_PLACEMENT_3D('',#50022,#38589,#38590);
#34274=AXIS2_PLACEMENT_3D('',#50023,#38591,#38592);
#34275=AXIS2_PLACEMENT_3D('',#50024,#38593,#38594);
#34276=AXIS2_PLACEMENT_3D('',#50025,#38595,#38596);
#34277=AXIS2_PLACEMENT_3D('',#50026,#38597,#38598);
#34278=AXIS2_PLACEMENT_3D('',#50027,#38599,#38600);
#34279=AXIS2_PLACEMENT_3D('',#50028,#38601,#38602);
#34280=AXIS2_PLACEMENT_3D('',#50029,#38603,#38604);
#34281=AXIS2_PLACEMENT_3D('',#50030,#38605,#38606);
#34282=AXIS2_PLACEMENT_3D('',#50031,#38607,#38608);
#34283=AXIS2_PLACEMENT_3D('',#50091,#38609,#38610);
#34284=AXIS2_PLACEMENT_3D('',#50092,#38611,#38612);
#34285=AXIS2_PLACEMENT_3D('',#50093,#38613,#38614);
#34286=AXIS2_PLACEMENT_3D('',#50095,#38615,#38616);
#34287=AXIS2_PLACEMENT_3D('',#50097,#38618,#38619);
#34288=AXIS2_PLACEMENT_3D('',#50098,#38620,#38621);
#34289=AXIS2_PLACEMENT_3D('',#50154,#38622,#38623);
#34290=AXIS2_PLACEMENT_3D('',#50254,#38624,#38625);
#34291=AXIS2_PLACEMENT_3D('',#50255,#38626,#38627);
#34292=AXIS2_PLACEMENT_3D('',#50258,#38629,#38630);
#34293=AXIS2_PLACEMENT_3D('',#50259,#38631,#38632);
#34294=AXIS2_PLACEMENT_3D('',#50273,#38635,#38636);
#34295=AXIS2_PLACEMENT_3D('',#50275,#38637,#38638);
#34296=AXIS2_PLACEMENT_3D('',#50277,#38640,#38641);
#34297=AXIS2_PLACEMENT_3D('',#50278,#38642,#38643);
#34298=AXIS2_PLACEMENT_3D('',#50279,#38644,#38645);
#34299=AXIS2_PLACEMENT_3D('',#50280,#38646,#38647);
#34300=AXIS2_PLACEMENT_3D('',#50282,#38648,#38649);
#34301=AXIS2_PLACEMENT_3D('',#50284,#38651,#38652);
#34302=AXIS2_PLACEMENT_3D('',#50310,#38655,#38656);
#34303=AXIS2_PLACEMENT_3D('',#50311,#38657,#38658);
#34304=AXIS2_PLACEMENT_3D('',#50312,#38659,#38660);
#34305=AXIS2_PLACEMENT_3D('',#50314,#38661,#38662);
#34306=AXIS2_PLACEMENT_3D('',#50315,#38663,#38664);
#34307=AXIS2_PLACEMENT_3D('',#50316,#38665,#38666);
#34308=AXIS2_PLACEMENT_3D('',#50364,#38668,#38669);
#34309=AXIS2_PLACEMENT_3D('',#50365,#38670,#38671);
#34310=AXIS2_PLACEMENT_3D('',#50366,#38672,#38673);
#34311=AXIS2_PLACEMENT_3D('',#50367,#38674,#38675);
#34312=AXIS2_PLACEMENT_3D('',#50405,#38676,#38677);
#34313=AXIS2_PLACEMENT_3D('',#50428,#38678,#38679);
#34314=AXIS2_PLACEMENT_3D('',#50431,#38681,#38682);
#34315=AXIS2_PLACEMENT_3D('',#50432,#38683,#38684);
#34316=AXIS2_PLACEMENT_3D('',#50433,#38685,#38686);
#34317=AXIS2_PLACEMENT_3D('',#50542,#38687,#38688);
#34318=AXIS2_PLACEMENT_3D('',#50543,#38689,#38690);
#34319=AXIS2_PLACEMENT_3D('',#50544,#38691,#38692);
#34320=AXIS2_PLACEMENT_3D('',#50545,#38693,#38694);
#34321=AXIS2_PLACEMENT_3D('',#50546,#38695,#38696);
#34322=AXIS2_PLACEMENT_3D('',#50547,#38697,#38698);
#34323=AXIS2_PLACEMENT_3D('',#50548,#38699,#38700);
#34324=AXIS2_PLACEMENT_3D('',#50549,#38701,#38702);
#34325=AXIS2_PLACEMENT_3D('',#50550,#38703,#38704);
#34326=AXIS2_PLACEMENT_3D('',#50650,#38705,#38706);
#34327=AXIS2_PLACEMENT_3D('',#50651,#38707,#38708);
#34328=AXIS2_PLACEMENT_3D('',#50652,#38709,#38710);
#34329=AXIS2_PLACEMENT_3D('',#50698,#38711,#38712);
#34330=AXIS2_PLACEMENT_3D('',#50763,#38713,#38714);
#34331=AXIS2_PLACEMENT_3D('',#50765,#38715,#38716);
#34332=AXIS2_PLACEMENT_3D('',#50767,#38718,#38719);
#34333=AXIS2_PLACEMENT_3D('',#50768,#38720,#38721);
#34334=AXIS2_PLACEMENT_3D('',#50769,#38722,#38723);
#34335=AXIS2_PLACEMENT_3D('',#50770,#38724,#38725);
#34336=AXIS2_PLACEMENT_3D('',#50816,#38726,#38727);
#34337=AXIS2_PLACEMENT_3D('',#50817,#38728,#38729);
#34338=AXIS2_PLACEMENT_3D('',#50818,#38730,#38731);
#34339=AXIS2_PLACEMENT_3D('',#50819,#38732,#38733);
#34340=AXIS2_PLACEMENT_3D('',#50820,#38734,#38735);
#34341=AXIS2_PLACEMENT_3D('',#50821,#38736,#38737);
#34342=AXIS2_PLACEMENT_3D('',#50822,#38738,#38739);
#34343=AXIS2_PLACEMENT_3D('',#50823,#38740,#38741);
#34344=AXIS2_PLACEMENT_3D('',#50868,#38742,#38743);
#34345=AXIS2_PLACEMENT_3D('',#50870,#38744,#38745);
#34346=AXIS2_PLACEMENT_3D('',#50871,#38746,#38747);
#34347=AXIS2_PLACEMENT_3D('',#50872,#38748,#38749);
#34348=AXIS2_PLACEMENT_3D('',#50874,#38750,#38751);
#34349=AXIS2_PLACEMENT_3D('',#50875,#38752,#38753);
#34350=AXIS2_PLACEMENT_3D('',#50878,#38754,#38755);
#34351=AXIS2_PLACEMENT_3D('',#50879,#38756,#38757);
#34352=AXIS2_PLACEMENT_3D('',#50880,#38758,#38759);
#34353=AXIS2_PLACEMENT_3D('',#50881,#38760,#38761);
#34354=AXIS2_PLACEMENT_3D('',#50883,#38762,#38763);
#34355=AXIS2_PLACEMENT_3D('',#50885,#38765,#38766);
#34356=AXIS2_PLACEMENT_3D('',#50887,#38767,#38768);
#34357=AXIS2_PLACEMENT_3D('',#50888,#38769,#38770);
#34358=AXIS2_PLACEMENT_3D('',#50890,#38771,#38772);
#34359=AXIS2_PLACEMENT_3D('',#50892,#38774,#38775);
#34360=AXIS2_PLACEMENT_3D('',#50894,#38776,#38777);
#34361=AXIS2_PLACEMENT_3D('',#50895,#38778,#38779);
#34362=AXIS2_PLACEMENT_3D('',#50897,#38780,#38781);
#34363=AXIS2_PLACEMENT_3D('',#50899,#38783,#38784);
#34364=AXIS2_PLACEMENT_3D('',#50901,#38785,#38786);
#34365=AXIS2_PLACEMENT_3D('',#50902,#38787,#38788);
#34366=AXIS2_PLACEMENT_3D('',#50904,#38789,#38790);
#34367=AXIS2_PLACEMENT_3D('',#50906,#38792,#38793);
#34368=AXIS2_PLACEMENT_3D('',#50908,#38794,#38795);
#34369=AXIS2_PLACEMENT_3D('',#50909,#38796,#38797);
#34370=AXIS2_PLACEMENT_3D('',#50911,#38798,#38799);
#34371=AXIS2_PLACEMENT_3D('',#50913,#38801,#38802);
#34372=AXIS2_PLACEMENT_3D('',#50915,#38803,#38804);
#34373=AXIS2_PLACEMENT_3D('',#50916,#38805,#38806);
#34374=AXIS2_PLACEMENT_3D('',#50918,#38807,#38808);
#34375=AXIS2_PLACEMENT_3D('',#50920,#38810,#38811);
#34376=AXIS2_PLACEMENT_3D('',#50922,#38812,#38813);
#34377=AXIS2_PLACEMENT_3D('',#50923,#38814,#38815);
#34378=AXIS2_PLACEMENT_3D('',#50925,#38816,#38817);
#34379=AXIS2_PLACEMENT_3D('',#50927,#38819,#38820);
#34380=AXIS2_PLACEMENT_3D('',#50930,#38821,#38822);
#34381=AXIS2_PLACEMENT_3D('',#50934,#38824,#38825);
#34382=AXIS2_PLACEMENT_3D('',#50938,#38827,#38828);
#34383=AXIS2_PLACEMENT_3D('',#50942,#38830,#38831);
#34384=AXIS2_PLACEMENT_3D('',#50944,#38833,#38834);
#34385=AXIS2_PLACEMENT_3D('',#50947,#38837,#38838);
#34386=AXIS2_PLACEMENT_3D('',#50949,#38840,#38841);
#34387=AXIS2_PLACEMENT_3D('',#50951,#38843,#38844);
#34388=AXIS2_PLACEMENT_3D('',#50953,#38846,#38847);
#34389=AXIS2_PLACEMENT_3D('',#50955,#38849,#38850);
#34390=AXIS2_PLACEMENT_3D('',#50957,#38852,#38853);
#34391=AXIS2_PLACEMENT_3D('',#50959,#38855,#38856);
#34392=AXIS2_PLACEMENT_3D('',#50960,#38857,#38858);
#34393=AXIS2_PLACEMENT_3D('',#50961,#38859,#38860);
#34394=AXIS2_PLACEMENT_3D('',#50964,#38861,#38862);
#34395=AXIS2_PLACEMENT_3D('',#50965,#38863,#38864);
#34396=AXIS2_PLACEMENT_3D('',#50967,#38865,#38866);
#34397=AXIS2_PLACEMENT_3D('',#50968,#38867,#38868);
#34398=AXIS2_PLACEMENT_3D('',#50969,#38869,#38870);
#34399=AXIS2_PLACEMENT_3D('',#50972,#38871,#38872);
#34400=AXIS2_PLACEMENT_3D('',#50973,#38873,#38874);
#34401=AXIS2_PLACEMENT_3D('',#50975,#38876,#38877);
#34402=AXIS2_PLACEMENT_3D('',#50977,#38878,#38879);
#34403=AXIS2_PLACEMENT_3D('',#50978,#38880,#38881);
#34404=AXIS2_PLACEMENT_3D('',#50981,#38883,#38884);
#34405=AXIS2_PLACEMENT_3D('',#50982,#38885,#38886);
#34406=AXIS2_PLACEMENT_3D('',#50983,#38887,#38888);
#34407=AXIS2_PLACEMENT_3D('',#50986,#38889,#38890);
#34408=AXIS2_PLACEMENT_3D('',#50987,#38891,#38892);
#34409=AXIS2_PLACEMENT_3D('',#50989,#38893,#38894);
#34410=AXIS2_PLACEMENT_3D('',#50990,#38895,#38896);
#34411=AXIS2_PLACEMENT_3D('',#50991,#38897,#38898);
#34412=AXIS2_PLACEMENT_3D('',#51004,#38905,#38906);
#34413=AXIS2_PLACEMENT_3D('',#51006,#38908,#38909);
#34414=AXIS2_PLACEMENT_3D('',#51014,#38912,#38913);
#34415=AXIS2_PLACEMENT_3D('',#51020,#38915,#38916);
#34416=AXIS2_PLACEMENT_3D('',#51026,#38918,#38919);
#34417=AXIS2_PLACEMENT_3D('',#51032,#38921,#38922);
#34418=AXIS2_PLACEMENT_3D('',#51042,#38924,#38925);
#34419=AXIS2_PLACEMENT_3D('',#51046,#38926,#38927);
#34420=AXIS2_PLACEMENT_3D('',#51049,#38929,#38930);
#34421=AXIS2_PLACEMENT_3D('',#51050,#38931,#38932);
#34422=AXIS2_PLACEMENT_3D('',#51053,#38933,#38934);
#34423=AXIS2_PLACEMENT_3D('',#51054,#38935,#38936);
#34424=AXIS2_PLACEMENT_3D('',#51056,#38937,#38938);
#34425=AXIS2_PLACEMENT_3D('',#51057,#38939,#38940);
#34426=AXIS2_PLACEMENT_3D('',#51058,#38941,#38942);
#34427=AXIS2_PLACEMENT_3D('',#51061,#38943,#38944);
#34428=AXIS2_PLACEMENT_3D('',#51062,#38945,#38946);
#34429=AXIS2_PLACEMENT_3D('',#51064,#38948,#38949);
#34430=AXIS2_PLACEMENT_3D('',#51066,#38950,#38951);
#34431=AXIS2_PLACEMENT_3D('',#51067,#38952,#38953);
#34432=AXIS2_PLACEMENT_3D('',#51070,#38955,#38956);
#34433=AXIS2_PLACEMENT_3D('',#51071,#38957,#38958);
#34434=AXIS2_PLACEMENT_3D('',#51072,#38959,#38960);
#34435=AXIS2_PLACEMENT_3D('',#51075,#38961,#38962);
#34436=AXIS2_PLACEMENT_3D('',#51076,#38963,#38964);
#34437=AXIS2_PLACEMENT_3D('',#51078,#38965,#38966);
#34438=AXIS2_PLACEMENT_3D('',#51079,#38967,#38968);
#34439=AXIS2_PLACEMENT_3D('',#51080,#38969,#38970);
#34440=AXIS2_PLACEMENT_3D('',#51093,#38977,#38978);
#34441=AXIS2_PLACEMENT_3D('',#51095,#38980,#38981);
#34442=AXIS2_PLACEMENT_3D('',#51103,#38984,#38985);
#34443=AXIS2_PLACEMENT_3D('',#51109,#38987,#38988);
#34444=AXIS2_PLACEMENT_3D('',#51115,#38990,#38991);
#34445=AXIS2_PLACEMENT_3D('',#51121,#38993,#38994);
#34446=AXIS2_PLACEMENT_3D('',#51131,#38996,#38997);
#34447=AXIS2_PLACEMENT_3D('',#51135,#38998,#38999);
#34448=AXIS2_PLACEMENT_3D('',#51138,#39001,#39002);
#34449=AXIS2_PLACEMENT_3D('',#51139,#39003,#39004);
#34450=AXIS2_PLACEMENT_3D('',#51142,#39005,#39006);
#34451=AXIS2_PLACEMENT_3D('',#51143,#39007,#39008);
#34452=AXIS2_PLACEMENT_3D('',#51145,#39009,#39010);
#34453=AXIS2_PLACEMENT_3D('',#51146,#39011,#39012);
#34454=AXIS2_PLACEMENT_3D('',#51147,#39013,#39014);
#34455=AXIS2_PLACEMENT_3D('',#51150,#39015,#39016);
#34456=AXIS2_PLACEMENT_3D('',#51151,#39017,#39018);
#34457=AXIS2_PLACEMENT_3D('',#51153,#39020,#39021);
#34458=AXIS2_PLACEMENT_3D('',#51155,#39022,#39023);
#34459=AXIS2_PLACEMENT_3D('',#51156,#39024,#39025);
#34460=AXIS2_PLACEMENT_3D('',#51159,#39027,#39028);
#34461=AXIS2_PLACEMENT_3D('',#51160,#39029,#39030);
#34462=AXIS2_PLACEMENT_3D('',#51161,#39031,#39032);
#34463=AXIS2_PLACEMENT_3D('',#51164,#39033,#39034);
#34464=AXIS2_PLACEMENT_3D('',#51165,#39035,#39036);
#34465=AXIS2_PLACEMENT_3D('',#51167,#39037,#39038);
#34466=AXIS2_PLACEMENT_3D('',#51168,#39039,#39040);
#34467=AXIS2_PLACEMENT_3D('',#51169,#39041,#39042);
#34468=AXIS2_PLACEMENT_3D('',#51182,#39049,#39050);
#34469=AXIS2_PLACEMENT_3D('',#51184,#39052,#39053);
#34470=AXIS2_PLACEMENT_3D('',#51192,#39056,#39057);
#34471=AXIS2_PLACEMENT_3D('',#51198,#39059,#39060);
#34472=AXIS2_PLACEMENT_3D('',#51204,#39062,#39063);
#34473=AXIS2_PLACEMENT_3D('',#51210,#39065,#39066);
#34474=AXIS2_PLACEMENT_3D('',#51220,#39068,#39069);
#34475=AXIS2_PLACEMENT_3D('',#51224,#39070,#39071);
#34476=AXIS2_PLACEMENT_3D('',#51227,#39073,#39074);
#34477=AXIS2_PLACEMENT_3D('',#51228,#39075,#39076);
#34478=AXIS2_PLACEMENT_3D('',#51231,#39077,#39078);
#34479=AXIS2_PLACEMENT_3D('',#51232,#39079,#39080);
#34480=AXIS2_PLACEMENT_3D('',#51234,#39081,#39082);
#34481=AXIS2_PLACEMENT_3D('',#51235,#39083,#39084);
#34482=AXIS2_PLACEMENT_3D('',#51236,#39085,#39086);
#34483=AXIS2_PLACEMENT_3D('',#51239,#39087,#39088);
#34484=AXIS2_PLACEMENT_3D('',#51240,#39089,#39090);
#34485=AXIS2_PLACEMENT_3D('',#51242,#39092,#39093);
#34486=AXIS2_PLACEMENT_3D('',#51244,#39094,#39095);
#34487=AXIS2_PLACEMENT_3D('',#51245,#39096,#39097);
#34488=AXIS2_PLACEMENT_3D('',#51248,#39099,#39100);
#34489=AXIS2_PLACEMENT_3D('',#51249,#39101,#39102);
#34490=AXIS2_PLACEMENT_3D('',#51250,#39103,#39104);
#34491=AXIS2_PLACEMENT_3D('',#51257,#39105,#39106);
#34492=AXIS2_PLACEMENT_3D('',#51261,#39107,#39108);
#34493=AXIS2_PLACEMENT_3D('',#51270,#39109,#39110);
#34494=AXIS2_PLACEMENT_3D('',#51271,#39111,#39112);
#34495=AXIS2_PLACEMENT_3D('',#51277,#39113,#39114);
#34496=AXIS2_PLACEMENT_3D('',#51281,#39115,#39116);
#34497=AXIS2_PLACEMENT_3D('',#51290,#39117,#39118);
#34498=AXIS2_PLACEMENT_3D('',#51291,#39119,#39120);
#34499=AXIS2_PLACEMENT_3D('',#51297,#39121,#39122);
#34500=AXIS2_PLACEMENT_3D('',#51301,#39123,#39124);
#34501=AXIS2_PLACEMENT_3D('',#51309,#39125,#39126);
#34502=AXIS2_PLACEMENT_3D('',#51310,#39127,#39128);
#34503=AXIS2_PLACEMENT_3D('',#51316,#39132,#39133);
#34504=AXIS2_PLACEMENT_3D('',#51320,#39136,#39137);
#34505=AXIS2_PLACEMENT_3D('',#51324,#39140,#39141);
#34506=AXIS2_PLACEMENT_3D('',#51331,#39145,#39146);
#34507=AXIS2_PLACEMENT_3D('',#51332,#39147,#39148);
#34508=AXIS2_PLACEMENT_3D('',#51334,#39150,#39151);
#34509=AXIS2_PLACEMENT_3D('',#51336,#39153,#39154);
#34510=AXIS2_PLACEMENT_3D('',#51337,#39155,#39156);
#34511=AXIS2_PLACEMENT_3D('',#51338,#39157,#39158);
#34512=AXIS2_PLACEMENT_3D('',#51340,#39160,#39161);
#34513=AXIS2_PLACEMENT_3D('',#51341,#39162,#39163);
#34514=AXIS2_PLACEMENT_3D('',#51350,#39168,#39169);
#34515=AXIS2_PLACEMENT_3D('',#51356,#39173,#39174);
#34516=AXIS2_PLACEMENT_3D('',#51362,#39178,#39179);
#34517=AXIS2_PLACEMENT_3D('',#51365,#39182,#39183);
#34518=AXIS2_PLACEMENT_3D('',#51374,#39188,#39189);
#34519=AXIS2_PLACEMENT_3D('',#51380,#39193,#39194);
#34520=AXIS2_PLACEMENT_3D('',#51386,#39198,#39199);
#34521=AXIS2_PLACEMENT_3D('',#51389,#39202,#39203);
#34522=AXIS2_PLACEMENT_3D('',#51390,#39204,#39205);
#34523=AXIS2_PLACEMENT_3D('',#51399,#39210,#39211);
#34524=AXIS2_PLACEMENT_3D('',#51405,#39215,#39216);
#34525=AXIS2_PLACEMENT_3D('',#51411,#39220,#39221);
#34526=AXIS2_PLACEMENT_3D('',#51414,#39224,#39225);
#34527=AXIS2_PLACEMENT_3D('',#51415,#39226,#39227);
#34528=AXIS2_PLACEMENT_3D('',#51416,#39228,#39229);
#34529=AXIS2_PLACEMENT_3D('',#51417,#39230,#39231);
#34530=AXIS2_PLACEMENT_3D('',#51419,#39232,#39233);
#34531=AXIS2_PLACEMENT_3D('',#51422,#39235,#39236);
#34532=AXIS2_PLACEMENT_3D('',#51423,#39237,#39238);
#34533=AXIS2_PLACEMENT_3D('',#51425,#39239,#39240);
#34534=AXIS2_PLACEMENT_3D('',#51428,#39242,#39243);
#34535=AXIS2_PLACEMENT_3D('',#51429,#39244,#39245);
#34536=AXIS2_PLACEMENT_3D('',#51431,#39246,#39247);
#34537=AXIS2_PLACEMENT_3D('',#51434,#39249,#39250);
#34538=AXIS2_PLACEMENT_3D('',#51435,#39251,#39252);
#34539=AXIS2_PLACEMENT_3D('',#51437,#39253,#39254);
#34540=AXIS2_PLACEMENT_3D('',#51440,#39256,#39257);
#34541=AXIS2_PLACEMENT_3D('',#51441,#39258,#39259);
#34542=AXIS2_PLACEMENT_3D('',#51443,#39260,#39261);
#34543=AXIS2_PLACEMENT_3D('',#51446,#39263,#39264);
#34544=AXIS2_PLACEMENT_3D('',#51447,#39265,#39266);
#34545=AXIS2_PLACEMENT_3D('',#51449,#39267,#39268);
#34546=AXIS2_PLACEMENT_3D('',#51452,#39270,#39271);
#34547=AXIS2_PLACEMENT_3D('',#51453,#39272,#39273);
#34548=AXIS2_PLACEMENT_3D('',#51470,#39282,#39283);
#34549=AXIS2_PLACEMENT_3D('',#51476,#39287,#39288);
#34550=AXIS2_PLACEMENT_3D('',#51480,#39291,#39292);
#34551=AXIS2_PLACEMENT_3D('',#51484,#39295,#39296);
#34552=AXIS2_PLACEMENT_3D('',#51486,#39298,#39299);
#34553=AXIS2_PLACEMENT_3D('',#51492,#39303,#39304);
#34554=AXIS2_PLACEMENT_3D('',#51500,#39309,#39310);
#34555=AXIS2_PLACEMENT_3D('',#51509,#39315,#39316);
#34556=AXIS2_PLACEMENT_3D('',#51515,#39320,#39321);
#34557=AXIS2_PLACEMENT_3D('',#51524,#39326,#39327);
#34558=AXIS2_PLACEMENT_3D('',#51530,#39331,#39332);
#34559=AXIS2_PLACEMENT_3D('',#51536,#39336,#39337);
#34560=AXIS2_PLACEMENT_3D('',#51542,#39341,#39342);
#34561=AXIS2_PLACEMENT_3D('',#51545,#39345,#39346);
#34562=AXIS2_PLACEMENT_3D('',#51548,#39349,#39350);
#34563=AXIS2_PLACEMENT_3D('',#51549,#39351,#39352);
#34564=AXIS2_PLACEMENT_3D('',#51553,#39355,#39356);
#34565=AXIS2_PLACEMENT_3D('',#51557,#39359,#39360);
#34566=AXIS2_PLACEMENT_3D('',#51561,#39363,#39364);
#34567=AXIS2_PLACEMENT_3D('',#51563,#39366,#39367);
#34568=AXIS2_PLACEMENT_3D('',#51564,#39368,#39369);
#34569=AXIS2_PLACEMENT_3D('',#51603,#39370,#39371);
#34570=AXIS2_PLACEMENT_3D('',#51604,#39372,#39373);
#34571=AXIS2_PLACEMENT_3D('',#51705,#39374,#39375);
#34572=AXIS2_PLACEMENT_3D('',#51711,#39379,#39380);
#34573=AXIS2_PLACEMENT_3D('',#51715,#39383,#39384);
#34574=AXIS2_PLACEMENT_3D('',#51719,#39387,#39388);
#34575=AXIS2_PLACEMENT_3D('',#51722,#39389,#39390);
#34576=AXIS2_PLACEMENT_3D('',#51724,#39392,#39393);
#34577=AXIS2_PLACEMENT_3D('',#51747,#39395,#39396);
#34578=AXIS2_PLACEMENT_3D('',#51750,#39397,#39398);
#34579=AXIS2_PLACEMENT_3D('',#51765,#39400,#39401);
#34580=AXIS2_PLACEMENT_3D('',#51786,#39402,#39403);
#34581=AXIS2_PLACEMENT_3D('',#51801,#39405,#39406);
#34582=AXIS2_PLACEMENT_3D('',#51827,#39409,#39410);
#34583=AXIS2_PLACEMENT_3D('',#51851,#39413,#39414);
#34584=AXIS2_PLACEMENT_3D('',#51895,#39417,#39418);
#34585=AXIS2_PLACEMENT_3D('',#51922,#39421,#39422);
#34586=AXIS2_PLACEMENT_3D('',#51928,#39426,#39427);
#34587=AXIS2_PLACEMENT_3D('',#51934,#39431,#39432);
#34588=AXIS2_PLACEMENT_3D('',#51937,#39433,#39434);
#34589=AXIS2_PLACEMENT_3D('',#51951,#39436,#39437);
#34590=AXIS2_PLACEMENT_3D('',#51962,#39438,#39439);
#34591=AXIS2_PLACEMENT_3D('',#51964,#39440,#39441);
#34592=AXIS2_PLACEMENT_3D('',#51965,#39442,#39443);
#34593=AXIS2_PLACEMENT_3D('',#51967,#39444,#39445);
#34594=AXIS2_PLACEMENT_3D('',#51982,#39447,#39448);
#34595=AXIS2_PLACEMENT_3D('',#52009,#39452,#39453);
#34596=AXIS2_PLACEMENT_3D('',#52010,#39454,#39455);
#34597=AXIS2_PLACEMENT_3D('',#52013,#39456,#39457);
#34598=AXIS2_PLACEMENT_3D('',#52015,#39458,#39459);
#34599=AXIS2_PLACEMENT_3D('',#52017,#39460,#39461);
#34600=AXIS2_PLACEMENT_3D('',#52019,#39462,#39463);
#34601=AXIS2_PLACEMENT_3D('',#52021,#39464,#39465);
#34602=AXIS2_PLACEMENT_3D('',#52023,#39466,#39467);
#34603=AXIS2_PLACEMENT_3D('',#52025,#39468,#39469);
#34604=AXIS2_PLACEMENT_3D('',#52027,#39470,#39471);
#34605=AXIS2_PLACEMENT_3D('',#52029,#39472,#39473);
#34606=AXIS2_PLACEMENT_3D('',#52031,#39474,#39475);
#34607=AXIS2_PLACEMENT_3D('',#52033,#39476,#39477);
#34608=AXIS2_PLACEMENT_3D('',#52034,#39478,#39479);
#34609=AXIS2_PLACEMENT_3D('',#52035,#39480,#39481);
#34610=AXIS2_PLACEMENT_3D('',#52038,#39482,#39483);
#34611=AXIS2_PLACEMENT_3D('',#52044,#39487,#39488);
#34612=AXIS2_PLACEMENT_3D('',#52046,#39489,#39490);
#34613=AXIS2_PLACEMENT_3D('',#52050,#39493,#39494);
#34614=AXIS2_PLACEMENT_3D('',#52051,#39495,#39496);
#34615=AXIS2_PLACEMENT_3D('',#52052,#39497,#39498);
#34616=AXIS2_PLACEMENT_3D('',#52054,#39499,#39500);
#34617=AXIS2_PLACEMENT_3D('',#52056,#39502,#39503);
#34618=AXIS2_PLACEMENT_3D('',#52057,#39504,#39505);
#34619=AXIS2_PLACEMENT_3D('',#52060,#39507,#39508);
#34620=AXIS2_PLACEMENT_3D('',#52061,#39509,#39510);
#34621=AXIS2_PLACEMENT_3D('',#52064,#39511,#39512);
#34622=AXIS2_PLACEMENT_3D('',#52070,#39516,#39517);
#34623=AXIS2_PLACEMENT_3D('',#52072,#39518,#39519);
#34624=AXIS2_PLACEMENT_3D('',#52076,#39522,#39523);
#34625=AXIS2_PLACEMENT_3D('',#52078,#39524,#39525);
#34626=AXIS2_PLACEMENT_3D('',#52082,#39528,#39529);
#34627=AXIS2_PLACEMENT_3D('',#52084,#39530,#39531);
#34628=AXIS2_PLACEMENT_3D('',#52088,#39534,#39535);
#34629=AXIS2_PLACEMENT_3D('',#52090,#39536,#39537);
#34630=AXIS2_PLACEMENT_3D('',#52094,#39540,#39541);
#34631=AXIS2_PLACEMENT_3D('',#52096,#39542,#39543);
#34632=AXIS2_PLACEMENT_3D('',#52100,#39546,#39547);
#34633=AXIS2_PLACEMENT_3D('',#52102,#39548,#39549);
#34634=AXIS2_PLACEMENT_3D('',#52106,#39552,#39553);
#34635=AXIS2_PLACEMENT_3D('',#52108,#39554,#39555);
#34636=AXIS2_PLACEMENT_3D('',#52112,#39558,#39559);
#34637=AXIS2_PLACEMENT_3D('',#52114,#39560,#39561);
#34638=AXIS2_PLACEMENT_3D('',#52118,#39564,#39565);
#34639=AXIS2_PLACEMENT_3D('',#52120,#39566,#39567);
#34640=AXIS2_PLACEMENT_3D('',#52124,#39570,#39571);
#34641=AXIS2_PLACEMENT_3D('',#52126,#39572,#39573);
#34642=AXIS2_PLACEMENT_3D('',#52130,#39576,#39577);
#34643=AXIS2_PLACEMENT_3D('',#52131,#39578,#39579);
#34644=AXIS2_PLACEMENT_3D('',#52133,#39581,#39582);
#34645=AXIS2_PLACEMENT_3D('',#52134,#39583,#39584);
#34646=AXIS2_PLACEMENT_3D('',#52135,#39585,#39586);
#34647=AXIS2_PLACEMENT_3D('',#52136,#39587,#39588);
#34648=AXIS2_PLACEMENT_3D('',#52149,#39590,#39591);
#34649=AXIS2_PLACEMENT_3D('',#52152,#39592,#39593);
#34650=AXIS2_PLACEMENT_3D('',#52156,#39595,#39596);
#34651=AXIS2_PLACEMENT_3D('',#52158,#39598,#39599);
#34652=AXIS2_PLACEMENT_3D('',#52164,#39603,#39604);
#34653=AXIS2_PLACEMENT_3D('',#52166,#39605,#39606);
#34654=AXIS2_PLACEMENT_3D('',#52168,#39607,#39608);
#34655=AXIS2_PLACEMENT_3D('',#52170,#39610,#39611);
#34656=AXIS2_PLACEMENT_3D('',#52176,#39615,#39616);
#34657=AXIS2_PLACEMENT_3D('',#52178,#39617,#39618);
#34658=AXIS2_PLACEMENT_3D('',#52180,#39619,#39620);
#34659=AXIS2_PLACEMENT_3D('',#52182,#39622,#39623);
#34660=AXIS2_PLACEMENT_3D('',#52188,#39627,#39628);
#34661=AXIS2_PLACEMENT_3D('',#52190,#39629,#39630);
#34662=AXIS2_PLACEMENT_3D('',#52192,#39631,#39632);
#34663=AXIS2_PLACEMENT_3D('',#52194,#39634,#39635);
#34664=AXIS2_PLACEMENT_3D('',#52197,#39638,#39639);
#34665=AXIS2_PLACEMENT_3D('',#52206,#39644,#39645);
#34666=AXIS2_PLACEMENT_3D('',#52208,#39646,#39647);
#34667=AXIS2_PLACEMENT_3D('',#52210,#39648,#39649);
#34668=AXIS2_PLACEMENT_3D('',#52215,#39651,#39652);
#34669=AXIS2_PLACEMENT_3D('',#52219,#39654,#39655);
#34670=AXIS2_PLACEMENT_3D('',#52223,#39657,#39658);
#34671=AXIS2_PLACEMENT_3D('',#52226,#39660,#39661);
#34672=AXIS2_PLACEMENT_3D('',#52227,#39662,#39663);
#34673=AXIS2_PLACEMENT_3D('',#52231,#39665,#39666);
#34674=AXIS2_PLACEMENT_3D('',#52233,#39668,#39669);
#34675=AXIS2_PLACEMENT_3D('',#52237,#39672,#39673);
#34676=AXIS2_PLACEMENT_3D('',#52239,#39674,#39675);
#34677=AXIS2_PLACEMENT_3D('',#52241,#39677,#39678);
#34678=AXIS2_PLACEMENT_3D('',#52245,#39681,#39682);
#34679=AXIS2_PLACEMENT_3D('',#52247,#39683,#39684);
#34680=AXIS2_PLACEMENT_3D('',#52249,#39686,#39687);
#34681=AXIS2_PLACEMENT_3D('',#52253,#39690,#39691);
#34682=AXIS2_PLACEMENT_3D('',#52255,#39692,#39693);
#34683=AXIS2_PLACEMENT_3D('',#52257,#39695,#39696);
#34684=AXIS2_PLACEMENT_3D('',#52259,#39698,#39699);
#34685=AXIS2_PLACEMENT_3D('',#52260,#39700,#39701);
#34686=AXIS2_PLACEMENT_3D('',#52262,#39702,#39703);
#34687=AXIS2_PLACEMENT_3D('',#52265,#39704,#39705);
#34688=AXIS2_PLACEMENT_3D('',#52267,#39706,#39707);
#34689=AXIS2_PLACEMENT_3D('',#52269,#39708,#39709);
#34690=AXIS2_PLACEMENT_3D('',#52271,#39710,#39711);
#34691=AXIS2_PLACEMENT_3D('',#52273,#39712,#39713);
#34692=AXIS2_PLACEMENT_3D('',#52275,#39714,#39715);
#34693=AXIS2_PLACEMENT_3D('',#52277,#39716,#39717);
#34694=AXIS2_PLACEMENT_3D('',#52279,#39718,#39719);
#34695=AXIS2_PLACEMENT_3D('',#52281,#39720,#39721);
#34696=AXIS2_PLACEMENT_3D('',#52283,#39722,#39723);
#34697=AXIS2_PLACEMENT_3D('',#52285,#39724,#39725);
#34698=AXIS2_PLACEMENT_3D('',#52286,#39726,#39727);
#34699=AXIS2_PLACEMENT_3D('',#52287,#39728,#39729);
#34700=AXIS2_PLACEMENT_3D('',#52289,#39731,#39732);
#34701=AXIS2_PLACEMENT_3D('',#52291,#39733,#39734);
#34702=AXIS2_PLACEMENT_3D('',#52294,#39735,#39736);
#34703=AXIS2_PLACEMENT_3D('',#52296,#39737,#39738);
#34704=AXIS2_PLACEMENT_3D('',#52298,#39739,#39740);
#34705=AXIS2_PLACEMENT_3D('',#52300,#39741,#39742);
#34706=AXIS2_PLACEMENT_3D('',#52302,#39743,#39744);
#34707=AXIS2_PLACEMENT_3D('',#52304,#39745,#39746);
#34708=AXIS2_PLACEMENT_3D('',#52306,#39747,#39748);
#34709=AXIS2_PLACEMENT_3D('',#52308,#39749,#39750);
#34710=AXIS2_PLACEMENT_3D('',#52310,#39751,#39752);
#34711=AXIS2_PLACEMENT_3D('',#52312,#39753,#39754);
#34712=AXIS2_PLACEMENT_3D('',#52314,#39755,#39756);
#34713=AXIS2_PLACEMENT_3D('',#52315,#39757,#39758);
#34714=AXIS2_PLACEMENT_3D('',#52316,#39759,#39760);
#34715=AXIS2_PLACEMENT_3D('',#52318,#39762,#39763);
#34716=AXIS2_PLACEMENT_3D('',#52324,#39767,#39768);
#34717=AXIS2_PLACEMENT_3D('',#52328,#39771,#39772);
#34718=AXIS2_PLACEMENT_3D('',#52332,#39775,#39776);
#34719=AXIS2_PLACEMENT_3D('',#52336,#39779,#39780);
#34720=AXIS2_PLACEMENT_3D('',#52340,#39783,#39784);
#34721=AXIS2_PLACEMENT_3D('',#52344,#39787,#39788);
#34722=AXIS2_PLACEMENT_3D('',#52348,#39791,#39792);
#34723=AXIS2_PLACEMENT_3D('',#52352,#39795,#39796);
#34724=AXIS2_PLACEMENT_3D('',#52356,#39799,#39800);
#34725=AXIS2_PLACEMENT_3D('',#52360,#39803,#39804);
#34726=AXIS2_PLACEMENT_3D('',#52364,#39807,#39808);
#34727=AXIS2_PLACEMENT_3D('',#52366,#39810,#39811);
#34728=AXIS2_PLACEMENT_3D('',#52367,#39812,#39813);
#34729=AXIS2_PLACEMENT_3D('',#52373,#39817,#39818);
#34730=AXIS2_PLACEMENT_3D('',#52377,#39821,#39822);
#34731=AXIS2_PLACEMENT_3D('',#52381,#39825,#39826);
#34732=AXIS2_PLACEMENT_3D('',#52385,#39829,#39830);
#34733=AXIS2_PLACEMENT_3D('',#52389,#39833,#39834);
#34734=AXIS2_PLACEMENT_3D('',#52393,#39837,#39838);
#34735=AXIS2_PLACEMENT_3D('',#52397,#39841,#39842);
#34736=AXIS2_PLACEMENT_3D('',#52401,#39845,#39846);
#34737=AXIS2_PLACEMENT_3D('',#52405,#39849,#39850);
#34738=AXIS2_PLACEMENT_3D('',#52409,#39853,#39854);
#34739=AXIS2_PLACEMENT_3D('',#52413,#39857,#39858);
#34740=AXIS2_PLACEMENT_3D('',#52415,#39860,#39861);
#34741=AXIS2_PLACEMENT_3D('',#52416,#39862,#39863);
#34742=AXIS2_PLACEMENT_3D('',#52434,#39873,#39874);
#34743=AXIS2_PLACEMENT_3D('',#52436,#39876,#39877);
#34744=AXIS2_PLACEMENT_3D('',#52438,#39879,#39880);
#34745=AXIS2_PLACEMENT_3D('',#52440,#39882,#39883);
#34746=AXIS2_PLACEMENT_3D('',#52442,#39885,#39886);
#34747=AXIS2_PLACEMENT_3D('',#52444,#39888,#39889);
#34748=AXIS2_PLACEMENT_3D('',#52446,#39891,#39892);
#34749=AXIS2_PLACEMENT_3D('',#52448,#39894,#39895);
#34750=AXIS2_PLACEMENT_3D('',#52450,#39897,#39898);
#34751=AXIS2_PLACEMENT_3D('',#52451,#39899,#39900);
#34752=AXIS2_PLACEMENT_3D('',#52466,#39903,#39904);
#34753=AXIS2_PLACEMENT_3D('',#52470,#39907,#39908);
#34754=AXIS2_PLACEMENT_3D('',#52471,#39909,#39910);
#34755=AXIS2_PLACEMENT_3D('',#52472,#39911,#39912);
#34756=AXIS2_PLACEMENT_3D('',#52473,#39913,#39914);
#34757=AXIS2_PLACEMENT_3D('',#52474,#39915,#39916);
#34758=AXIS2_PLACEMENT_3D('',#52489,#39919,#39920);
#34759=AXIS2_PLACEMENT_3D('',#52492,#39923,#39924);
#34760=AXIS2_PLACEMENT_3D('',#52493,#39925,#39926);
#34761=AXIS2_PLACEMENT_3D('',#52494,#39927,#39928);
#34762=AXIS2_PLACEMENT_3D('',#52497,#39931,#39932);
#34763=AXIS2_PLACEMENT_3D('',#52498,#39933,#39934);
#34764=AXIS2_PLACEMENT_3D('',#52499,#39935,#39936);
#34765=AXIS2_PLACEMENT_3D('',#52501,#39937,#39938);
#34766=AXIS2_PLACEMENT_3D('',#52503,#39940,#39941);
#34767=AXIS2_PLACEMENT_3D('',#52505,#39943,#39944);
#34768=AXIS2_PLACEMENT_3D('',#52507,#39945,#39946);
#34769=AXIS2_PLACEMENT_3D('',#52508,#39947,#39948);
#34770=AXIS2_PLACEMENT_3D('',#52509,#39949,#39950);
#34771=AXIS2_PLACEMENT_3D('',#52515,#39954,#39955);
#34772=AXIS2_PLACEMENT_3D('',#52519,#39958,#39959);
#34773=AXIS2_PLACEMENT_3D('',#52523,#39962,#39963);
#34774=AXIS2_PLACEMENT_3D('',#52527,#39966,#39967);
#34775=AXIS2_PLACEMENT_3D('',#52531,#39970,#39971);
#34776=AXIS2_PLACEMENT_3D('',#52535,#39974,#39975);
#34777=AXIS2_PLACEMENT_3D('',#52539,#39978,#39979);
#34778=AXIS2_PLACEMENT_3D('',#52543,#39982,#39983);
#34779=AXIS2_PLACEMENT_3D('',#52547,#39986,#39987);
#34780=AXIS2_PLACEMENT_3D('',#52551,#39990,#39991);
#34781=AXIS2_PLACEMENT_3D('',#52555,#39994,#39995);
#34782=AXIS2_PLACEMENT_3D('',#52558,#39997,#39998);
#34783=AXIS2_PLACEMENT_3D('',#52559,#39999,#40000);
#34784=AXIS2_PLACEMENT_3D('',#52560,#40001,#40002);
#34785=AXIS2_PLACEMENT_3D('',#52562,#40004,#40005);
#34786=AXIS2_PLACEMENT_3D('',#52563,#40006,#40007);
#34787=AXIS2_PLACEMENT_3D('',#52565,#40008,#40009);
#34788=AXIS2_PLACEMENT_3D('',#52567,#40010,#40011);
#34789=AXIS2_PLACEMENT_3D('',#52569,#40012,#40013);
#34790=AXIS2_PLACEMENT_3D('',#52571,#40014,#40015);
#34791=AXIS2_PLACEMENT_3D('',#52573,#40016,#40017);
#34792=AXIS2_PLACEMENT_3D('',#52575,#40018,#40019);
#34793=AXIS2_PLACEMENT_3D('',#52577,#40020,#40021);
#34794=AXIS2_PLACEMENT_3D('',#52579,#40022,#40023);
#34795=AXIS2_PLACEMENT_3D('',#52581,#40024,#40025);
#34796=AXIS2_PLACEMENT_3D('',#52582,#40026,#40027);
#34797=AXIS2_PLACEMENT_3D('',#52583,#40028,#40029);
#34798=AXIS2_PLACEMENT_3D('',#52603,#40040,#40041);
#34799=AXIS2_PLACEMENT_3D('',#52605,#40043,#40044);
#34800=AXIS2_PLACEMENT_3D('',#52607,#40046,#40047);
#34801=AXIS2_PLACEMENT_3D('',#52609,#40049,#40050);
#34802=AXIS2_PLACEMENT_3D('',#52611,#40052,#40053);
#34803=AXIS2_PLACEMENT_3D('',#52613,#40055,#40056);
#34804=AXIS2_PLACEMENT_3D('',#52615,#40058,#40059);
#34805=AXIS2_PLACEMENT_3D('',#52617,#40061,#40062);
#34806=AXIS2_PLACEMENT_3D('',#52619,#40064,#40065);
#34807=AXIS2_PLACEMENT_3D('',#52621,#40067,#40068);
#34808=AXIS2_PLACEMENT_3D('',#52622,#40069,#40070);
#34809=AXIS2_PLACEMENT_3D('',#52624,#40071,#40072);
#34810=AXIS2_PLACEMENT_3D('',#52626,#40073,#40074);
#34811=AXIS2_PLACEMENT_3D('',#52627,#40075,#40076);
#34812=AXIS2_PLACEMENT_3D('',#52651,#40078,#40079);
#34813=AXIS2_PLACEMENT_3D('',#52652,#40080,#40081);
#34814=AXIS2_PLACEMENT_3D('',#52671,#40082,#40083);
#34815=AXIS2_PLACEMENT_3D('',#52674,#40084,#40085);
#34816=AXIS2_PLACEMENT_3D('',#52675,#40086,#40087);
#34817=AXIS2_PLACEMENT_3D('',#52676,#40088,#40089);
#34818=AXIS2_PLACEMENT_3D('',#52700,#40091,#40092);
#34819=AXIS2_PLACEMENT_3D('',#52701,#40093,#40094);
#34820=AXIS2_PLACEMENT_3D('',#52720,#40095,#40096);
#34821=AXIS2_PLACEMENT_3D('',#52723,#40097,#40098);
#34822=AXIS2_PLACEMENT_3D('',#52730,#40099,#40100);
#34823=AXIS2_PLACEMENT_3D('',#52731,#40101,#40102);
#34824=AXIS2_PLACEMENT_3D('',#52754,#40104,#40105);
#34825=AXIS2_PLACEMENT_3D('',#52800,#40106,#40107);
#34826=AXIS2_PLACEMENT_3D('',#52801,#40108,#40109);
#34827=AXIS2_PLACEMENT_3D('',#52804,#40110,#40111);
#34828=AXIS2_PLACEMENT_3D('',#52805,#40112,#40113);
#34829=AXIS2_PLACEMENT_3D('',#52833,#40114,#40115);
#34830=AXIS2_PLACEMENT_3D('',#52861,#40116,#40117);
#34831=AXIS2_PLACEMENT_3D('',#52862,#40118,#40119);
#34832=AXIS2_PLACEMENT_3D('',#52865,#40120,#40121);
#34833=AXIS2_PLACEMENT_3D('',#52866,#40122,#40123);
#34834=AXIS2_PLACEMENT_3D('',#52868,#40124,#40125);
#34835=AXIS2_PLACEMENT_3D('',#52869,#40126,#40127);
#34836=AXIS2_PLACEMENT_3D('',#52870,#40128,#40129);
#34837=AXIS2_PLACEMENT_3D('',#52872,#40131,#40132);
#34838=AXIS2_PLACEMENT_3D('',#52873,#40133,#40134);
#34839=AXIS2_PLACEMENT_3D('',#52875,#40135,#40136);
#34840=AXIS2_PLACEMENT_3D('',#52876,#40137,#40138);
#34841=AXIS2_PLACEMENT_3D('',#52880,#40140,#40141);
#34842=AXIS2_PLACEMENT_3D('',#52881,#40142,#40143);
#34843=AXIS2_PLACEMENT_3D('',#52882,#40144,#40145);
#34844=AXIS2_PLACEMENT_3D('',#52885,#40146,#40147);
#34845=AXIS2_PLACEMENT_3D('',#52891,#40151,#40152);
#34846=AXIS2_PLACEMENT_3D('',#52921,#40168,#40169);
#34847=AXIS2_PLACEMENT_3D('',#52923,#40170,#40171);
#34848=AXIS2_PLACEMENT_3D('',#52925,#40173,#40174);
#34849=AXIS2_PLACEMENT_3D('',#52938,#40181,#40182);
#34850=AXIS2_PLACEMENT_3D('',#52951,#40189,#40190);
#34851=AXIS2_PLACEMENT_3D('',#52956,#40192,#40193);
#34852=AXIS2_PLACEMENT_3D('',#52959,#40195,#40196);
#34853=AXIS2_PLACEMENT_3D('',#52962,#40197,#40198);
#34854=AXIS2_PLACEMENT_3D('',#52966,#40200,#40201);
#34855=AXIS2_PLACEMENT_3D('',#52968,#40203,#40204);
#34856=AXIS2_PLACEMENT_3D('',#52971,#40205,#40206);
#34857=AXIS2_PLACEMENT_3D('',#52974,#40209,#40210);
#34858=AXIS2_PLACEMENT_3D('',#52978,#40213,#40214);
#34859=AXIS2_PLACEMENT_3D('',#52980,#40215,#40216);
#34860=AXIS2_PLACEMENT_3D('',#52982,#40218,#40219);
#34861=AXIS2_PLACEMENT_3D('',#52984,#40221,#40222);
#34862=AXIS2_PLACEMENT_3D('',#52989,#40224,#40225);
#34863=AXIS2_PLACEMENT_3D('',#52992,#40227,#40228);
#34864=AXIS2_PLACEMENT_3D('',#52993,#40229,#40230);
#34865=AXIS2_PLACEMENT_3D('',#52994,#40231,#40232);
#34866=AXIS2_PLACEMENT_3D('',#52995,#40233,#40234);
#34867=AXIS2_PLACEMENT_3D('',#52998,#40235,#40236);
#34868=AXIS2_PLACEMENT_3D('',#53001,#40239,#40240);
#34869=AXIS2_PLACEMENT_3D('',#53005,#40243,#40244);
#34870=AXIS2_PLACEMENT_3D('',#53007,#40245,#40246);
#34871=AXIS2_PLACEMENT_3D('',#53009,#40248,#40249);
#34872=AXIS2_PLACEMENT_3D('',#53011,#40251,#40252);
#34873=AXIS2_PLACEMENT_3D('',#53013,#40253,#40254);
#34874=AXIS2_PLACEMENT_3D('',#53014,#40255,#40256);
#34875=AXIS2_PLACEMENT_3D('',#53018,#40258,#40259);
#34876=AXIS2_PLACEMENT_3D('',#53019,#40260,#40261);
#34877=AXIS2_PLACEMENT_3D('',#53020,#40262,#40263);
#34878=AXIS2_PLACEMENT_3D('',#53023,#40265,#40266);
#34879=AXIS2_PLACEMENT_3D('',#53024,#40267,#40268);
#34880=AXIS2_PLACEMENT_3D('',#53026,#40269,#40270);
#34881=AXIS2_PLACEMENT_3D('',#53027,#40271,#40272);
#34882=AXIS2_PLACEMENT_3D('',#53031,#40274,#40275);
#34883=AXIS2_PLACEMENT_3D('',#53032,#40276,#40277);
#34884=AXIS2_PLACEMENT_3D('',#53033,#40278,#40279);
#34885=AXIS2_PLACEMENT_3D('',#53036,#40281,#40282);
#34886=AXIS2_PLACEMENT_3D('',#53037,#40283,#40284);
#34887=AXIS2_PLACEMENT_3D('',#53039,#40285,#40286);
#34888=AXIS2_PLACEMENT_3D('',#53040,#40287,#40288);
#34889=AXIS2_PLACEMENT_3D('',#53044,#40290,#40291);
#34890=AXIS2_PLACEMENT_3D('',#53045,#40292,#40293);
#34891=AXIS2_PLACEMENT_3D('',#53046,#40294,#40295);
#34892=AXIS2_PLACEMENT_3D('',#53049,#40297,#40298);
#34893=AXIS2_PLACEMENT_3D('',#53050,#40299,#40300);
#34894=AXIS2_PLACEMENT_3D('',#53052,#40301,#40302);
#34895=AXIS2_PLACEMENT_3D('',#53053,#40303,#40304);
#34896=AXIS2_PLACEMENT_3D('',#53057,#40306,#40307);
#34897=AXIS2_PLACEMENT_3D('',#53058,#40308,#40309);
#34898=AXIS2_PLACEMENT_3D('',#53059,#40310,#40311);
#34899=AXIS2_PLACEMENT_3D('',#53062,#40313,#40314);
#34900=AXIS2_PLACEMENT_3D('',#53063,#40315,#40316);
#34901=AXIS2_PLACEMENT_3D('',#53066,#40318,#40319);
#34902=AXIS2_PLACEMENT_3D('',#53067,#40320,#40321);
#34903=AXIS2_PLACEMENT_3D('',#53069,#40322,#40323);
#34904=AXIS2_PLACEMENT_3D('',#53071,#40324,#40325);
#34905=AXIS2_PLACEMENT_3D('',#53073,#40326,#40327);
#34906=AXIS2_PLACEMENT_3D('',#53075,#40328,#40329);
#34907=AXIS2_PLACEMENT_3D('',#53077,#40330,#40331);
#34908=AXIS2_PLACEMENT_3D('',#53078,#40332,#40333);
#34909=AXIS2_PLACEMENT_3D('',#53081,#40335,#40336);
#34910=AXIS2_PLACEMENT_3D('',#53082,#40337,#40338);
#34911=AXIS2_PLACEMENT_3D('',#53084,#40339,#40340);
#34912=AXIS2_PLACEMENT_3D('',#53085,#40341,#40342);
#34913=AXIS2_PLACEMENT_3D('',#53088,#40344,#40345);
#34914=AXIS2_PLACEMENT_3D('',#53089,#40346,#40347);
#34915=AXIS2_PLACEMENT_3D('',#53091,#40348,#40349);
#34916=AXIS2_PLACEMENT_3D('',#53092,#40350,#40351);
#34917=AXIS2_PLACEMENT_3D('',#53095,#40353,#40354);
#34918=AXIS2_PLACEMENT_3D('',#53096,#40355,#40356);
#34919=AXIS2_PLACEMENT_3D('',#53098,#40357,#40358);
#34920=AXIS2_PLACEMENT_3D('',#53099,#40359,#40360);
#34921=AXIS2_PLACEMENT_3D('',#53101,#40362,#40363);
#34922=AXIS2_PLACEMENT_3D('',#53103,#40364,#40365);
#34923=AXIS2_PLACEMENT_3D('',#53105,#40366,#40367);
#34924=AXIS2_PLACEMENT_3D('',#53106,#40368,#40369);
#34925=AXIS2_PLACEMENT_3D('',#53108,#40371,#40372);
#34926=AXIS2_PLACEMENT_3D('',#53111,#40374,#40375);
#34927=AXIS2_PLACEMENT_3D('',#53112,#40376,#40377);
#34928=AXIS2_PLACEMENT_3D('',#53113,#40378,#40379);
#34929=AXIS2_PLACEMENT_3D('',#53115,#40380,#40381);
#34930=AXIS2_PLACEMENT_3D('',#53117,#40383,#40384);
#34931=AXIS2_PLACEMENT_3D('',#53119,#40385,#40386);
#34932=AXIS2_PLACEMENT_3D('',#53120,#40387,#40388);
#34933=AXIS2_PLACEMENT_3D('',#53122,#40389,#40390);
#34934=AXIS2_PLACEMENT_3D('',#53124,#40392,#40393);
#34935=AXIS2_PLACEMENT_3D('',#53125,#40394,#40395);
#34936=AXIS2_PLACEMENT_3D('',#53127,#40396,#40397);
#34937=AXIS2_PLACEMENT_3D('',#53128,#40398,#40399);
#34938=AXIS2_PLACEMENT_3D('',#53130,#40400,#40401);
#34939=AXIS2_PLACEMENT_3D('',#53132,#40403,#40404);
#34940=AXIS2_PLACEMENT_3D('',#53134,#40405,#40406);
#34941=AXIS2_PLACEMENT_3D('',#53135,#40407,#40408);
#34942=AXIS2_PLACEMENT_3D('',#53137,#40410,#40411);
#34943=AXIS2_PLACEMENT_3D('',#53139,#40412,#40413);
#34944=AXIS2_PLACEMENT_3D('',#53141,#40415,#40416);
#34945=AXIS2_PLACEMENT_3D('',#53143,#40417,#40418);
#34946=AXIS2_PLACEMENT_3D('',#53144,#40419,#40420);
#34947=AXIS2_PLACEMENT_3D('',#53146,#40421,#40422);
#34948=AXIS2_PLACEMENT_3D('',#53148,#40424,#40425);
#34949=AXIS2_PLACEMENT_3D('',#53149,#40426,#40427);
#34950=AXIS2_PLACEMENT_3D('',#53159,#40433,#40434);
#34951=AXIS2_PLACEMENT_3D('',#53163,#40436,#40437);
#34952=AXIS2_PLACEMENT_3D('',#53164,#40438,#40439);
#34953=AXIS2_PLACEMENT_3D('',#53165,#40440,#40441);
#34954=AXIS2_PLACEMENT_3D('',#53172,#40446,#40447);
#34955=AXIS2_PLACEMENT_3D('',#53173,#40448,#40449);
#34956=AXIS2_PLACEMENT_3D('',#53174,#40450,#40451);
#34957=AXIS2_PLACEMENT_3D('',#53176,#40452,#40453);
#34958=AXIS2_PLACEMENT_3D('',#53177,#40454,#40455);
#34959=AXIS2_PLACEMENT_3D('',#53178,#40456,#40457);
#34960=AXIS2_PLACEMENT_3D('',#53179,#40458,#40459);
#34961=AXIS2_PLACEMENT_3D('',#53180,#40460,#40461);
#34962=AXIS2_PLACEMENT_3D('',#53181,#40462,#40463);
#34963=AXIS2_PLACEMENT_3D('',#53182,#40464,#40465);
#34964=AXIS2_PLACEMENT_3D('',#53184,#40466,#40467);
#34965=AXIS2_PLACEMENT_3D('',#53185,#40468,#40469);
#34966=AXIS2_PLACEMENT_3D('',#53186,#40470,#40471);
#34967=AXIS2_PLACEMENT_3D('',#53187,#40472,#40473);
#34968=AXIS2_PLACEMENT_3D('',#53188,#40474,#40475);
#34969=AXIS2_PLACEMENT_3D('',#53191,#40477,#40478);
#34970=AXIS2_PLACEMENT_3D('',#53192,#40479,#40480);
#34971=AXIS2_PLACEMENT_3D('',#53193,#40481,#40482);
#34972=AXIS2_PLACEMENT_3D('',#53196,#40483,#40484);
#34973=AXIS2_PLACEMENT_3D('',#53198,#40485,#40486);
#34974=AXIS2_PLACEMENT_3D('',#53200,#40487,#40488);
#34975=AXIS2_PLACEMENT_3D('',#53202,#40489,#40490);
#34976=AXIS2_PLACEMENT_3D('',#53204,#40491,#40492);
#34977=AXIS2_PLACEMENT_3D('',#53206,#40493,#40494);
#34978=AXIS2_PLACEMENT_3D('',#53208,#40495,#40496);
#34979=AXIS2_PLACEMENT_3D('',#53210,#40497,#40498);
#34980=AXIS2_PLACEMENT_3D('',#53211,#40499,#40500);
#34981=AXIS2_PLACEMENT_3D('',#53213,#40501,#40502);
#34982=AXIS2_PLACEMENT_3D('',#53215,#40503,#40504);
#34983=AXIS2_PLACEMENT_3D('',#53217,#40505,#40506);
#34984=AXIS2_PLACEMENT_3D('',#53219,#40507,#40508);
#34985=AXIS2_PLACEMENT_3D('',#53220,#40509,#40510);
#34986=AXIS2_PLACEMENT_3D('',#53221,#40511,#40512);
#34987=AXIS2_PLACEMENT_3D('',#53222,#40513,#40514);
#34988=AXIS2_PLACEMENT_3D('',#53224,#40515,#40516);
#34989=AXIS2_PLACEMENT_3D('',#53225,#40517,#40518);
#34990=AXIS2_PLACEMENT_3D('',#53227,#40520,#40521);
#34991=AXIS2_PLACEMENT_3D('',#53228,#40522,#40523);
#34992=AXIS2_PLACEMENT_3D('',#53229,#40524,#40525);
#34993=AXIS2_PLACEMENT_3D('',#53232,#40526,#40527);
#34994=AXIS2_PLACEMENT_3D('',#53234,#40528,#40529);
#34995=AXIS2_PLACEMENT_3D('',#53236,#40530,#40531);
#34996=AXIS2_PLACEMENT_3D('',#53238,#40532,#40533);
#34997=AXIS2_PLACEMENT_3D('',#53240,#40534,#40535);
#34998=AXIS2_PLACEMENT_3D('',#53242,#40536,#40537);
#34999=AXIS2_PLACEMENT_3D('',#53244,#40538,#40539);
#35000=AXIS2_PLACEMENT_3D('',#53246,#40540,#40541);
#35001=AXIS2_PLACEMENT_3D('',#53248,#40542,#40543);
#35002=AXIS2_PLACEMENT_3D('',#53250,#40544,#40545);
#35003=AXIS2_PLACEMENT_3D('',#53252,#40546,#40547);
#35004=AXIS2_PLACEMENT_3D('',#53254,#40548,#40549);
#35005=AXIS2_PLACEMENT_3D('',#53256,#40550,#40551);
#35006=AXIS2_PLACEMENT_3D('',#53258,#40552,#40553);
#35007=AXIS2_PLACEMENT_3D('',#53260,#40554,#40555);
#35008=AXIS2_PLACEMENT_3D('',#53261,#40556,#40557);
#35009=AXIS2_PLACEMENT_3D('',#53262,#40558,#40559);
#35010=AXIS2_PLACEMENT_3D('',#53268,#40563,#40564);
#35011=AXIS2_PLACEMENT_3D('',#53272,#40567,#40568);
#35012=AXIS2_PLACEMENT_3D('',#53276,#40571,#40572);
#35013=AXIS2_PLACEMENT_3D('',#53280,#40575,#40576);
#35014=AXIS2_PLACEMENT_3D('',#53284,#40579,#40580);
#35015=AXIS2_PLACEMENT_3D('',#53288,#40583,#40584);
#35016=AXIS2_PLACEMENT_3D('',#53292,#40587,#40588);
#35017=AXIS2_PLACEMENT_3D('',#53296,#40591,#40592);
#35018=AXIS2_PLACEMENT_3D('',#53300,#40595,#40596);
#35019=AXIS2_PLACEMENT_3D('',#53304,#40599,#40600);
#35020=AXIS2_PLACEMENT_3D('',#53308,#40603,#40604);
#35021=AXIS2_PLACEMENT_3D('',#53312,#40607,#40608);
#35022=AXIS2_PLACEMENT_3D('',#53316,#40611,#40612);
#35023=AXIS2_PLACEMENT_3D('',#53320,#40615,#40616);
#35024=AXIS2_PLACEMENT_3D('',#53324,#40619,#40620);
#35025=AXIS2_PLACEMENT_3D('',#53326,#40622,#40623);
#35026=AXIS2_PLACEMENT_3D('',#53327,#40624,#40625);
#35027=AXIS2_PLACEMENT_3D('',#53329,#40627,#40628);
#35028=AXIS2_PLACEMENT_3D('',#53331,#40630,#40631);
#35029=AXIS2_PLACEMENT_3D('',#53333,#40633,#40634);
#35030=AXIS2_PLACEMENT_3D('',#53335,#40636,#40637);
#35031=AXIS2_PLACEMENT_3D('',#53337,#40639,#40640);
#35032=AXIS2_PLACEMENT_3D('',#53339,#40642,#40643);
#35033=AXIS2_PLACEMENT_3D('',#53341,#40645,#40646);
#35034=AXIS2_PLACEMENT_3D('',#53343,#40648,#40649);
#35035=AXIS2_PLACEMENT_3D('',#53345,#40651,#40652);
#35036=AXIS2_PLACEMENT_3D('',#53347,#40654,#40655);
#35037=AXIS2_PLACEMENT_3D('',#53349,#40657,#40658);
#35038=AXIS2_PLACEMENT_3D('',#53351,#40660,#40661);
#35039=AXIS2_PLACEMENT_3D('',#53353,#40663,#40664);
#35040=AXIS2_PLACEMENT_3D('',#53354,#40665,#40666);
#35041=AXIS2_PLACEMENT_3D('',#53355,#40667,#40668);
#35042=AXIS2_PLACEMENT_3D('',#53358,#40669,#40670);
#35043=AXIS2_PLACEMENT_3D('',#53362,#40672,#40673);
#35044=AXIS2_PLACEMENT_3D('',#53364,#40675,#40676);
#35045=AXIS2_PLACEMENT_3D('',#53387,#40688,#40689);
#35046=AXIS2_PLACEMENT_3D('',#53389,#40690,#40691);
#35047=AXIS2_PLACEMENT_3D('',#53399,#40696,#40697);
#35048=AXIS2_PLACEMENT_3D('',#53401,#40698,#40699);
#35049=AXIS2_PLACEMENT_3D('',#53402,#40700,#40701);
#35050=AXIS2_PLACEMENT_3D('',#53404,#40702,#40703);
#35051=AXIS2_PLACEMENT_3D('',#53407,#40705,#40706);
#35052=AXIS2_PLACEMENT_3D('',#53408,#40707,#40708);
#35053=AXIS2_PLACEMENT_3D('',#53426,#40717,#40718);
#35054=AXIS2_PLACEMENT_3D('',#53434,#40723,#40724);
#35055=AXIS2_PLACEMENT_3D('',#53436,#40725,#40726);
#35056=AXIS2_PLACEMENT_3D('',#53438,#40727,#40728);
#35057=AXIS2_PLACEMENT_3D('',#53440,#40729,#40730);
#35058=AXIS2_PLACEMENT_3D('',#53443,#40732,#40733);
#35059=AXIS2_PLACEMENT_3D('',#53471,#40734,#40735);
#35060=AXIS2_PLACEMENT_3D('',#53499,#40736,#40737);
#35061=AXIS2_PLACEMENT_3D('',#53500,#40738,#40739);
#35062=AXIS2_PLACEMENT_3D('',#53506,#40743,#40744);
#35063=AXIS2_PLACEMENT_3D('',#53509,#40746,#40747);
#35064=AXIS2_PLACEMENT_3D('',#53511,#40749,#40750);
#35065=AXIS2_PLACEMENT_3D('',#53519,#40755,#40756);
#35066=AXIS2_PLACEMENT_3D('',#53521,#40757,#40758);
#35067=AXIS2_PLACEMENT_3D('',#53523,#40759,#40760);
#35068=AXIS2_PLACEMENT_3D('',#53525,#40762,#40763);
#35069=AXIS2_PLACEMENT_3D('',#53527,#40764,#40765);
#35070=AXIS2_PLACEMENT_3D('',#53529,#40766,#40767);
#35071=AXIS2_PLACEMENT_3D('',#53530,#40768,#40769);
#35072=AXIS2_PLACEMENT_3D('',#53531,#40770,#40771);
#35073=AXIS2_PLACEMENT_3D('',#53533,#40772,#40773);
#35074=AXIS2_PLACEMENT_3D('',#53534,#40774,#40775);
#35075=AXIS2_PLACEMENT_3D('',#53535,#40776,#40777);
#35076=AXIS2_PLACEMENT_3D('',#53536,#40778,#40779);
#35077=AXIS2_PLACEMENT_3D('',#53539,#40780,#40781);
#35078=AXIS2_PLACEMENT_3D('',#53541,#40782,#40783);
#35079=AXIS2_PLACEMENT_3D('',#53542,#40784,#40785);
#35080=AXIS2_PLACEMENT_3D('',#53543,#40786,#40787);
#35081=AXIS2_PLACEMENT_3D('',#53546,#40788,#40789);
#35082=AXIS2_PLACEMENT_3D('',#53547,#40790,#40791);
#35083=AXIS2_PLACEMENT_3D('',#53548,#40792,#40793);
#35084=AXIS2_PLACEMENT_3D('',#53549,#40794,#40795);
#35085=AXIS2_PLACEMENT_3D('',#53552,#40796,#40797);
#35086=AXIS2_PLACEMENT_3D('',#53554,#40798,#40799);
#35087=AXIS2_PLACEMENT_3D('',#53555,#40800,#40801);
#35088=AXIS2_PLACEMENT_3D('',#53556,#40802,#40803);
#35089=AXIS2_PLACEMENT_3D('',#53559,#40804,#40805);
#35090=AXIS2_PLACEMENT_3D('',#53560,#40806,#40807);
#35091=AXIS2_PLACEMENT_3D('',#53561,#40808,#40809);
#35092=AXIS2_PLACEMENT_3D('',#53562,#40810,#40811);
#35093=AXIS2_PLACEMENT_3D('',#53565,#40812,#40813);
#35094=AXIS2_PLACEMENT_3D('',#53567,#40814,#40815);
#35095=AXIS2_PLACEMENT_3D('',#53569,#40816,#40817);
#35096=AXIS2_PLACEMENT_3D('',#53570,#40818,#40819);
#35097=AXIS2_PLACEMENT_3D('',#53571,#40820,#40821);
#35098=AXIS2_PLACEMENT_3D('',#53574,#40822,#40823);
#35099=AXIS2_PLACEMENT_3D('',#53575,#40824,#40825);
#35100=AXIS2_PLACEMENT_3D('',#53576,#40826,#40827);
#35101=AXIS2_PLACEMENT_3D('',#53577,#40828,#40829);
#35102=AXIS2_PLACEMENT_3D('',#53580,#40830,#40831);
#35103=AXIS2_PLACEMENT_3D('',#53582,#40832,#40833);
#35104=AXIS2_PLACEMENT_3D('',#53583,#40834,#40835);
#35105=AXIS2_PLACEMENT_3D('',#53584,#40836,#40837);
#35106=AXIS2_PLACEMENT_3D('',#53587,#40838,#40839);
#35107=AXIS2_PLACEMENT_3D('',#53589,#40840,#40841);
#35108=AXIS2_PLACEMENT_3D('',#53590,#40842,#40843);
#35109=AXIS2_PLACEMENT_3D('',#53591,#40844,#40845);
#35110=AXIS2_PLACEMENT_3D('',#53594,#40848,#40849);
#35111=AXIS2_PLACEMENT_3D('',#53597,#40850,#40851);
#35112=AXIS2_PLACEMENT_3D('',#53600,#40854,#40855);
#35113=AXIS2_PLACEMENT_3D('',#53602,#40856,#40857);
#35114=AXIS2_PLACEMENT_3D('',#53604,#40858,#40859);
#35115=AXIS2_PLACEMENT_3D('',#53605,#40860,#40861);
#35116=AXIS2_PLACEMENT_3D('',#53606,#40862,#40863);
#35117=AXIS2_PLACEMENT_3D('',#53608,#40865,#40866);
#35118=AXIS2_PLACEMENT_3D('',#53611,#40869,#40870);
#35119=AXIS2_PLACEMENT_3D('',#53614,#40871,#40872);
#35120=AXIS2_PLACEMENT_3D('',#53615,#40873,#40874);
#35121=AXIS2_PLACEMENT_3D('',#53616,#40875,#40876);
#35122=AXIS2_PLACEMENT_3D('',#53617,#40877,#40878);
#35123=AXIS2_PLACEMENT_3D('',#53619,#40879,#40880);
#35124=AXIS2_PLACEMENT_3D('',#53621,#40882,#40883);
#35125=AXIS2_PLACEMENT_3D('',#53623,#40885,#40886);
#35126=AXIS2_PLACEMENT_3D('',#53626,#40889,#40890);
#35127=AXIS2_PLACEMENT_3D('',#53629,#40893,#40894);
#35128=AXIS2_PLACEMENT_3D('',#53631,#40896,#40897);
#35129=AXIS2_PLACEMENT_3D('',#53634,#40900,#40901);
#35130=AXIS2_PLACEMENT_3D('',#53637,#40904,#40905);
#35131=AXIS2_PLACEMENT_3D('',#53639,#40907,#40908);
#35132=AXIS2_PLACEMENT_3D('',#53642,#40911,#40912);
#35133=AXIS2_PLACEMENT_3D('',#53645,#40915,#40916);
#35134=AXIS2_PLACEMENT_3D('',#53647,#40918,#40919);
#35135=AXIS2_PLACEMENT_3D('',#53650,#40922,#40923);
#35136=AXIS2_PLACEMENT_3D('',#53653,#40926,#40927);
#35137=AXIS2_PLACEMENT_3D('',#53654,#40928,#40929);
#35138=AXIS2_PLACEMENT_3D('',#53656,#40931,#40932);
#35139=AXIS2_PLACEMENT_3D('',#53658,#40933,#40934);
#35140=AXIS2_PLACEMENT_3D('',#53660,#40936,#40937);
#35141=AXIS2_PLACEMENT_3D('',#53667,#40942,#40943);
#35142=AXIS2_PLACEMENT_3D('',#53673,#40947,#40948);
#35143=AXIS2_PLACEMENT_3D('',#53680,#40953,#40954);
#35144=AXIS2_PLACEMENT_3D('',#53682,#40955,#40956);
#35145=AXIS2_PLACEMENT_3D('',#53684,#40957,#40958);
#35146=AXIS2_PLACEMENT_3D('',#53694,#40963,#40964);
#35147=AXIS2_PLACEMENT_3D('',#53696,#40965,#40966);
#35148=AXIS2_PLACEMENT_3D('',#53697,#40967,#40968);
#35149=AXIS2_PLACEMENT_3D('',#53698,#40969,#40970);
#35150=AXIS2_PLACEMENT_3D('',#53699,#40971,#40972);
#35151=AXIS2_PLACEMENT_3D('',#53700,#40973,#40974);
#35152=AXIS2_PLACEMENT_3D('',#53701,#40975,#40976);
#35153=AXIS2_PLACEMENT_3D('',#53703,#40977,#40978);
#35154=AXIS2_PLACEMENT_3D('',#53705,#40980,#40981);
#35155=AXIS2_PLACEMENT_3D('',#53709,#40983,#40984);
#35156=AXIS2_PLACEMENT_3D('',#53710,#40985,#40986);
#35157=AXIS2_PLACEMENT_3D('',#53711,#40987,#40988);
#35158=AXIS2_PLACEMENT_3D('',#53713,#40989,#40990);
#35159=AXIS2_PLACEMENT_3D('',#53715,#40992,#40993);
#35160=AXIS2_PLACEMENT_3D('',#53719,#40995,#40996);
#35161=AXIS2_PLACEMENT_3D('',#53720,#40997,#40998);
#35162=AXIS2_PLACEMENT_3D('',#53721,#40999,#41000);
#35163=AXIS2_PLACEMENT_3D('',#53723,#41001,#41002);
#35164=AXIS2_PLACEMENT_3D('',#53725,#41004,#41005);
#35165=AXIS2_PLACEMENT_3D('',#53729,#41007,#41008);
#35166=AXIS2_PLACEMENT_3D('',#53730,#41009,#41010);
#35167=AXIS2_PLACEMENT_3D('',#53731,#41011,#41012);
#35168=AXIS2_PLACEMENT_3D('',#53733,#41013,#41014);
#35169=AXIS2_PLACEMENT_3D('',#53735,#41016,#41017);
#35170=AXIS2_PLACEMENT_3D('',#53739,#41019,#41020);
#35171=AXIS2_PLACEMENT_3D('',#53740,#41021,#41022);
#35172=AXIS2_PLACEMENT_3D('',#53741,#41023,#41024);
#35173=AXIS2_PLACEMENT_3D('',#53743,#41026,#41027);
#35174=AXIS2_PLACEMENT_3D('',#53745,#41029,#41030);
#35175=AXIS2_PLACEMENT_3D('',#53747,#41032,#41033);
#35176=AXIS2_PLACEMENT_3D('',#53749,#41035,#41036);
#35177=AXIS2_PLACEMENT_3D('',#53751,#41038,#41039);
#35178=AXIS2_PLACEMENT_3D('',#53752,#41040,#41041);
#35179=AXIS2_PLACEMENT_3D('',#53758,#41045,#41046);
#35180=AXIS2_PLACEMENT_3D('',#53760,#41048,#41049);
#35181=AXIS2_PLACEMENT_3D('',#53762,#41051,#41052);
#35182=AXIS2_PLACEMENT_3D('',#53763,#41053,#41054);
#35183=AXIS2_PLACEMENT_3D('',#53767,#41057,#41058);
#35184=AXIS2_PLACEMENT_3D('',#53769,#41060,#41061);
#35185=AXIS2_PLACEMENT_3D('',#53770,#41062,#41063);
#35186=AXIS2_PLACEMENT_3D('',#53772,#41065,#41066);
#35187=AXIS2_PLACEMENT_3D('',#53773,#41067,#41068);
#35188=AXIS2_PLACEMENT_3D('',#53776,#41071,#41072);
#35189=AXIS2_PLACEMENT_3D('',#53778,#41074,#41075);
#35190=AXIS2_PLACEMENT_3D('',#53780,#41077,#41078);
#35191=AXIS2_PLACEMENT_3D('',#53781,#41079,#41080);
#35192=AXIS2_PLACEMENT_3D('',#53782,#41081,#41082);
#35193=AXIS2_PLACEMENT_3D('',#53791,#41087,#41088);
#35194=AXIS2_PLACEMENT_3D('',#53793,#41089,#41090);
#35195=AXIS2_PLACEMENT_3D('',#53796,#41092,#41093);
#35196=AXIS2_PLACEMENT_3D('',#53797,#41094,#41095);
#35197=AXIS2_PLACEMENT_3D('',#53803,#41099,#41100);
#35198=AXIS2_PLACEMENT_3D('',#53805,#41101,#41102);
#35199=AXIS2_PLACEMENT_3D('',#53808,#41104,#41105);
#35200=AXIS2_PLACEMENT_3D('',#53809,#41106,#41107);
#35201=AXIS2_PLACEMENT_3D('',#53818,#41112,#41113);
#35202=AXIS2_PLACEMENT_3D('',#53820,#41114,#41115);
#35203=AXIS2_PLACEMENT_3D('',#53823,#41117,#41118);
#35204=AXIS2_PLACEMENT_3D('',#53824,#41119,#41120);
#35205=AXIS2_PLACEMENT_3D('',#53830,#41124,#41125);
#35206=AXIS2_PLACEMENT_3D('',#53832,#41126,#41127);
#35207=AXIS2_PLACEMENT_3D('',#53835,#41129,#41130);
#35208=AXIS2_PLACEMENT_3D('',#53836,#41131,#41132);
#35209=AXIS2_PLACEMENT_3D('',#53842,#41136,#41137);
#35210=AXIS2_PLACEMENT_3D('',#53844,#41138,#41139);
#35211=AXIS2_PLACEMENT_3D('',#53846,#41140,#41141);
#35212=AXIS2_PLACEMENT_3D('',#53848,#41143,#41144);
#35213=AXIS2_PLACEMENT_3D('',#53854,#41148,#41149);
#35214=AXIS2_PLACEMENT_3D('',#53855,#41150,#41151);
#35215=AXIS2_PLACEMENT_3D('',#53856,#41152,#41153);
#35216=AXIS2_PLACEMENT_3D('',#53857,#41154,#41155);
#35217=AXIS2_PLACEMENT_3D('',#53863,#41159,#41160);
#35218=AXIS2_PLACEMENT_3D('',#53865,#41161,#41162);
#35219=AXIS2_PLACEMENT_3D('',#53868,#41164,#41165);
#35220=AXIS2_PLACEMENT_3D('',#53869,#41166,#41167);
#35221=AXIS2_PLACEMENT_3D('',#53875,#41171,#41172);
#35222=AXIS2_PLACEMENT_3D('',#53876,#41173,#41174);
#35223=AXIS2_PLACEMENT_3D('',#53877,#41175,#41176);
#35224=AXIS2_PLACEMENT_3D('',#53878,#41177,#41178);
#35225=AXIS2_PLACEMENT_3D('',#53879,#41179,#41180);
#35226=AXIS2_PLACEMENT_3D('',#53880,#41181,#41182);
#35227=AXIS2_PLACEMENT_3D('',#53889,#41187,#41188);
#35228=AXIS2_PLACEMENT_3D('',#53891,#41189,#41190);
#35229=AXIS2_PLACEMENT_3D('',#53894,#41192,#41193);
#35230=AXIS2_PLACEMENT_3D('',#53895,#41194,#41195);
#35231=AXIS2_PLACEMENT_3D('',#53901,#41199,#41200);
#35232=AXIS2_PLACEMENT_3D('',#53903,#41201,#41202);
#35233=AXIS2_PLACEMENT_3D('',#53906,#41204,#41205);
#35234=AXIS2_PLACEMENT_3D('',#53907,#41206,#41207);
#35235=AXIS2_PLACEMENT_3D('',#53916,#41212,#41213);
#35236=AXIS2_PLACEMENT_3D('',#53918,#41214,#41215);
#35237=AXIS2_PLACEMENT_3D('',#53921,#41217,#41218);
#35238=AXIS2_PLACEMENT_3D('',#53922,#41219,#41220);
#35239=AXIS2_PLACEMENT_3D('',#53928,#41224,#41225);
#35240=AXIS2_PLACEMENT_3D('',#53930,#41226,#41227);
#35241=AXIS2_PLACEMENT_3D('',#53933,#41229,#41230);
#35242=AXIS2_PLACEMENT_3D('',#53934,#41231,#41232);
#35243=AXIS2_PLACEMENT_3D('',#53940,#41236,#41237);
#35244=AXIS2_PLACEMENT_3D('',#53942,#41238,#41239);
#35245=AXIS2_PLACEMENT_3D('',#53944,#41240,#41241);
#35246=AXIS2_PLACEMENT_3D('',#53946,#41243,#41244);
#35247=AXIS2_PLACEMENT_3D('',#53952,#41248,#41249);
#35248=AXIS2_PLACEMENT_3D('',#53953,#41250,#41251);
#35249=AXIS2_PLACEMENT_3D('',#53954,#41252,#41253);
#35250=AXIS2_PLACEMENT_3D('',#53955,#41254,#41255);
#35251=AXIS2_PLACEMENT_3D('',#53961,#41259,#41260);
#35252=AXIS2_PLACEMENT_3D('',#53963,#41261,#41262);
#35253=AXIS2_PLACEMENT_3D('',#53966,#41264,#41265);
#35254=AXIS2_PLACEMENT_3D('',#53967,#41266,#41267);
#35255=AXIS2_PLACEMENT_3D('',#53973,#41271,#41272);
#35256=AXIS2_PLACEMENT_3D('',#53974,#41273,#41274);
#35257=AXIS2_PLACEMENT_3D('',#53975,#41275,#41276);
#35258=AXIS2_PLACEMENT_3D('',#53976,#41277,#41278);
#35259=AXIS2_PLACEMENT_3D('',#53977,#41279,#41280);
#35260=AXIS2_PLACEMENT_3D('',#53978,#41281,#41282);
#35261=AXIS2_PLACEMENT_3D('',#53987,#41287,#41288);
#35262=AXIS2_PLACEMENT_3D('',#53989,#41289,#41290);
#35263=AXIS2_PLACEMENT_3D('',#53992,#41292,#41293);
#35264=AXIS2_PLACEMENT_3D('',#53993,#41294,#41295);
#35265=AXIS2_PLACEMENT_3D('',#53999,#41299,#41300);
#35266=AXIS2_PLACEMENT_3D('',#54001,#41301,#41302);
#35267=AXIS2_PLACEMENT_3D('',#54004,#41304,#41305);
#35268=AXIS2_PLACEMENT_3D('',#54005,#41306,#41307);
#35269=AXIS2_PLACEMENT_3D('',#54014,#41312,#41313);
#35270=AXIS2_PLACEMENT_3D('',#54016,#41314,#41315);
#35271=AXIS2_PLACEMENT_3D('',#54019,#41317,#41318);
#35272=AXIS2_PLACEMENT_3D('',#54020,#41319,#41320);
#35273=AXIS2_PLACEMENT_3D('',#54026,#41324,#41325);
#35274=AXIS2_PLACEMENT_3D('',#54028,#41326,#41327);
#35275=AXIS2_PLACEMENT_3D('',#54031,#41329,#41330);
#35276=AXIS2_PLACEMENT_3D('',#54032,#41331,#41332);
#35277=AXIS2_PLACEMENT_3D('',#54038,#41336,#41337);
#35278=AXIS2_PLACEMENT_3D('',#54040,#41338,#41339);
#35279=AXIS2_PLACEMENT_3D('',#54042,#41340,#41341);
#35280=AXIS2_PLACEMENT_3D('',#54044,#41343,#41344);
#35281=AXIS2_PLACEMENT_3D('',#54050,#41348,#41349);
#35282=AXIS2_PLACEMENT_3D('',#54051,#41350,#41351);
#35283=AXIS2_PLACEMENT_3D('',#54052,#41352,#41353);
#35284=AXIS2_PLACEMENT_3D('',#54053,#41354,#41355);
#35285=AXIS2_PLACEMENT_3D('',#54059,#41359,#41360);
#35286=AXIS2_PLACEMENT_3D('',#54061,#41361,#41362);
#35287=AXIS2_PLACEMENT_3D('',#54064,#41364,#41365);
#35288=AXIS2_PLACEMENT_3D('',#54065,#41366,#41367);
#35289=AXIS2_PLACEMENT_3D('',#54071,#41371,#41372);
#35290=AXIS2_PLACEMENT_3D('',#54072,#41373,#41374);
#35291=AXIS2_PLACEMENT_3D('',#54073,#41375,#41376);
#35292=AXIS2_PLACEMENT_3D('',#54074,#41377,#41378);
#35293=AXIS2_PLACEMENT_3D('',#54075,#41379,#41380);
#35294=AXIS2_PLACEMENT_3D('',#54076,#41381,#41382);
#35295=AXIS2_PLACEMENT_3D('',#54085,#41387,#41388);
#35296=AXIS2_PLACEMENT_3D('',#54087,#41389,#41390);
#35297=AXIS2_PLACEMENT_3D('',#54090,#41392,#41393);
#35298=AXIS2_PLACEMENT_3D('',#54091,#41394,#41395);
#35299=AXIS2_PLACEMENT_3D('',#54097,#41399,#41400);
#35300=AXIS2_PLACEMENT_3D('',#54099,#41401,#41402);
#35301=AXIS2_PLACEMENT_3D('',#54102,#41404,#41405);
#35302=AXIS2_PLACEMENT_3D('',#54103,#41406,#41407);
#35303=AXIS2_PLACEMENT_3D('',#54112,#41412,#41413);
#35304=AXIS2_PLACEMENT_3D('',#54114,#41414,#41415);
#35305=AXIS2_PLACEMENT_3D('',#54117,#41417,#41418);
#35306=AXIS2_PLACEMENT_3D('',#54118,#41419,#41420);
#35307=AXIS2_PLACEMENT_3D('',#54124,#41424,#41425);
#35308=AXIS2_PLACEMENT_3D('',#54126,#41426,#41427);
#35309=AXIS2_PLACEMENT_3D('',#54129,#41429,#41430);
#35310=AXIS2_PLACEMENT_3D('',#54130,#41431,#41432);
#35311=AXIS2_PLACEMENT_3D('',#54136,#41436,#41437);
#35312=AXIS2_PLACEMENT_3D('',#54138,#41438,#41439);
#35313=AXIS2_PLACEMENT_3D('',#54140,#41440,#41441);
#35314=AXIS2_PLACEMENT_3D('',#54142,#41443,#41444);
#35315=AXIS2_PLACEMENT_3D('',#54148,#41448,#41449);
#35316=AXIS2_PLACEMENT_3D('',#54149,#41450,#41451);
#35317=AXIS2_PLACEMENT_3D('',#54150,#41452,#41453);
#35318=AXIS2_PLACEMENT_3D('',#54151,#41454,#41455);
#35319=AXIS2_PLACEMENT_3D('',#54157,#41459,#41460);
#35320=AXIS2_PLACEMENT_3D('',#54159,#41461,#41462);
#35321=AXIS2_PLACEMENT_3D('',#54162,#41464,#41465);
#35322=AXIS2_PLACEMENT_3D('',#54163,#41466,#41467);
#35323=AXIS2_PLACEMENT_3D('',#54169,#41471,#41472);
#35324=AXIS2_PLACEMENT_3D('',#54170,#41473,#41474);
#35325=AXIS2_PLACEMENT_3D('',#54171,#41475,#41476);
#35326=AXIS2_PLACEMENT_3D('',#54172,#41477,#41478);
#35327=AXIS2_PLACEMENT_3D('',#54173,#41479,#41480);
#35328=AXIS2_PLACEMENT_3D('',#54174,#41481,#41482);
#35329=AXIS2_PLACEMENT_3D('',#54177,#41483,#41484);
#35330=AXIS2_PLACEMENT_3D('',#54181,#41486,#41487);
#35331=AXIS2_PLACEMENT_3D('',#54185,#41489,#41490);
#35332=AXIS2_PLACEMENT_3D('',#54189,#41492,#41493);
#35333=AXIS2_PLACEMENT_3D('',#54195,#41496,#41497);
#35334=AXIS2_PLACEMENT_3D('',#54199,#41499,#41500);
#35335=AXIS2_PLACEMENT_3D('',#54203,#41502,#41503);
#35336=AXIS2_PLACEMENT_3D('',#54206,#41505,#41506);
#35337=AXIS2_PLACEMENT_3D('',#54207,#41507,#41508);
#35338=AXIS2_PLACEMENT_3D('',#54213,#41512,#41513);
#35339=AXIS2_PLACEMENT_3D('',#54216,#41515,#41516);
#35340=AXIS2_PLACEMENT_3D('',#54217,#41517,#41518);
#35341=AXIS2_PLACEMENT_3D('',#54221,#41521,#41522);
#35342=AXIS2_PLACEMENT_3D('',#54224,#41524,#41525);
#35343=AXIS2_PLACEMENT_3D('',#54225,#41526,#41527);
#35344=AXIS2_PLACEMENT_3D('',#54229,#41529,#41530);
#35345=AXIS2_PLACEMENT_3D('',#54231,#41532,#41533);
#35346=AXIS2_PLACEMENT_3D('',#54235,#41535,#41536);
#35347=AXIS2_PLACEMENT_3D('',#54237,#41538,#41539);
#35348=AXIS2_PLACEMENT_3D('',#54241,#41542,#41543);
#35349=AXIS2_PLACEMENT_3D('',#54244,#41545,#41546);
#35350=AXIS2_PLACEMENT_3D('',#54248,#41548,#41549);
#35351=AXIS2_PLACEMENT_3D('',#54253,#41552,#41553);
#35352=AXIS2_PLACEMENT_3D('',#54256,#41555,#41556);
#35353=AXIS2_PLACEMENT_3D('',#54257,#41557,#41558);
#35354=AXIS2_PLACEMENT_3D('',#54259,#41560,#41561);
#35355=AXIS2_PLACEMENT_3D('',#54261,#41563,#41564);
#35356=AXIS2_PLACEMENT_3D('',#54263,#41566,#41567);
#35357=AXIS2_PLACEMENT_3D('',#54265,#41569,#41570);
#35358=AXIS2_PLACEMENT_3D('',#54266,#41571,#41572);
#35359=AXIS2_PLACEMENT_3D('',#54267,#41573,#41574);
#35360=AXIS2_PLACEMENT_3D('',#54269,#41576,#41577);
#35361=AXIS2_PLACEMENT_3D('',#54271,#41579,#41580);
#35362=AXIS2_PLACEMENT_3D('',#54272,#41581,#41582);
#35363=AXIS2_PLACEMENT_3D('',#54275,#41583,#41584);
#35364=AXIS2_PLACEMENT_3D('',#54279,#41586,#41587);
#35365=AXIS2_PLACEMENT_3D('',#54283,#41589,#41590);
#35366=AXIS2_PLACEMENT_3D('',#54287,#41592,#41593);
#35367=AXIS2_PLACEMENT_3D('',#54293,#41596,#41597);
#35368=AXIS2_PLACEMENT_3D('',#54297,#41599,#41600);
#35369=AXIS2_PLACEMENT_3D('',#54301,#41602,#41603);
#35370=AXIS2_PLACEMENT_3D('',#54304,#41605,#41606);
#35371=AXIS2_PLACEMENT_3D('',#54305,#41607,#41608);
#35372=AXIS2_PLACEMENT_3D('',#54311,#41612,#41613);
#35373=AXIS2_PLACEMENT_3D('',#54314,#41615,#41616);
#35374=AXIS2_PLACEMENT_3D('',#54315,#41617,#41618);
#35375=AXIS2_PLACEMENT_3D('',#54319,#41621,#41622);
#35376=AXIS2_PLACEMENT_3D('',#54322,#41624,#41625);
#35377=AXIS2_PLACEMENT_3D('',#54323,#41626,#41627);
#35378=AXIS2_PLACEMENT_3D('',#54327,#41629,#41630);
#35379=AXIS2_PLACEMENT_3D('',#54329,#41632,#41633);
#35380=AXIS2_PLACEMENT_3D('',#54333,#41636,#41637);
#35381=AXIS2_PLACEMENT_3D('',#54336,#41639,#41640);
#35382=AXIS2_PLACEMENT_3D('',#54337,#41641,#41642);
#35383=AXIS2_PLACEMENT_3D('',#54341,#41645,#41646);
#35384=AXIS2_PLACEMENT_3D('',#54343,#41647,#41648);
#35385=AXIS2_PLACEMENT_3D('',#54347,#41650,#41651);
#35386=AXIS2_PLACEMENT_3D('',#54352,#41654,#41655);
#35387=AXIS2_PLACEMENT_3D('',#54355,#41657,#41658);
#35388=AXIS2_PLACEMENT_3D('',#54356,#41659,#41660);
#35389=AXIS2_PLACEMENT_3D('',#54358,#41662,#41663);
#35390=AXIS2_PLACEMENT_3D('',#54360,#41665,#41666);
#35391=AXIS2_PLACEMENT_3D('',#54362,#41668,#41669);
#35392=AXIS2_PLACEMENT_3D('',#54364,#41671,#41672);
#35393=AXIS2_PLACEMENT_3D('',#54365,#41673,#41674);
#35394=AXIS2_PLACEMENT_3D('',#54367,#41676,#41677);
#35395=AXIS2_PLACEMENT_3D('',#54369,#41679,#41680);
#35396=AXIS2_PLACEMENT_3D('',#54370,#41681,#41682);
#35397=AXIS2_PLACEMENT_3D('',#54375,#41684,#41685);
#35398=AXIS2_PLACEMENT_3D('',#54379,#41687,#41688);
#35399=AXIS2_PLACEMENT_3D('',#54383,#41690,#41691);
#35400=AXIS2_PLACEMENT_3D('',#54386,#41693,#41694);
#35401=AXIS2_PLACEMENT_3D('',#54391,#41696,#41697);
#35402=AXIS2_PLACEMENT_3D('',#54395,#41699,#41700);
#35403=AXIS2_PLACEMENT_3D('',#54399,#41702,#41703);
#35404=AXIS2_PLACEMENT_3D('',#54402,#41705,#41706);
#35405=AXIS2_PLACEMENT_3D('',#54403,#41707,#41708);
#35406=AXIS2_PLACEMENT_3D('',#54409,#41712,#41713);
#35407=AXIS2_PLACEMENT_3D('',#54412,#41715,#41716);
#35408=AXIS2_PLACEMENT_3D('',#54413,#41717,#41718);
#35409=AXIS2_PLACEMENT_3D('',#54417,#41721,#41722);
#35410=AXIS2_PLACEMENT_3D('',#54420,#41724,#41725);
#35411=AXIS2_PLACEMENT_3D('',#54421,#41726,#41727);
#35412=AXIS2_PLACEMENT_3D('',#54427,#41731,#41732);
#35413=AXIS2_PLACEMENT_3D('',#54430,#41734,#41735);
#35414=AXIS2_PLACEMENT_3D('',#54431,#41736,#41737);
#35415=AXIS2_PLACEMENT_3D('',#54435,#41740,#41741);
#35416=AXIS2_PLACEMENT_3D('',#54438,#41743,#41744);
#35417=AXIS2_PLACEMENT_3D('',#54439,#41745,#41746);
#35418=AXIS2_PLACEMENT_3D('',#54443,#41748,#41749);
#35419=AXIS2_PLACEMENT_3D('',#54446,#41751,#41752);
#35420=AXIS2_PLACEMENT_3D('',#54450,#41754,#41755);
#35421=AXIS2_PLACEMENT_3D('',#54453,#41757,#41758);
#35422=AXIS2_PLACEMENT_3D('',#54454,#41759,#41760);
#35423=AXIS2_PLACEMENT_3D('',#54456,#41762,#41763);
#35424=AXIS2_PLACEMENT_3D('',#54458,#41765,#41766);
#35425=AXIS2_PLACEMENT_3D('',#54460,#41768,#41769);
#35426=AXIS2_PLACEMENT_3D('',#54462,#41771,#41772);
#35427=AXIS2_PLACEMENT_3D('',#54463,#41773,#41774);
#35428=AXIS2_PLACEMENT_3D('',#54465,#41776,#41777);
#35429=AXIS2_PLACEMENT_3D('',#54467,#41779,#41780);
#35430=AXIS2_PLACEMENT_3D('',#54468,#41781,#41782);
#35431=AXIS2_PLACEMENT_3D('',#54473,#41784,#41785);
#35432=AXIS2_PLACEMENT_3D('',#54477,#41787,#41788);
#35433=AXIS2_PLACEMENT_3D('',#54481,#41790,#41791);
#35434=AXIS2_PLACEMENT_3D('',#54484,#41793,#41794);
#35435=AXIS2_PLACEMENT_3D('',#54489,#41796,#41797);
#35436=AXIS2_PLACEMENT_3D('',#54493,#41799,#41800);
#35437=AXIS2_PLACEMENT_3D('',#54497,#41802,#41803);
#35438=AXIS2_PLACEMENT_3D('',#54500,#41805,#41806);
#35439=AXIS2_PLACEMENT_3D('',#54501,#41807,#41808);
#35440=AXIS2_PLACEMENT_3D('',#54507,#41812,#41813);
#35441=AXIS2_PLACEMENT_3D('',#54510,#41815,#41816);
#35442=AXIS2_PLACEMENT_3D('',#54511,#41817,#41818);
#35443=AXIS2_PLACEMENT_3D('',#54515,#41821,#41822);
#35444=AXIS2_PLACEMENT_3D('',#54518,#41824,#41825);
#35445=AXIS2_PLACEMENT_3D('',#54519,#41826,#41827);
#35446=AXIS2_PLACEMENT_3D('',#54525,#41831,#41832);
#35447=AXIS2_PLACEMENT_3D('',#54528,#41834,#41835);
#35448=AXIS2_PLACEMENT_3D('',#54529,#41836,#41837);
#35449=AXIS2_PLACEMENT_3D('',#54533,#41840,#41841);
#35450=AXIS2_PLACEMENT_3D('',#54536,#41843,#41844);
#35451=AXIS2_PLACEMENT_3D('',#54537,#41845,#41846);
#35452=AXIS2_PLACEMENT_3D('',#54541,#41848,#41849);
#35453=AXIS2_PLACEMENT_3D('',#54544,#41851,#41852);
#35454=AXIS2_PLACEMENT_3D('',#54548,#41854,#41855);
#35455=AXIS2_PLACEMENT_3D('',#54551,#41857,#41858);
#35456=AXIS2_PLACEMENT_3D('',#54552,#41859,#41860);
#35457=AXIS2_PLACEMENT_3D('',#54554,#41862,#41863);
#35458=AXIS2_PLACEMENT_3D('',#54556,#41865,#41866);
#35459=AXIS2_PLACEMENT_3D('',#54558,#41868,#41869);
#35460=AXIS2_PLACEMENT_3D('',#54560,#41871,#41872);
#35461=AXIS2_PLACEMENT_3D('',#54561,#41873,#41874);
#35462=AXIS2_PLACEMENT_3D('',#54563,#41876,#41877);
#35463=AXIS2_PLACEMENT_3D('',#54565,#41879,#41880);
#35464=AXIS2_PLACEMENT_3D('',#54566,#41881,#41882);
#35465=AXIS2_PLACEMENT_3D('',#54575,#41887,#41888);
#35466=AXIS2_PLACEMENT_3D('',#54577,#41889,#41890);
#35467=AXIS2_PLACEMENT_3D('',#54580,#41892,#41893);
#35468=AXIS2_PLACEMENT_3D('',#54581,#41894,#41895);
#35469=AXIS2_PLACEMENT_3D('',#54587,#41899,#41900);
#35470=AXIS2_PLACEMENT_3D('',#54589,#41901,#41902);
#35471=AXIS2_PLACEMENT_3D('',#54592,#41904,#41905);
#35472=AXIS2_PLACEMENT_3D('',#54593,#41906,#41907);
#35473=AXIS2_PLACEMENT_3D('',#54602,#41912,#41913);
#35474=AXIS2_PLACEMENT_3D('',#54604,#41914,#41915);
#35475=AXIS2_PLACEMENT_3D('',#54607,#41917,#41918);
#35476=AXIS2_PLACEMENT_3D('',#54608,#41919,#41920);
#35477=AXIS2_PLACEMENT_3D('',#54614,#41924,#41925);
#35478=AXIS2_PLACEMENT_3D('',#54616,#41926,#41927);
#35479=AXIS2_PLACEMENT_3D('',#54619,#41929,#41930);
#35480=AXIS2_PLACEMENT_3D('',#54620,#41931,#41932);
#35481=AXIS2_PLACEMENT_3D('',#54626,#41936,#41937);
#35482=AXIS2_PLACEMENT_3D('',#54628,#41938,#41939);
#35483=AXIS2_PLACEMENT_3D('',#54630,#41940,#41941);
#35484=AXIS2_PLACEMENT_3D('',#54632,#41943,#41944);
#35485=AXIS2_PLACEMENT_3D('',#54638,#41948,#41949);
#35486=AXIS2_PLACEMENT_3D('',#54639,#41950,#41951);
#35487=AXIS2_PLACEMENT_3D('',#54640,#41952,#41953);
#35488=AXIS2_PLACEMENT_3D('',#54641,#41954,#41955);
#35489=AXIS2_PLACEMENT_3D('',#54647,#41959,#41960);
#35490=AXIS2_PLACEMENT_3D('',#54649,#41961,#41962);
#35491=AXIS2_PLACEMENT_3D('',#54652,#41964,#41965);
#35492=AXIS2_PLACEMENT_3D('',#54653,#41966,#41967);
#35493=AXIS2_PLACEMENT_3D('',#54659,#41971,#41972);
#35494=AXIS2_PLACEMENT_3D('',#54660,#41973,#41974);
#35495=AXIS2_PLACEMENT_3D('',#54661,#41975,#41976);
#35496=AXIS2_PLACEMENT_3D('',#54662,#41977,#41978);
#35497=AXIS2_PLACEMENT_3D('',#54663,#41979,#41980);
#35498=AXIS2_PLACEMENT_3D('',#54664,#41981,#41982);
#35499=AXIS2_PLACEMENT_3D('',#54673,#41987,#41988);
#35500=AXIS2_PLACEMENT_3D('',#54675,#41989,#41990);
#35501=AXIS2_PLACEMENT_3D('',#54678,#41992,#41993);
#35502=AXIS2_PLACEMENT_3D('',#54679,#41994,#41995);
#35503=AXIS2_PLACEMENT_3D('',#54685,#41999,#42000);
#35504=AXIS2_PLACEMENT_3D('',#54687,#42001,#42002);
#35505=AXIS2_PLACEMENT_3D('',#54690,#42004,#42005);
#35506=AXIS2_PLACEMENT_3D('',#54691,#42006,#42007);
#35507=AXIS2_PLACEMENT_3D('',#54700,#42012,#42013);
#35508=AXIS2_PLACEMENT_3D('',#54702,#42014,#42015);
#35509=AXIS2_PLACEMENT_3D('',#54705,#42017,#42018);
#35510=AXIS2_PLACEMENT_3D('',#54706,#42019,#42020);
#35511=AXIS2_PLACEMENT_3D('',#54712,#42024,#42025);
#35512=AXIS2_PLACEMENT_3D('',#54714,#42026,#42027);
#35513=AXIS2_PLACEMENT_3D('',#54717,#42029,#42030);
#35514=AXIS2_PLACEMENT_3D('',#54718,#42031,#42032);
#35515=AXIS2_PLACEMENT_3D('',#54724,#42036,#42037);
#35516=AXIS2_PLACEMENT_3D('',#54726,#42038,#42039);
#35517=AXIS2_PLACEMENT_3D('',#54728,#42040,#42041);
#35518=AXIS2_PLACEMENT_3D('',#54730,#42043,#42044);
#35519=AXIS2_PLACEMENT_3D('',#54736,#42048,#42049);
#35520=AXIS2_PLACEMENT_3D('',#54737,#42050,#42051);
#35521=AXIS2_PLACEMENT_3D('',#54738,#42052,#42053);
#35522=AXIS2_PLACEMENT_3D('',#54739,#42054,#42055);
#35523=AXIS2_PLACEMENT_3D('',#54745,#42059,#42060);
#35524=AXIS2_PLACEMENT_3D('',#54747,#42061,#42062);
#35525=AXIS2_PLACEMENT_3D('',#54750,#42064,#42065);
#35526=AXIS2_PLACEMENT_3D('',#54751,#42066,#42067);
#35527=AXIS2_PLACEMENT_3D('',#54757,#42071,#42072);
#35528=AXIS2_PLACEMENT_3D('',#54758,#42073,#42074);
#35529=AXIS2_PLACEMENT_3D('',#54759,#42075,#42076);
#35530=AXIS2_PLACEMENT_3D('',#54760,#42077,#42078);
#35531=AXIS2_PLACEMENT_3D('',#54761,#42079,#42080);
#35532=AXIS2_PLACEMENT_3D('',#54762,#42081,#42082);
#35533=AXIS2_PLACEMENT_3D('',#54771,#42087,#42088);
#35534=AXIS2_PLACEMENT_3D('',#54773,#42089,#42090);
#35535=AXIS2_PLACEMENT_3D('',#54776,#42092,#42093);
#35536=AXIS2_PLACEMENT_3D('',#54777,#42094,#42095);
#35537=AXIS2_PLACEMENT_3D('',#54783,#42099,#42100);
#35538=AXIS2_PLACEMENT_3D('',#54785,#42101,#42102);
#35539=AXIS2_PLACEMENT_3D('',#54788,#42104,#42105);
#35540=AXIS2_PLACEMENT_3D('',#54789,#42106,#42107);
#35541=AXIS2_PLACEMENT_3D('',#54798,#42112,#42113);
#35542=AXIS2_PLACEMENT_3D('',#54800,#42114,#42115);
#35543=AXIS2_PLACEMENT_3D('',#54803,#42117,#42118);
#35544=AXIS2_PLACEMENT_3D('',#54804,#42119,#42120);
#35545=AXIS2_PLACEMENT_3D('',#54810,#42124,#42125);
#35546=AXIS2_PLACEMENT_3D('',#54812,#42126,#42127);
#35547=AXIS2_PLACEMENT_3D('',#54815,#42129,#42130);
#35548=AXIS2_PLACEMENT_3D('',#54816,#42131,#42132);
#35549=AXIS2_PLACEMENT_3D('',#54822,#42136,#42137);
#35550=AXIS2_PLACEMENT_3D('',#54824,#42138,#42139);
#35551=AXIS2_PLACEMENT_3D('',#54826,#42140,#42141);
#35552=AXIS2_PLACEMENT_3D('',#54828,#42143,#42144);
#35553=AXIS2_PLACEMENT_3D('',#54834,#42148,#42149);
#35554=AXIS2_PLACEMENT_3D('',#54835,#42150,#42151);
#35555=AXIS2_PLACEMENT_3D('',#54836,#42152,#42153);
#35556=AXIS2_PLACEMENT_3D('',#54837,#42154,#42155);
#35557=AXIS2_PLACEMENT_3D('',#54843,#42159,#42160);
#35558=AXIS2_PLACEMENT_3D('',#54845,#42161,#42162);
#35559=AXIS2_PLACEMENT_3D('',#54848,#42164,#42165);
#35560=AXIS2_PLACEMENT_3D('',#54849,#42166,#42167);
#35561=AXIS2_PLACEMENT_3D('',#54855,#42171,#42172);
#35562=AXIS2_PLACEMENT_3D('',#54856,#42173,#42174);
#35563=AXIS2_PLACEMENT_3D('',#54857,#42175,#42176);
#35564=AXIS2_PLACEMENT_3D('',#54858,#42177,#42178);
#35565=AXIS2_PLACEMENT_3D('',#54859,#42179,#42180);
#35566=AXIS2_PLACEMENT_3D('',#54860,#42181,#42182);
#35567=AXIS2_PLACEMENT_3D('',#54863,#42183,#42184);
#35568=AXIS2_PLACEMENT_3D('',#54867,#42186,#42187);
#35569=AXIS2_PLACEMENT_3D('',#54869,#42189,#42190);
#35570=AXIS2_PLACEMENT_3D('',#54875,#42194,#42195);
#35571=AXIS2_PLACEMENT_3D('',#54877,#42196,#42197);
#35572=AXIS2_PLACEMENT_3D('',#54880,#42199,#42200);
#35573=AXIS2_PLACEMENT_3D('',#54881,#42201,#42202);
#35574=AXIS2_PLACEMENT_3D('',#54887,#42206,#42207);
#35575=AXIS2_PLACEMENT_3D('',#54889,#42208,#42209);
#35576=AXIS2_PLACEMENT_3D('',#54892,#42211,#42212);
#35577=AXIS2_PLACEMENT_3D('',#54893,#42213,#42214);
#35578=AXIS2_PLACEMENT_3D('',#54899,#42218,#42219);
#35579=AXIS2_PLACEMENT_3D('',#54901,#42220,#42221);
#35580=AXIS2_PLACEMENT_3D('',#54904,#42223,#42224);
#35581=AXIS2_PLACEMENT_3D('',#54905,#42225,#42226);
#35582=AXIS2_PLACEMENT_3D('',#54908,#42229,#42230);
#35583=AXIS2_PLACEMENT_3D('',#54911,#42231,#42232);
#35584=AXIS2_PLACEMENT_3D('',#54915,#42234,#42235);
#35585=AXIS2_PLACEMENT_3D('',#54917,#42237,#42238);
#35586=AXIS2_PLACEMENT_3D('',#54923,#42242,#42243);
#35587=AXIS2_PLACEMENT_3D('',#54925,#42244,#42245);
#35588=AXIS2_PLACEMENT_3D('',#54927,#42246,#42247);
#35589=AXIS2_PLACEMENT_3D('',#54929,#42249,#42250);
#35590=AXIS2_PLACEMENT_3D('',#54935,#42254,#42255);
#35591=AXIS2_PLACEMENT_3D('',#54937,#42256,#42257);
#35592=AXIS2_PLACEMENT_3D('',#54939,#42258,#42259);
#35593=AXIS2_PLACEMENT_3D('',#54941,#42261,#42262);
#35594=AXIS2_PLACEMENT_3D('',#54947,#42266,#42267);
#35595=AXIS2_PLACEMENT_3D('',#54949,#42268,#42269);
#35596=AXIS2_PLACEMENT_3D('',#54951,#42270,#42271);
#35597=AXIS2_PLACEMENT_3D('',#54953,#42273,#42274);
#35598=AXIS2_PLACEMENT_3D('',#54956,#42277,#42278);
#35599=AXIS2_PLACEMENT_3D('',#54957,#42279,#42280);
#35600=AXIS2_PLACEMENT_3D('',#54958,#42281,#42282);
#35601=AXIS2_PLACEMENT_3D('',#54961,#42283,#42284);
#35602=AXIS2_PLACEMENT_3D('',#54965,#42286,#42287);
#35603=AXIS2_PLACEMENT_3D('',#54967,#42289,#42290);
#35604=AXIS2_PLACEMENT_3D('',#54973,#42294,#42295);
#35605=AXIS2_PLACEMENT_3D('',#54975,#42296,#42297);
#35606=AXIS2_PLACEMENT_3D('',#54978,#42299,#42300);
#35607=AXIS2_PLACEMENT_3D('',#54979,#42301,#42302);
#35608=AXIS2_PLACEMENT_3D('',#54985,#42306,#42307);
#35609=AXIS2_PLACEMENT_3D('',#54987,#42308,#42309);
#35610=AXIS2_PLACEMENT_3D('',#54990,#42311,#42312);
#35611=AXIS2_PLACEMENT_3D('',#54991,#42313,#42314);
#35612=AXIS2_PLACEMENT_3D('',#54997,#42318,#42319);
#35613=AXIS2_PLACEMENT_3D('',#54999,#42320,#42321);
#35614=AXIS2_PLACEMENT_3D('',#55002,#42323,#42324);
#35615=AXIS2_PLACEMENT_3D('',#55003,#42325,#42326);
#35616=AXIS2_PLACEMENT_3D('',#55006,#42329,#42330);
#35617=AXIS2_PLACEMENT_3D('',#55009,#42331,#42332);
#35618=AXIS2_PLACEMENT_3D('',#55013,#42334,#42335);
#35619=AXIS2_PLACEMENT_3D('',#55015,#42337,#42338);
#35620=AXIS2_PLACEMENT_3D('',#55021,#42342,#42343);
#35621=AXIS2_PLACEMENT_3D('',#55023,#42344,#42345);
#35622=AXIS2_PLACEMENT_3D('',#55025,#42346,#42347);
#35623=AXIS2_PLACEMENT_3D('',#55027,#42349,#42350);
#35624=AXIS2_PLACEMENT_3D('',#55033,#42354,#42355);
#35625=AXIS2_PLACEMENT_3D('',#55035,#42356,#42357);
#35626=AXIS2_PLACEMENT_3D('',#55037,#42358,#42359);
#35627=AXIS2_PLACEMENT_3D('',#55039,#42361,#42362);
#35628=AXIS2_PLACEMENT_3D('',#55045,#42366,#42367);
#35629=AXIS2_PLACEMENT_3D('',#55047,#42368,#42369);
#35630=AXIS2_PLACEMENT_3D('',#55049,#42370,#42371);
#35631=AXIS2_PLACEMENT_3D('',#55051,#42373,#42374);
#35632=AXIS2_PLACEMENT_3D('',#55054,#42377,#42378);
#35633=AXIS2_PLACEMENT_3D('',#55055,#42379,#42380);
#35634=AXIS2_PLACEMENT_3D('',#55056,#42381,#42382);
#35635=AXIS2_PLACEMENT_3D('',#55059,#42383,#42384);
#35636=AXIS2_PLACEMENT_3D('',#55063,#42386,#42387);
#35637=AXIS2_PLACEMENT_3D('',#55065,#42389,#42390);
#35638=AXIS2_PLACEMENT_3D('',#55071,#42394,#42395);
#35639=AXIS2_PLACEMENT_3D('',#55073,#42396,#42397);
#35640=AXIS2_PLACEMENT_3D('',#55076,#42399,#42400);
#35641=AXIS2_PLACEMENT_3D('',#55077,#42401,#42402);
#35642=AXIS2_PLACEMENT_3D('',#55083,#42406,#42407);
#35643=AXIS2_PLACEMENT_3D('',#55085,#42408,#42409);
#35644=AXIS2_PLACEMENT_3D('',#55088,#42411,#42412);
#35645=AXIS2_PLACEMENT_3D('',#55089,#42413,#42414);
#35646=AXIS2_PLACEMENT_3D('',#55095,#42418,#42419);
#35647=AXIS2_PLACEMENT_3D('',#55097,#42420,#42421);
#35648=AXIS2_PLACEMENT_3D('',#55100,#42423,#42424);
#35649=AXIS2_PLACEMENT_3D('',#55101,#42425,#42426);
#35650=AXIS2_PLACEMENT_3D('',#55104,#42429,#42430);
#35651=AXIS2_PLACEMENT_3D('',#55107,#42431,#42432);
#35652=AXIS2_PLACEMENT_3D('',#55111,#42434,#42435);
#35653=AXIS2_PLACEMENT_3D('',#55113,#42437,#42438);
#35654=AXIS2_PLACEMENT_3D('',#55119,#42442,#42443);
#35655=AXIS2_PLACEMENT_3D('',#55121,#42444,#42445);
#35656=AXIS2_PLACEMENT_3D('',#55123,#42446,#42447);
#35657=AXIS2_PLACEMENT_3D('',#55125,#42449,#42450);
#35658=AXIS2_PLACEMENT_3D('',#55131,#42454,#42455);
#35659=AXIS2_PLACEMENT_3D('',#55133,#42456,#42457);
#35660=AXIS2_PLACEMENT_3D('',#55135,#42458,#42459);
#35661=AXIS2_PLACEMENT_3D('',#55137,#42461,#42462);
#35662=AXIS2_PLACEMENT_3D('',#55143,#42466,#42467);
#35663=AXIS2_PLACEMENT_3D('',#55145,#42468,#42469);
#35664=AXIS2_PLACEMENT_3D('',#55147,#42470,#42471);
#35665=AXIS2_PLACEMENT_3D('',#55149,#42473,#42474);
#35666=AXIS2_PLACEMENT_3D('',#55152,#42477,#42478);
#35667=AXIS2_PLACEMENT_3D('',#55153,#42479,#42480);
#35668=AXIS2_PLACEMENT_3D('',#55154,#42481,#42482);
#35669=AXIS2_PLACEMENT_3D('',#55157,#42483,#42484);
#35670=AXIS2_PLACEMENT_3D('',#55161,#42486,#42487);
#35671=AXIS2_PLACEMENT_3D('',#55163,#42489,#42490);
#35672=AXIS2_PLACEMENT_3D('',#55169,#42494,#42495);
#35673=AXIS2_PLACEMENT_3D('',#55171,#42496,#42497);
#35674=AXIS2_PLACEMENT_3D('',#55174,#42499,#42500);
#35675=AXIS2_PLACEMENT_3D('',#55175,#42501,#42502);
#35676=AXIS2_PLACEMENT_3D('',#55181,#42506,#42507);
#35677=AXIS2_PLACEMENT_3D('',#55183,#42508,#42509);
#35678=AXIS2_PLACEMENT_3D('',#55186,#42511,#42512);
#35679=AXIS2_PLACEMENT_3D('',#55187,#42513,#42514);
#35680=AXIS2_PLACEMENT_3D('',#55193,#42518,#42519);
#35681=AXIS2_PLACEMENT_3D('',#55195,#42520,#42521);
#35682=AXIS2_PLACEMENT_3D('',#55198,#42523,#42524);
#35683=AXIS2_PLACEMENT_3D('',#55199,#42525,#42526);
#35684=AXIS2_PLACEMENT_3D('',#55202,#42529,#42530);
#35685=AXIS2_PLACEMENT_3D('',#55205,#42531,#42532);
#35686=AXIS2_PLACEMENT_3D('',#55209,#42534,#42535);
#35687=AXIS2_PLACEMENT_3D('',#55211,#42537,#42538);
#35688=AXIS2_PLACEMENT_3D('',#55217,#42542,#42543);
#35689=AXIS2_PLACEMENT_3D('',#55219,#42544,#42545);
#35690=AXIS2_PLACEMENT_3D('',#55221,#42546,#42547);
#35691=AXIS2_PLACEMENT_3D('',#55223,#42549,#42550);
#35692=AXIS2_PLACEMENT_3D('',#55229,#42554,#42555);
#35693=AXIS2_PLACEMENT_3D('',#55231,#42556,#42557);
#35694=AXIS2_PLACEMENT_3D('',#55233,#42558,#42559);
#35695=AXIS2_PLACEMENT_3D('',#55235,#42561,#42562);
#35696=AXIS2_PLACEMENT_3D('',#55241,#42566,#42567);
#35697=AXIS2_PLACEMENT_3D('',#55243,#42568,#42569);
#35698=AXIS2_PLACEMENT_3D('',#55245,#42570,#42571);
#35699=AXIS2_PLACEMENT_3D('',#55247,#42573,#42574);
#35700=AXIS2_PLACEMENT_3D('',#55250,#42577,#42578);
#35701=AXIS2_PLACEMENT_3D('',#55251,#42579,#42580);
#35702=AXIS2_PLACEMENT_3D('',#55252,#42581,#42582);
#35703=AXIS2_PLACEMENT_3D('',#55253,#42583,#42584);
#35704=AXIS2_PLACEMENT_3D('',#55254,#42585,#42586);
#35705=AXIS2_PLACEMENT_3D('',#55256,#42587,#42588);
#35706=AXIS2_PLACEMENT_3D('',#55259,#42590,#42591);
#35707=AXIS2_PLACEMENT_3D('',#55260,#42592,#42593);
#35708=AXIS2_PLACEMENT_3D('',#55262,#42594,#42595);
#35709=AXIS2_PLACEMENT_3D('',#55265,#42597,#42598);
#35710=AXIS2_PLACEMENT_3D('',#55266,#42599,#42600);
#35711=AXIS2_PLACEMENT_3D('',#55268,#42601,#42602);
#35712=AXIS2_PLACEMENT_3D('',#55271,#42604,#42605);
#35713=AXIS2_PLACEMENT_3D('',#55272,#42606,#42607);
#35714=AXIS2_PLACEMENT_3D('',#55274,#42608,#42609);
#35715=AXIS2_PLACEMENT_3D('',#55277,#42611,#42612);
#35716=AXIS2_PLACEMENT_3D('',#55278,#42613,#42614);
#35717=AXIS2_PLACEMENT_3D('',#55280,#42615,#42616);
#35718=AXIS2_PLACEMENT_3D('',#55283,#42618,#42619);
#35719=AXIS2_PLACEMENT_3D('',#55284,#42620,#42621);
#35720=AXIS2_PLACEMENT_3D('',#55286,#42622,#42623);
#35721=AXIS2_PLACEMENT_3D('',#55289,#42625,#42626);
#35722=AXIS2_PLACEMENT_3D('',#55290,#42627,#42628);
#35723=AXIS2_PLACEMENT_3D('',#55292,#42629,#42630);
#35724=AXIS2_PLACEMENT_3D('',#55295,#42632,#42633);
#35725=AXIS2_PLACEMENT_3D('',#55296,#42634,#42635);
#35726=AXIS2_PLACEMENT_3D('',#55298,#42636,#42637);
#35727=AXIS2_PLACEMENT_3D('',#55301,#42639,#42640);
#35728=AXIS2_PLACEMENT_3D('',#55302,#42641,#42642);
#35729=AXIS2_PLACEMENT_3D('',#55304,#42643,#42644);
#35730=AXIS2_PLACEMENT_3D('',#55307,#42646,#42647);
#35731=AXIS2_PLACEMENT_3D('',#55308,#42648,#42649);
#35732=AXIS2_PLACEMENT_3D('',#55310,#42650,#42651);
#35733=AXIS2_PLACEMENT_3D('',#55313,#42653,#42654);
#35734=AXIS2_PLACEMENT_3D('',#55314,#42655,#42656);
#35735=AXIS2_PLACEMENT_3D('',#55316,#42657,#42658);
#35736=AXIS2_PLACEMENT_3D('',#55319,#42660,#42661);
#35737=AXIS2_PLACEMENT_3D('',#55320,#42662,#42663);
#35738=AXIS2_PLACEMENT_3D('',#55322,#42664,#42665);
#35739=AXIS2_PLACEMENT_3D('',#55325,#42667,#42668);
#35740=AXIS2_PLACEMENT_3D('',#55326,#42669,#42670);
#35741=AXIS2_PLACEMENT_3D('',#55328,#42671,#42672);
#35742=AXIS2_PLACEMENT_3D('',#55331,#42674,#42675);
#35743=AXIS2_PLACEMENT_3D('',#55332,#42676,#42677);
#35744=AXIS2_PLACEMENT_3D('',#55334,#42678,#42679);
#35745=AXIS2_PLACEMENT_3D('',#55337,#42681,#42682);
#35746=AXIS2_PLACEMENT_3D('',#55338,#42683,#42684);
#35747=AXIS2_PLACEMENT_3D('',#55340,#42685,#42686);
#35748=AXIS2_PLACEMENT_3D('',#55343,#42688,#42689);
#35749=AXIS2_PLACEMENT_3D('',#55344,#42690,#42691);
#35750=AXIS2_PLACEMENT_3D('',#55346,#42692,#42693);
#35751=AXIS2_PLACEMENT_3D('',#55349,#42695,#42696);
#35752=AXIS2_PLACEMENT_3D('',#55350,#42697,#42698);
#35753=AXIS2_PLACEMENT_3D('',#55359,#42703,#42704);
#35754=AXIS2_PLACEMENT_3D('',#55365,#42708,#42709);
#35755=AXIS2_PLACEMENT_3D('',#55371,#42713,#42714);
#35756=AXIS2_PLACEMENT_3D('',#55374,#42717,#42718);
#35757=AXIS2_PLACEMENT_3D('',#55383,#42723,#42724);
#35758=AXIS2_PLACEMENT_3D('',#55389,#42728,#42729);
#35759=AXIS2_PLACEMENT_3D('',#55393,#42732,#42733);
#35760=AXIS2_PLACEMENT_3D('',#55397,#42736,#42737);
#35761=AXIS2_PLACEMENT_3D('',#55399,#42739,#42740);
#35762=AXIS2_PLACEMENT_3D('',#55400,#42741,#42742);
#35763=AXIS2_PLACEMENT_3D('',#55401,#42743,#42744);
#35764=AXIS2_PLACEMENT_3D('',#55411,#42749,#42750);
#35765=AXIS2_PLACEMENT_3D('',#55413,#42751,#42752);
#35766=AXIS2_PLACEMENT_3D('',#55415,#42753,#42754);
#35767=AXIS2_PLACEMENT_3D('',#55416,#42755,#42756);
#35768=AXIS2_PLACEMENT_3D('',#55426,#42761,#42762);
#35769=AXIS2_PLACEMENT_3D('',#55428,#42763,#42764);
#35770=AXIS2_PLACEMENT_3D('',#55430,#42765,#42766);
#35771=AXIS2_PLACEMENT_3D('',#55431,#42767,#42768);
#35772=AXIS2_PLACEMENT_3D('',#55434,#42771,#42772);
#35773=AXIS2_PLACEMENT_3D('',#55438,#42774,#42775);
#35774=AXIS2_PLACEMENT_3D('',#55439,#42776,#42777);
#35775=AXIS2_PLACEMENT_3D('',#55441,#42779,#42780);
#35776=AXIS2_PLACEMENT_3D('',#55445,#42782,#42783);
#35777=AXIS2_PLACEMENT_3D('',#55446,#42784,#42785);
#35778=AXIS2_PLACEMENT_3D('',#55448,#42787,#42788);
#35779=AXIS2_PLACEMENT_3D('',#55452,#42790,#42791);
#35780=AXIS2_PLACEMENT_3D('',#55453,#42792,#42793);
#35781=AXIS2_PLACEMENT_3D('',#55455,#42795,#42796);
#35782=AXIS2_PLACEMENT_3D('',#55459,#42798,#42799);
#35783=AXIS2_PLACEMENT_3D('',#55460,#42800,#42801);
#35784=AXIS2_PLACEMENT_3D('',#55462,#42803,#42804);
#35785=AXIS2_PLACEMENT_3D('',#55466,#42806,#42807);
#35786=AXIS2_PLACEMENT_3D('',#55467,#42808,#42809);
#35787=AXIS2_PLACEMENT_3D('',#55469,#42811,#42812);
#35788=AXIS2_PLACEMENT_3D('',#55473,#42814,#42815);
#35789=AXIS2_PLACEMENT_3D('',#55474,#42816,#42817);
#35790=AXIS2_PLACEMENT_3D('',#55476,#42819,#42820);
#35791=AXIS2_PLACEMENT_3D('',#55478,#42821,#42822);
#35792=AXIS2_PLACEMENT_3D('',#55481,#42824,#42825);
#35793=AXIS2_PLACEMENT_3D('',#55482,#42826,#42827);
#35794=AXIS2_PLACEMENT_3D('',#55484,#42828,#42829);
#35795=AXIS2_PLACEMENT_3D('',#55487,#42831,#42832);
#35796=AXIS2_PLACEMENT_3D('',#55488,#42833,#42834);
#35797=AXIS2_PLACEMENT_3D('',#55490,#42835,#42836);
#35798=AXIS2_PLACEMENT_3D('',#55493,#42838,#42839);
#35799=AXIS2_PLACEMENT_3D('',#55494,#42840,#42841);
#35800=AXIS2_PLACEMENT_3D('',#55496,#42842,#42843);
#35801=AXIS2_PLACEMENT_3D('',#55499,#42845,#42846);
#35802=AXIS2_PLACEMENT_3D('',#55500,#42847,#42848);
#35803=AXIS2_PLACEMENT_3D('',#55502,#42849,#42850);
#35804=AXIS2_PLACEMENT_3D('',#55505,#42852,#42853);
#35805=AXIS2_PLACEMENT_3D('',#55506,#42854,#42855);
#35806=AXIS2_PLACEMENT_3D('',#55508,#42856,#42857);
#35807=AXIS2_PLACEMENT_3D('',#55511,#42859,#42860);
#35808=AXIS2_PLACEMENT_3D('',#55512,#42861,#42862);
#35809=AXIS2_PLACEMENT_3D('',#55514,#42863,#42864);
#35810=AXIS2_PLACEMENT_3D('',#55517,#42866,#42867);
#35811=AXIS2_PLACEMENT_3D('',#55518,#42868,#42869);
#35812=AXIS2_PLACEMENT_3D('',#55520,#42870,#42871);
#35813=AXIS2_PLACEMENT_3D('',#55523,#42873,#42874);
#35814=AXIS2_PLACEMENT_3D('',#55524,#42875,#42876);
#35815=AXIS2_PLACEMENT_3D('',#55526,#42877,#42878);
#35816=AXIS2_PLACEMENT_3D('',#55529,#42880,#42881);
#35817=AXIS2_PLACEMENT_3D('',#55530,#42882,#42883);
#35818=AXIS2_PLACEMENT_3D('',#55532,#42884,#42885);
#35819=AXIS2_PLACEMENT_3D('',#55535,#42887,#42888);
#35820=AXIS2_PLACEMENT_3D('',#55536,#42889,#42890);
#35821=AXIS2_PLACEMENT_3D('',#55538,#42892,#42893);
#35822=AXIS2_PLACEMENT_3D('',#55540,#42895,#42896);
#35823=AXIS2_PLACEMENT_3D('',#55541,#42897,#42898);
#35824=AXIS2_PLACEMENT_3D('',#55542,#42899,#42900);
#35825=AXIS2_PLACEMENT_3D('',#55552,#42905,#42906);
#35826=AXIS2_PLACEMENT_3D('',#55554,#42907,#42908);
#35827=AXIS2_PLACEMENT_3D('',#55556,#42909,#42910);
#35828=AXIS2_PLACEMENT_3D('',#55557,#42911,#42912);
#35829=AXIS2_PLACEMENT_3D('',#55567,#42917,#42918);
#35830=AXIS2_PLACEMENT_3D('',#55569,#42919,#42920);
#35831=AXIS2_PLACEMENT_3D('',#55571,#42921,#42922);
#35832=AXIS2_PLACEMENT_3D('',#55572,#42923,#42924);
#35833=AXIS2_PLACEMENT_3D('',#55575,#42927,#42928);
#35834=AXIS2_PLACEMENT_3D('',#55579,#42930,#42931);
#35835=AXIS2_PLACEMENT_3D('',#55580,#42932,#42933);
#35836=AXIS2_PLACEMENT_3D('',#55582,#42935,#42936);
#35837=AXIS2_PLACEMENT_3D('',#55586,#42938,#42939);
#35838=AXIS2_PLACEMENT_3D('',#55587,#42940,#42941);
#35839=AXIS2_PLACEMENT_3D('',#55589,#42943,#42944);
#35840=AXIS2_PLACEMENT_3D('',#55593,#42946,#42947);
#35841=AXIS2_PLACEMENT_3D('',#55594,#42948,#42949);
#35842=AXIS2_PLACEMENT_3D('',#55596,#42951,#42952);
#35843=AXIS2_PLACEMENT_3D('',#55600,#42954,#42955);
#35844=AXIS2_PLACEMENT_3D('',#55601,#42956,#42957);
#35845=AXIS2_PLACEMENT_3D('',#55603,#42959,#42960);
#35846=AXIS2_PLACEMENT_3D('',#55607,#42962,#42963);
#35847=AXIS2_PLACEMENT_3D('',#55608,#42964,#42965);
#35848=AXIS2_PLACEMENT_3D('',#55610,#42967,#42968);
#35849=AXIS2_PLACEMENT_3D('',#55614,#42970,#42971);
#35850=AXIS2_PLACEMENT_3D('',#55615,#42972,#42973);
#35851=AXIS2_PLACEMENT_3D('',#55617,#42975,#42976);
#35852=AXIS2_PLACEMENT_3D('',#55619,#42977,#42978);
#35853=AXIS2_PLACEMENT_3D('',#55622,#42980,#42981);
#35854=AXIS2_PLACEMENT_3D('',#55623,#42982,#42983);
#35855=AXIS2_PLACEMENT_3D('',#55625,#42984,#42985);
#35856=AXIS2_PLACEMENT_3D('',#55628,#42987,#42988);
#35857=AXIS2_PLACEMENT_3D('',#55629,#42989,#42990);
#35858=AXIS2_PLACEMENT_3D('',#55631,#42991,#42992);
#35859=AXIS2_PLACEMENT_3D('',#55634,#42994,#42995);
#35860=AXIS2_PLACEMENT_3D('',#55635,#42996,#42997);
#35861=AXIS2_PLACEMENT_3D('',#55637,#42998,#42999);
#35862=AXIS2_PLACEMENT_3D('',#55640,#43001,#43002);
#35863=AXIS2_PLACEMENT_3D('',#55641,#43003,#43004);
#35864=AXIS2_PLACEMENT_3D('',#55643,#43005,#43006);
#35865=AXIS2_PLACEMENT_3D('',#55646,#43008,#43009);
#35866=AXIS2_PLACEMENT_3D('',#55647,#43010,#43011);
#35867=AXIS2_PLACEMENT_3D('',#55649,#43012,#43013);
#35868=AXIS2_PLACEMENT_3D('',#55652,#43015,#43016);
#35869=AXIS2_PLACEMENT_3D('',#55653,#43017,#43018);
#35870=AXIS2_PLACEMENT_3D('',#55655,#43019,#43020);
#35871=AXIS2_PLACEMENT_3D('',#55658,#43022,#43023);
#35872=AXIS2_PLACEMENT_3D('',#55659,#43024,#43025);
#35873=AXIS2_PLACEMENT_3D('',#55661,#43026,#43027);
#35874=AXIS2_PLACEMENT_3D('',#55664,#43029,#43030);
#35875=AXIS2_PLACEMENT_3D('',#55665,#43031,#43032);
#35876=AXIS2_PLACEMENT_3D('',#55667,#43033,#43034);
#35877=AXIS2_PLACEMENT_3D('',#55670,#43036,#43037);
#35878=AXIS2_PLACEMENT_3D('',#55671,#43038,#43039);
#35879=AXIS2_PLACEMENT_3D('',#55673,#43040,#43041);
#35880=AXIS2_PLACEMENT_3D('',#55676,#43043,#43044);
#35881=AXIS2_PLACEMENT_3D('',#55677,#43045,#43046);
#35882=AXIS2_PLACEMENT_3D('',#55679,#43048,#43049);
#35883=AXIS2_PLACEMENT_3D('',#55681,#43051,#43052);
#35884=AXIS2_PLACEMENT_3D('',#55682,#43053,#43054);
#35885=AXIS2_PLACEMENT_3D('',#55683,#43055,#43056);
#35886=AXIS2_PLACEMENT_3D('',#55685,#43057,#43058);
#35887=AXIS2_PLACEMENT_3D('',#55688,#43060,#43061);
#35888=AXIS2_PLACEMENT_3D('',#55689,#43062,#43063);
#35889=AXIS2_PLACEMENT_3D('',#55691,#43064,#43065);
#35890=AXIS2_PLACEMENT_3D('',#55694,#43067,#43068);
#35891=AXIS2_PLACEMENT_3D('',#55695,#43069,#43070);
#35892=AXIS2_PLACEMENT_3D('',#55697,#43071,#43072);
#35893=AXIS2_PLACEMENT_3D('',#55700,#43074,#43075);
#35894=AXIS2_PLACEMENT_3D('',#55701,#43076,#43077);
#35895=AXIS2_PLACEMENT_3D('',#55703,#43078,#43079);
#35896=AXIS2_PLACEMENT_3D('',#55706,#43081,#43082);
#35897=AXIS2_PLACEMENT_3D('',#55707,#43083,#43084);
#35898=AXIS2_PLACEMENT_3D('',#55709,#43085,#43086);
#35899=AXIS2_PLACEMENT_3D('',#55712,#43088,#43089);
#35900=AXIS2_PLACEMENT_3D('',#55713,#43090,#43091);
#35901=AXIS2_PLACEMENT_3D('',#55715,#43092,#43093);
#35902=AXIS2_PLACEMENT_3D('',#55718,#43095,#43096);
#35903=AXIS2_PLACEMENT_3D('',#55719,#43097,#43098);
#35904=AXIS2_PLACEMENT_3D('',#55728,#43103,#43104);
#35905=AXIS2_PLACEMENT_3D('',#55734,#43108,#43109);
#35906=AXIS2_PLACEMENT_3D('',#55740,#43113,#43114);
#35907=AXIS2_PLACEMENT_3D('',#55743,#43117,#43118);
#35908=AXIS2_PLACEMENT_3D('',#55744,#43119,#43120);
#35909=AXIS2_PLACEMENT_3D('',#55745,#43121,#43122);
#35910=AXIS2_PLACEMENT_3D('',#55746,#43123,#43124);
#35911=AXIS2_PLACEMENT_3D('',#55755,#43129,#43130);
#35912=AXIS2_PLACEMENT_3D('',#55761,#43134,#43135);
#35913=AXIS2_PLACEMENT_3D('',#55769,#43139,#43140);
#35914=AXIS2_PLACEMENT_3D('',#55773,#43143,#43144);
#35915=AXIS2_PLACEMENT_3D('',#55778,#43147,#43148);
#35916=AXIS2_PLACEMENT_3D('',#55779,#43149,#43150);
#35917=AXIS2_PLACEMENT_3D('',#55788,#43156,#43157);
#35918=AXIS2_PLACEMENT_3D('',#55790,#43159,#43160);
#35919=AXIS2_PLACEMENT_3D('',#55792,#43162,#43163);
#35920=AXIS2_PLACEMENT_3D('',#55794,#43165,#43166);
#35921=AXIS2_PLACEMENT_3D('',#55795,#43167,#43168);
#35922=AXIS2_PLACEMENT_3D('',#55796,#43169,#43170);
#35923=AXIS2_PLACEMENT_3D('',#55797,#43171,#43172);
#35924=AXIS2_PLACEMENT_3D('',#55799,#43173,#43174);
#35925=AXIS2_PLACEMENT_3D('',#55802,#43176,#43177);
#35926=AXIS2_PLACEMENT_3D('',#55803,#43178,#43179);
#35927=AXIS2_PLACEMENT_3D('',#55805,#43180,#43181);
#35928=AXIS2_PLACEMENT_3D('',#55808,#43183,#43184);
#35929=AXIS2_PLACEMENT_3D('',#55809,#43185,#43186);
#35930=AXIS2_PLACEMENT_3D('',#55811,#43187,#43188);
#35931=AXIS2_PLACEMENT_3D('',#55814,#43190,#43191);
#35932=AXIS2_PLACEMENT_3D('',#55815,#43192,#43193);
#35933=AXIS2_PLACEMENT_3D('',#55817,#43194,#43195);
#35934=AXIS2_PLACEMENT_3D('',#55820,#43197,#43198);
#35935=AXIS2_PLACEMENT_3D('',#55821,#43199,#43200);
#35936=AXIS2_PLACEMENT_3D('',#55830,#43205,#43206);
#35937=AXIS2_PLACEMENT_3D('',#55836,#43210,#43211);
#35938=AXIS2_PLACEMENT_3D('',#55842,#43215,#43216);
#35939=AXIS2_PLACEMENT_3D('',#55845,#43219,#43220);
#35940=AXIS2_PLACEMENT_3D('',#55854,#43225,#43226);
#35941=AXIS2_PLACEMENT_3D('',#55860,#43230,#43231);
#35942=AXIS2_PLACEMENT_3D('',#55866,#43235,#43236);
#35943=AXIS2_PLACEMENT_3D('',#55869,#43239,#43240);
#35944=AXIS2_PLACEMENT_3D('',#55870,#43241,#43242);
#35945=AXIS2_PLACEMENT_3D('',#55871,#43243,#43244);
#35946=AXIS2_PLACEMENT_3D('',#55872,#43245,#43246);
#35947=AXIS2_PLACEMENT_3D('',#55873,#43247,#43248);
#35948=AXIS2_PLACEMENT_3D('',#55874,#43249,#43250);
#35949=AXIS2_PLACEMENT_3D('',#55875,#43251,#43252);
#35950=AXIS2_PLACEMENT_3D('',#55876,#43253,#43254);
#35951=AXIS2_PLACEMENT_3D('',#55877,#43255,#43256);
#35952=AXIS2_PLACEMENT_3D('',#55878,#43257,#43258);
#35953=AXIS2_PLACEMENT_3D('',#55879,#43259,#43260);
#35954=AXIS2_PLACEMENT_3D('',#55880,#43261,#43262);
#35955=AXIS2_PLACEMENT_3D('',#55881,#43263,#43264);
#35956=AXIS2_PLACEMENT_3D('',#55882,#43265,#43266);
#35957=AXIS2_PLACEMENT_3D('',#55883,#43267,#43268);
#35958=AXIS2_PLACEMENT_3D('',#55884,#43269,#43270);
#35959=AXIS2_PLACEMENT_3D('',#55885,#43271,#43272);
#35960=AXIS2_PLACEMENT_3D('',#55886,#43273,#43274);
#35961=AXIS2_PLACEMENT_3D('',#55887,#43275,#43276);
#35962=AXIS2_PLACEMENT_3D('',#55888,#43277,#43278);
#35963=AXIS2_PLACEMENT_3D('',#55889,#43279,#43280);
#35964=AXIS2_PLACEMENT_3D('',#55894,#43282,#43283);
#35965=AXIS2_PLACEMENT_3D('',#55919,#43285,#43286);
#35966=AXIS2_PLACEMENT_3D('',#55920,#43287,#43288);
#35967=AXIS2_PLACEMENT_3D('',#55944,#43290,#43291);
#35968=AXIS2_PLACEMENT_3D('',#55946,#43293,#43294);
#35969=AXIS2_PLACEMENT_3D('',#55952,#43298,#43299);
#35970=AXIS2_PLACEMENT_3D('',#55958,#43303,#43304);
#35971=AXIS2_PLACEMENT_3D('',#55977,#43305,#43306);
#35972=AXIS2_PLACEMENT_3D('',#55978,#43307,#43308);
#35973=AXIS2_PLACEMENT_3D('',#55979,#43309,#43310);
#35974=AXIS2_PLACEMENT_3D('',#55982,#43311,#43312);
#35975=AXIS2_PLACEMENT_3D('',#55983,#43313,#43314);
#35976=AXIS2_PLACEMENT_3D('',#55985,#43315,#43316);
#35977=AXIS2_PLACEMENT_3D('',#55986,#43317,#43318);
#35978=AXIS2_PLACEMENT_3D('',#55987,#43319,#43320);
#35979=AXIS2_PLACEMENT_3D('',#55989,#43321,#43322);
#35980=AXIS2_PLACEMENT_3D('',#55990,#43323,#43324);
#35981=AXIS2_PLACEMENT_3D('',#55992,#43325,#43326);
#35982=AXIS2_PLACEMENT_3D('',#55994,#43328,#43329);
#35983=AXIS2_PLACEMENT_3D('',#55996,#43330,#43331);
#35984=AXIS2_PLACEMENT_3D('',#55998,#43332,#43333);
#35985=AXIS2_PLACEMENT_3D('',#56000,#43334,#43335);
#35986=AXIS2_PLACEMENT_3D('',#56001,#43336,#43337);
#35987=AXIS2_PLACEMENT_3D('',#56002,#43338,#43339);
#35988=AXIS2_PLACEMENT_3D('',#56004,#43340,#43341);
#35989=AXIS2_PLACEMENT_3D('',#56005,#43342,#43343);
#35990=AXIS2_PLACEMENT_3D('',#56009,#43345,#43346);
#35991=AXIS2_PLACEMENT_3D('',#56010,#43347,#43348);
#35992=AXIS2_PLACEMENT_3D('',#56011,#43349,#43350);
#35993=AXIS2_PLACEMENT_3D('',#56014,#43351,#43352);
#35994=AXIS2_PLACEMENT_3D('',#56015,#43353,#43354);
#35995=AXIS2_PLACEMENT_3D('',#56017,#43356,#43357);
#35996=AXIS2_PLACEMENT_3D('',#56020,#43358,#43359);
#35997=AXIS2_PLACEMENT_3D('',#56022,#43361,#43362);
#35998=AXIS2_PLACEMENT_3D('',#56023,#43363,#43364);
#35999=AXIS2_PLACEMENT_3D('',#56026,#43365,#43366);
#36000=AXIS2_PLACEMENT_3D('',#56027,#43367,#43368);
#36001=AXIS2_PLACEMENT_3D('',#56029,#43370,#43371);
#36002=AXIS2_PLACEMENT_3D('',#56033,#43373,#43374);
#36003=AXIS2_PLACEMENT_3D('',#56034,#43375,#43376);
#36004=AXIS2_PLACEMENT_3D('',#56035,#43377,#43378);
#36005=AXIS2_PLACEMENT_3D('',#56038,#43380,#43381);
#36006=AXIS2_PLACEMENT_3D('',#56039,#43382,#43383);
#36007=AXIS2_PLACEMENT_3D('',#56040,#43384,#43385);
#36008=AXIS2_PLACEMENT_3D('',#56044,#43387,#43388);
#36009=AXIS2_PLACEMENT_3D('',#56057,#43390,#43391);
#36010=AXIS2_PLACEMENT_3D('',#56063,#43395,#43396);
#36011=AXIS2_PLACEMENT_3D('',#56067,#43399,#43400);
#36012=AXIS2_PLACEMENT_3D('',#56078,#43401,#43402);
#36013=AXIS2_PLACEMENT_3D('',#56079,#43403,#43404);
#36014=AXIS2_PLACEMENT_3D('',#56080,#43405,#43406);
#36015=AXIS2_PLACEMENT_3D('',#56081,#43407,#43408);
#36016=AXIS2_PLACEMENT_3D('',#56082,#43409,#43410);
#36017=AXIS2_PLACEMENT_3D('',#56083,#43411,#43412);
#36018=AXIS2_PLACEMENT_3D('',#56086,#43414,#43415);
#36019=AXIS2_PLACEMENT_3D('',#56087,#43416,#43417);
#36020=AXIS2_PLACEMENT_3D('',#56088,#43418,#43419);
#36021=AXIS2_PLACEMENT_3D('',#56090,#43420,#43421);
#36022=AXIS2_PLACEMENT_3D('',#56091,#43422,#43423);
#36023=AXIS2_PLACEMENT_3D('',#56092,#43424,#43425);
#36024=AXIS2_PLACEMENT_3D('',#56094,#43426,#43427);
#36025=AXIS2_PLACEMENT_3D('',#56095,#43428,#43429);
#36026=AXIS2_PLACEMENT_3D('',#56097,#43431,#43432);
#36027=AXIS2_PLACEMENT_3D('',#56100,#43434,#43435);
#36028=AXIS2_PLACEMENT_3D('',#56101,#43436,#43437);
#36029=AXIS2_PLACEMENT_3D('',#56103,#43438,#43439);
#36030=AXIS2_PLACEMENT_3D('',#56104,#43440,#43441);
#36031=AXIS2_PLACEMENT_3D('',#56105,#43442,#43443);
#36032=AXIS2_PLACEMENT_3D('',#56106,#43444,#43445);
#36033=AXIS2_PLACEMENT_3D('',#56107,#43446,#43447);
#36034=AXIS2_PLACEMENT_3D('',#56112,#43449,#43450);
#36035=AXIS2_PLACEMENT_3D('',#56137,#43452,#43453);
#36036=AXIS2_PLACEMENT_3D('',#56138,#43454,#43455);
#36037=AXIS2_PLACEMENT_3D('',#56141,#43456,#43457);
#36038=AXIS2_PLACEMENT_3D('',#56142,#43458,#43459);
#36039=AXIS2_PLACEMENT_3D('',#56145,#43461,#43462);
#36040=AXIS2_PLACEMENT_3D('',#56146,#43463,#43464);
#36041=AXIS2_PLACEMENT_3D('',#56149,#43466,#43467);
#36042=AXIS2_PLACEMENT_3D('',#56192,#43470,#43471);
#36043=AXIS2_PLACEMENT_3D('',#56193,#43472,#43473);
#36044=AXIS2_PLACEMENT_3D('',#56196,#43474,#43475);
#36045=AXIS2_PLACEMENT_3D('',#56197,#43476,#43477);
#36046=AXIS2_PLACEMENT_3D('',#56200,#43479,#43480);
#36047=AXIS2_PLACEMENT_3D('',#56201,#43481,#43482);
#36048=AXIS2_PLACEMENT_3D('',#56205,#43484,#43485);
#36049=AXIS2_PLACEMENT_3D('',#56206,#43486,#43487);
#36050=AXIS2_PLACEMENT_3D('',#56207,#43488,#43489);
#36051=AXIS2_PLACEMENT_3D('',#56208,#43490,#43491);
#36052=AXIS2_PLACEMENT_3D('',#56214,#43495,#43496);
#36053=AXIS2_PLACEMENT_3D('',#56216,#43497,#43498);
#36054=AXIS2_PLACEMENT_3D('',#56218,#43500,#43501);
#36055=AXIS2_PLACEMENT_3D('',#56222,#43504,#43505);
#36056=AXIS2_PLACEMENT_3D('',#56223,#43506,#43507);
#36057=AXIS2_PLACEMENT_3D('',#56224,#43508,#43509);
#36058=AXIS2_PLACEMENT_3D('',#56225,#43510,#43511);
#36059=AXIS2_PLACEMENT_3D('',#56228,#43512,#43513);
#36060=AXIS2_PLACEMENT_3D('',#56229,#43514,#43515);
#36061=AXIS2_PLACEMENT_3D('',#56232,#43517,#43518);
#36062=AXIS2_PLACEMENT_3D('',#56233,#43519,#43520);
#36063=AXIS2_PLACEMENT_3D('',#56235,#43521,#43522);
#36064=AXIS2_PLACEMENT_3D('',#56236,#43523,#43524);
#36065=AXIS2_PLACEMENT_3D('',#56239,#43525,#43526);
#36066=AXIS2_PLACEMENT_3D('',#56241,#43528,#43529);
#36067=AXIS2_PLACEMENT_3D('',#56242,#43530,#43531);
#36068=AXIS2_PLACEMENT_3D('',#56244,#43532,#43533);
#36069=AXIS2_PLACEMENT_3D('',#56246,#43534,#43535);
#36070=AXIS2_PLACEMENT_3D('',#56247,#43536,#43537);
#36071=AXIS2_PLACEMENT_3D('',#56248,#43538,#43539);
#36072=AXIS2_PLACEMENT_3D('',#56252,#43541,#43542);
#36073=AXIS2_PLACEMENT_3D('',#56253,#43543,#43544);
#36074=AXIS2_PLACEMENT_3D('',#56254,#43545,#43546);
#36075=AXIS2_PLACEMENT_3D('',#56256,#43547,#43548);
#36076=AXIS2_PLACEMENT_3D('',#56257,#43549,#43550);
#36077=AXIS2_PLACEMENT_3D('',#56258,#43551,#43552);
#36078=AXIS2_PLACEMENT_3D('',#56260,#43553,#43554);
#36079=AXIS2_PLACEMENT_3D('',#56261,#43555,#43556);
#36080=AXIS2_PLACEMENT_3D('',#56264,#43557,#43558);
#36081=AXIS2_PLACEMENT_3D('',#56265,#43559,#43560);
#36082=AXIS2_PLACEMENT_3D('',#56267,#43562,#43563);
#36083=AXIS2_PLACEMENT_3D('',#56271,#43565,#43566);
#36084=AXIS2_PLACEMENT_3D('',#56272,#43567,#43568);
#36085=AXIS2_PLACEMENT_3D('',#56273,#43569,#43570);
#36086=AXIS2_PLACEMENT_3D('',#56276,#43572,#43573);
#36087=AXIS2_PLACEMENT_3D('',#56277,#43574,#43575);
#36088=AXIS2_PLACEMENT_3D('',#56278,#43576,#43577);
#36089=AXIS2_PLACEMENT_3D('',#56282,#43579,#43580);
#36090=AXIS2_PLACEMENT_3D('',#56295,#43582,#43583);
#36091=AXIS2_PLACEMENT_3D('',#56301,#43587,#43588);
#36092=AXIS2_PLACEMENT_3D('',#56305,#43591,#43592);
#36093=AXIS2_PLACEMENT_3D('',#56316,#43593,#43594);
#36094=AXIS2_PLACEMENT_3D('',#56317,#43595,#43596);
#36095=AXIS2_PLACEMENT_3D('',#56318,#43597,#43598);
#36096=AXIS2_PLACEMENT_3D('',#56319,#43599,#43600);
#36097=AXIS2_PLACEMENT_3D('',#56320,#43601,#43602);
#36098=AXIS2_PLACEMENT_3D('',#56321,#43603,#43604);
#36099=AXIS2_PLACEMENT_3D('',#56323,#43605,#43606);
#36100=AXIS2_PLACEMENT_3D('',#56324,#43607,#43608);
#36101=AXIS2_PLACEMENT_3D('',#56325,#43609,#43610);
#36102=AXIS2_PLACEMENT_3D('',#56327,#43611,#43612);
#36103=AXIS2_PLACEMENT_3D('',#56328,#43613,#43614);
#36104=AXIS2_PLACEMENT_3D('',#56330,#43616,#43617);
#36105=AXIS2_PLACEMENT_3D('',#56333,#43619,#43620);
#36106=AXIS2_PLACEMENT_3D('',#56334,#43621,#43622);
#36107=AXIS2_PLACEMENT_3D('',#56336,#43623,#43624);
#36108=AXIS2_PLACEMENT_3D('',#56337,#43625,#43626);
#36109=AXIS2_PLACEMENT_3D('',#56338,#43627,#43628);
#36110=AXIS2_PLACEMENT_3D('',#56339,#43629,#43630);
#36111=AXIS2_PLACEMENT_3D('',#56340,#43631,#43632);
#36112=AXIS2_PLACEMENT_3D('',#56349,#43637,#43638);
#36113=AXIS2_PLACEMENT_3D('',#56355,#43642,#43643);
#36114=AXIS2_PLACEMENT_3D('',#56361,#43647,#43648);
#36115=AXIS2_PLACEMENT_3D('',#56363,#43649,#43650);
#36116=AXIS2_PLACEMENT_3D('',#56364,#43651,#43652);
#36117=AXIS2_PLACEMENT_3D('',#56365,#43653,#43654);
#36118=AXIS2_PLACEMENT_3D('',#56366,#43655,#43656);
#36119=AXIS2_PLACEMENT_3D('',#56367,#43657,#43658);
#36120=AXIS2_PLACEMENT_3D('',#56369,#43659,#43660);
#36121=AXIS2_PLACEMENT_3D('',#56371,#43662,#43663);
#36122=AXIS2_PLACEMENT_3D('',#56372,#43664,#43665);
#36123=AXIS2_PLACEMENT_3D('',#56373,#43666,#43667);
#36124=AXIS2_PLACEMENT_3D('',#56375,#43668,#43669);
#36125=AXIS2_PLACEMENT_3D('',#56378,#43671,#43672);
#36126=AXIS2_PLACEMENT_3D('',#56379,#43673,#43674);
#36127=AXIS2_PLACEMENT_3D('',#56381,#43675,#43676);
#36128=AXIS2_PLACEMENT_3D('',#56384,#43678,#43679);
#36129=AXIS2_PLACEMENT_3D('',#56385,#43680,#43681);
#36130=AXIS2_PLACEMENT_3D('',#56386,#43682,#43683);
#36131=AXIS2_PLACEMENT_3D('',#56387,#43684,#43685);
#36132=AXIS2_PLACEMENT_3D('',#56388,#43686,#43687);
#36133=AXIS2_PLACEMENT_3D('',#56389,#43688,#43689);
#36134=AXIS2_PLACEMENT_3D('',#56390,#43690,#43691);
#36135=AXIS2_PLACEMENT_3D('',#56391,#43692,#43693);
#36136=AXIS2_PLACEMENT_3D('',#56392,#43694,#43695);
#36137=AXIS2_PLACEMENT_3D('',#56393,#43696,#43697);
#36138=AXIS2_PLACEMENT_3D('',#56394,#43698,#43699);
#36139=AXIS2_PLACEMENT_3D('',#56395,#43700,#43701);
#36140=AXIS2_PLACEMENT_3D('',#56396,#43702,#43703);
#36141=AXIS2_PLACEMENT_3D('',#56397,#43704,#43705);
#36142=AXIS2_PLACEMENT_3D('',#56398,#43706,#43707);
#36143=AXIS2_PLACEMENT_3D('',#56399,#43708,#43709);
#36144=AXIS2_PLACEMENT_3D('',#56400,#43710,#43711);
#36145=AXIS2_PLACEMENT_3D('',#56401,#43712,#43713);
#36146=AXIS2_PLACEMENT_3D('',#56402,#43714,#43715);
#36147=AXIS2_PLACEMENT_3D('',#56403,#43716,#43717);
#36148=AXIS2_PLACEMENT_3D('',#56404,#43718,#43719);
#36149=AXIS2_PLACEMENT_3D('',#56405,#43720,#43721);
#36150=AXIS2_PLACEMENT_3D('',#56407,#43722,#43723);
#36151=AXIS2_PLACEMENT_3D('',#56409,#43724,#43725);
#36152=AXIS2_PLACEMENT_3D('',#56411,#43726,#43727);
#36153=AXIS2_PLACEMENT_3D('',#56412,#43728,#43729);
#36154=AXIS2_PLACEMENT_3D('',#56413,#43730,#43731);
#36155=AXIS2_PLACEMENT_3D('',#56416,#43733,#43734);
#36156=AXIS2_PLACEMENT_3D('',#56417,#43735,#43736);
#36157=AXIS2_PLACEMENT_3D('',#56425,#43740,#43741);
#36158=AXIS2_PLACEMENT_3D('',#56426,#43742,#43743);
#36159=AXIS2_PLACEMENT_3D('',#56428,#43744,#43745);
#36160=AXIS2_PLACEMENT_3D('',#56429,#43746,#43747);
#36161=AXIS2_PLACEMENT_3D('',#56430,#43748,#43749);
#36162=AXIS2_PLACEMENT_3D('',#56433,#43750,#43751);
#36163=AXIS2_PLACEMENT_3D('',#56435,#43752,#43753);
#36164=AXIS2_PLACEMENT_3D('',#56437,#43754,#43755);
#36165=AXIS2_PLACEMENT_3D('',#56439,#43756,#43757);
#36166=AXIS2_PLACEMENT_3D('',#56441,#43758,#43759);
#36167=AXIS2_PLACEMENT_3D('',#56443,#43760,#43761);
#36168=AXIS2_PLACEMENT_3D('',#56445,#43762,#43763);
#36169=AXIS2_PLACEMENT_3D('',#56447,#43764,#43765);
#36170=AXIS2_PLACEMENT_3D('',#56449,#43766,#43767);
#36171=AXIS2_PLACEMENT_3D('',#56451,#43768,#43769);
#36172=AXIS2_PLACEMENT_3D('',#56453,#43770,#43771);
#36173=AXIS2_PLACEMENT_3D('',#56455,#43772,#43773);
#36174=AXIS2_PLACEMENT_3D('',#56457,#43774,#43775);
#36175=AXIS2_PLACEMENT_3D('',#56459,#43776,#43777);
#36176=AXIS2_PLACEMENT_3D('',#56461,#43778,#43779);
#36177=AXIS2_PLACEMENT_3D('',#56463,#43780,#43781);
#36178=AXIS2_PLACEMENT_3D('',#56465,#43782,#43783);
#36179=AXIS2_PLACEMENT_3D('',#56467,#43784,#43785);
#36180=AXIS2_PLACEMENT_3D('',#56469,#43786,#43787);
#36181=AXIS2_PLACEMENT_3D('',#56471,#43788,#43789);
#36182=AXIS2_PLACEMENT_3D('',#56473,#43790,#43791);
#36183=AXIS2_PLACEMENT_3D('',#56475,#43792,#43793);
#36184=AXIS2_PLACEMENT_3D('',#56477,#43794,#43795);
#36185=AXIS2_PLACEMENT_3D('',#56479,#43796,#43797);
#36186=AXIS2_PLACEMENT_3D('',#56481,#43798,#43799);
#36187=AXIS2_PLACEMENT_3D('',#56483,#43800,#43801);
#36188=AXIS2_PLACEMENT_3D('',#56485,#43802,#43803);
#36189=AXIS2_PLACEMENT_3D('',#56487,#43804,#43805);
#36190=AXIS2_PLACEMENT_3D('',#56489,#43806,#43807);
#36191=AXIS2_PLACEMENT_3D('',#56491,#43808,#43809);
#36192=AXIS2_PLACEMENT_3D('',#56493,#43810,#43811);
#36193=AXIS2_PLACEMENT_3D('',#56495,#43812,#43813);
#36194=AXIS2_PLACEMENT_3D('',#56497,#43814,#43815);
#36195=AXIS2_PLACEMENT_3D('',#56499,#43816,#43817);
#36196=AXIS2_PLACEMENT_3D('',#56501,#43818,#43819);
#36197=AXIS2_PLACEMENT_3D('',#56503,#43820,#43821);
#36198=AXIS2_PLACEMENT_3D('',#56505,#43822,#43823);
#36199=AXIS2_PLACEMENT_3D('',#56507,#43824,#43825);
#36200=AXIS2_PLACEMENT_3D('',#56509,#43826,#43827);
#36201=AXIS2_PLACEMENT_3D('',#56511,#43828,#43829);
#36202=AXIS2_PLACEMENT_3D('',#56513,#43830,#43831);
#36203=AXIS2_PLACEMENT_3D('',#56515,#43832,#43833);
#36204=AXIS2_PLACEMENT_3D('',#56517,#43834,#43835);
#36205=AXIS2_PLACEMENT_3D('',#56519,#43836,#43837);
#36206=AXIS2_PLACEMENT_3D('',#56521,#43838,#43839);
#36207=AXIS2_PLACEMENT_3D('',#56523,#43840,#43841);
#36208=AXIS2_PLACEMENT_3D('',#56525,#43842,#43843);
#36209=AXIS2_PLACEMENT_3D('',#56527,#43844,#43845);
#36210=AXIS2_PLACEMENT_3D('',#56529,#43846,#43847);
#36211=AXIS2_PLACEMENT_3D('',#56531,#43848,#43849);
#36212=AXIS2_PLACEMENT_3D('',#56533,#43850,#43851);
#36213=AXIS2_PLACEMENT_3D('',#56535,#43852,#43853);
#36214=AXIS2_PLACEMENT_3D('',#56537,#43854,#43855);
#36215=AXIS2_PLACEMENT_3D('',#56539,#43856,#43857);
#36216=AXIS2_PLACEMENT_3D('',#56541,#43858,#43859);
#36217=AXIS2_PLACEMENT_3D('',#56543,#43860,#43861);
#36218=AXIS2_PLACEMENT_3D('',#56545,#43862,#43863);
#36219=AXIS2_PLACEMENT_3D('',#56547,#43864,#43865);
#36220=AXIS2_PLACEMENT_3D('',#56549,#43866,#43867);
#36221=AXIS2_PLACEMENT_3D('',#56551,#43868,#43869);
#36222=AXIS2_PLACEMENT_3D('',#56553,#43870,#43871);
#36223=AXIS2_PLACEMENT_3D('',#56555,#43872,#43873);
#36224=AXIS2_PLACEMENT_3D('',#56557,#43874,#43875);
#36225=AXIS2_PLACEMENT_3D('',#56559,#43876,#43877);
#36226=AXIS2_PLACEMENT_3D('',#56561,#43878,#43879);
#36227=AXIS2_PLACEMENT_3D('',#56563,#43880,#43881);
#36228=AXIS2_PLACEMENT_3D('',#56565,#43882,#43883);
#36229=AXIS2_PLACEMENT_3D('',#56567,#43884,#43885);
#36230=AXIS2_PLACEMENT_3D('',#56569,#43886,#43887);
#36231=AXIS2_PLACEMENT_3D('',#56571,#43888,#43889);
#36232=AXIS2_PLACEMENT_3D('',#56573,#43890,#43891);
#36233=AXIS2_PLACEMENT_3D('',#56575,#43892,#43893);
#36234=AXIS2_PLACEMENT_3D('',#56577,#43894,#43895);
#36235=AXIS2_PLACEMENT_3D('',#56579,#43896,#43897);
#36236=AXIS2_PLACEMENT_3D('',#56581,#43898,#43899);
#36237=AXIS2_PLACEMENT_3D('',#56583,#43900,#43901);
#36238=AXIS2_PLACEMENT_3D('',#56585,#43902,#43903);
#36239=AXIS2_PLACEMENT_3D('',#56587,#43904,#43905);
#36240=AXIS2_PLACEMENT_3D('',#56589,#43906,#43907);
#36241=AXIS2_PLACEMENT_3D('',#56591,#43908,#43909);
#36242=AXIS2_PLACEMENT_3D('',#56593,#43910,#43911);
#36243=AXIS2_PLACEMENT_3D('',#56595,#43912,#43913);
#36244=AXIS2_PLACEMENT_3D('',#56597,#43914,#43915);
#36245=AXIS2_PLACEMENT_3D('',#56599,#43916,#43917);
#36246=AXIS2_PLACEMENT_3D('',#56601,#43918,#43919);
#36247=AXIS2_PLACEMENT_3D('',#56603,#43920,#43921);
#36248=AXIS2_PLACEMENT_3D('',#56605,#43922,#43923);
#36249=AXIS2_PLACEMENT_3D('',#56607,#43924,#43925);
#36250=AXIS2_PLACEMENT_3D('',#56609,#43926,#43927);
#36251=AXIS2_PLACEMENT_3D('',#56611,#43928,#43929);
#36252=AXIS2_PLACEMENT_3D('',#56613,#43930,#43931);
#36253=AXIS2_PLACEMENT_3D('',#56615,#43932,#43933);
#36254=AXIS2_PLACEMENT_3D('',#56617,#43934,#43935);
#36255=AXIS2_PLACEMENT_3D('',#56619,#43936,#43937);
#36256=AXIS2_PLACEMENT_3D('',#56621,#43938,#43939);
#36257=AXIS2_PLACEMENT_3D('',#56623,#43940,#43941);
#36258=AXIS2_PLACEMENT_3D('',#56625,#43942,#43943);
#36259=AXIS2_PLACEMENT_3D('',#56627,#43944,#43945);
#36260=AXIS2_PLACEMENT_3D('',#56629,#43946,#43947);
#36261=AXIS2_PLACEMENT_3D('',#56631,#43948,#43949);
#36262=AXIS2_PLACEMENT_3D('',#56633,#43950,#43951);
#36263=AXIS2_PLACEMENT_3D('',#56635,#43952,#43953);
#36264=AXIS2_PLACEMENT_3D('',#56637,#43954,#43955);
#36265=AXIS2_PLACEMENT_3D('',#56639,#43956,#43957);
#36266=AXIS2_PLACEMENT_3D('',#56641,#43958,#43959);
#36267=AXIS2_PLACEMENT_3D('',#56643,#43960,#43961);
#36268=AXIS2_PLACEMENT_3D('',#56645,#43962,#43963);
#36269=AXIS2_PLACEMENT_3D('',#56647,#43964,#43965);
#36270=AXIS2_PLACEMENT_3D('',#56649,#43966,#43967);
#36271=AXIS2_PLACEMENT_3D('',#56651,#43968,#43969);
#36272=AXIS2_PLACEMENT_3D('',#56653,#43970,#43971);
#36273=AXIS2_PLACEMENT_3D('',#56655,#43972,#43973);
#36274=AXIS2_PLACEMENT_3D('',#56657,#43974,#43975);
#36275=AXIS2_PLACEMENT_3D('',#56659,#43976,#43977);
#36276=AXIS2_PLACEMENT_3D('',#56661,#43978,#43979);
#36277=AXIS2_PLACEMENT_3D('',#56663,#43980,#43981);
#36278=AXIS2_PLACEMENT_3D('',#56665,#43982,#43983);
#36279=AXIS2_PLACEMENT_3D('',#56667,#43984,#43985);
#36280=AXIS2_PLACEMENT_3D('',#56669,#43986,#43987);
#36281=AXIS2_PLACEMENT_3D('',#56671,#43988,#43989);
#36282=AXIS2_PLACEMENT_3D('',#56673,#43990,#43991);
#36283=AXIS2_PLACEMENT_3D('',#56675,#43992,#43993);
#36284=AXIS2_PLACEMENT_3D('',#56677,#43994,#43995);
#36285=AXIS2_PLACEMENT_3D('',#56679,#43996,#43997);
#36286=AXIS2_PLACEMENT_3D('',#56681,#43998,#43999);
#36287=AXIS2_PLACEMENT_3D('',#56683,#44000,#44001);
#36288=AXIS2_PLACEMENT_3D('',#56685,#44002,#44003);
#36289=AXIS2_PLACEMENT_3D('',#56687,#44004,#44005);
#36290=AXIS2_PLACEMENT_3D('',#56689,#44006,#44007);
#36291=AXIS2_PLACEMENT_3D('',#56691,#44008,#44009);
#36292=AXIS2_PLACEMENT_3D('',#56693,#44010,#44011);
#36293=AXIS2_PLACEMENT_3D('',#56695,#44012,#44013);
#36294=AXIS2_PLACEMENT_3D('',#56697,#44014,#44015);
#36295=AXIS2_PLACEMENT_3D('',#56699,#44016,#44017);
#36296=AXIS2_PLACEMENT_3D('',#56701,#44018,#44019);
#36297=AXIS2_PLACEMENT_3D('',#56703,#44020,#44021);
#36298=AXIS2_PLACEMENT_3D('',#56705,#44022,#44023);
#36299=AXIS2_PLACEMENT_3D('',#56707,#44024,#44025);
#36300=AXIS2_PLACEMENT_3D('',#56709,#44026,#44027);
#36301=AXIS2_PLACEMENT_3D('',#56711,#44028,#44029);
#36302=AXIS2_PLACEMENT_3D('',#56713,#44030,#44031);
#36303=AXIS2_PLACEMENT_3D('',#56715,#44032,#44033);
#36304=AXIS2_PLACEMENT_3D('',#56717,#44034,#44035);
#36305=AXIS2_PLACEMENT_3D('',#56719,#44036,#44037);
#36306=AXIS2_PLACEMENT_3D('',#56721,#44038,#44039);
#36307=AXIS2_PLACEMENT_3D('',#56723,#44040,#44041);
#36308=AXIS2_PLACEMENT_3D('',#56725,#44042,#44043);
#36309=AXIS2_PLACEMENT_3D('',#56727,#44044,#44045);
#36310=AXIS2_PLACEMENT_3D('',#56729,#44046,#44047);
#36311=AXIS2_PLACEMENT_3D('',#56731,#44048,#44049);
#36312=AXIS2_PLACEMENT_3D('',#56733,#44050,#44051);
#36313=AXIS2_PLACEMENT_3D('',#56735,#44052,#44053);
#36314=AXIS2_PLACEMENT_3D('',#56737,#44054,#44055);
#36315=AXIS2_PLACEMENT_3D('',#56739,#44056,#44057);
#36316=AXIS2_PLACEMENT_3D('',#56741,#44058,#44059);
#36317=AXIS2_PLACEMENT_3D('',#56743,#44060,#44061);
#36318=AXIS2_PLACEMENT_3D('',#56745,#44062,#44063);
#36319=AXIS2_PLACEMENT_3D('',#56747,#44064,#44065);
#36320=AXIS2_PLACEMENT_3D('',#56749,#44066,#44067);
#36321=AXIS2_PLACEMENT_3D('',#56751,#44068,#44069);
#36322=AXIS2_PLACEMENT_3D('',#56753,#44070,#44071);
#36323=AXIS2_PLACEMENT_3D('',#56755,#44072,#44073);
#36324=AXIS2_PLACEMENT_3D('',#56757,#44074,#44075);
#36325=AXIS2_PLACEMENT_3D('',#56759,#44076,#44077);
#36326=AXIS2_PLACEMENT_3D('',#56761,#44078,#44079);
#36327=AXIS2_PLACEMENT_3D('',#56763,#44080,#44081);
#36328=AXIS2_PLACEMENT_3D('',#56765,#44082,#44083);
#36329=AXIS2_PLACEMENT_3D('',#56767,#44084,#44085);
#36330=AXIS2_PLACEMENT_3D('',#56769,#44086,#44087);
#36331=AXIS2_PLACEMENT_3D('',#56771,#44088,#44089);
#36332=AXIS2_PLACEMENT_3D('',#56773,#44090,#44091);
#36333=AXIS2_PLACEMENT_3D('',#56775,#44092,#44093);
#36334=AXIS2_PLACEMENT_3D('',#56777,#44094,#44095);
#36335=AXIS2_PLACEMENT_3D('',#56779,#44096,#44097);
#36336=AXIS2_PLACEMENT_3D('',#56781,#44098,#44099);
#36337=AXIS2_PLACEMENT_3D('',#56783,#44100,#44101);
#36338=AXIS2_PLACEMENT_3D('',#56785,#44102,#44103);
#36339=AXIS2_PLACEMENT_3D('',#56787,#44104,#44105);
#36340=AXIS2_PLACEMENT_3D('',#56789,#44106,#44107);
#36341=AXIS2_PLACEMENT_3D('',#56791,#44108,#44109);
#36342=AXIS2_PLACEMENT_3D('',#56793,#44110,#44111);
#36343=AXIS2_PLACEMENT_3D('',#56795,#44112,#44113);
#36344=AXIS2_PLACEMENT_3D('',#56797,#44114,#44115);
#36345=AXIS2_PLACEMENT_3D('',#56799,#44116,#44117);
#36346=AXIS2_PLACEMENT_3D('',#56801,#44118,#44119);
#36347=AXIS2_PLACEMENT_3D('',#56803,#44120,#44121);
#36348=AXIS2_PLACEMENT_3D('',#56805,#44122,#44123);
#36349=AXIS2_PLACEMENT_3D('',#56807,#44124,#44125);
#36350=AXIS2_PLACEMENT_3D('',#56809,#44126,#44127);
#36351=AXIS2_PLACEMENT_3D('',#56811,#44128,#44129);
#36352=AXIS2_PLACEMENT_3D('',#56813,#44130,#44131);
#36353=AXIS2_PLACEMENT_3D('',#56814,#44132,#44133);
#36354=AXIS2_PLACEMENT_3D('',#56815,#44134,#44135);
#36355=AXIS2_PLACEMENT_3D('',#56821,#44139,#44140);
#36356=AXIS2_PLACEMENT_3D('',#56825,#44143,#44144);
#36357=AXIS2_PLACEMENT_3D('',#56827,#44145,#44146);
#36358=AXIS2_PLACEMENT_3D('',#56829,#44148,#44149);
#36359=AXIS2_PLACEMENT_3D('',#56831,#44151,#44152);
#36360=AXIS2_PLACEMENT_3D('',#56835,#44154,#44155);
#36361=AXIS2_PLACEMENT_3D('',#56837,#44157,#44158);
#36362=AXIS2_PLACEMENT_3D('',#56839,#44159,#44160);
#36363=AXIS2_PLACEMENT_3D('',#56841,#44162,#44163);
#36364=AXIS2_PLACEMENT_3D('',#56844,#44165,#44166);
#36365=AXIS2_PLACEMENT_3D('',#56845,#44167,#44168);
#36366=AXIS2_PLACEMENT_3D('',#56849,#44170,#44171);
#36367=AXIS2_PLACEMENT_3D('',#56851,#44173,#44174);
#36368=AXIS2_PLACEMENT_3D('',#56853,#44175,#44176);
#36369=AXIS2_PLACEMENT_3D('',#56855,#44178,#44179);
#36370=AXIS2_PLACEMENT_3D('',#56858,#44181,#44182);
#36371=AXIS2_PLACEMENT_3D('',#56859,#44183,#44184);
#36372=AXIS2_PLACEMENT_3D('',#56863,#44186,#44187);
#36373=AXIS2_PLACEMENT_3D('',#56865,#44189,#44190);
#36374=AXIS2_PLACEMENT_3D('',#56867,#44191,#44192);
#36375=AXIS2_PLACEMENT_3D('',#56869,#44194,#44195);
#36376=AXIS2_PLACEMENT_3D('',#56872,#44197,#44198);
#36377=AXIS2_PLACEMENT_3D('',#56873,#44199,#44200);
#36378=AXIS2_PLACEMENT_3D('',#56877,#44202,#44203);
#36379=AXIS2_PLACEMENT_3D('',#56879,#44205,#44206);
#36380=AXIS2_PLACEMENT_3D('',#56881,#44207,#44208);
#36381=AXIS2_PLACEMENT_3D('',#56883,#44210,#44211);
#36382=AXIS2_PLACEMENT_3D('',#56886,#44213,#44214);
#36383=AXIS2_PLACEMENT_3D('',#56887,#44215,#44216);
#36384=AXIS2_PLACEMENT_3D('',#56891,#44218,#44219);
#36385=AXIS2_PLACEMENT_3D('',#56893,#44221,#44222);
#36386=AXIS2_PLACEMENT_3D('',#56895,#44223,#44224);
#36387=AXIS2_PLACEMENT_3D('',#56897,#44226,#44227);
#36388=AXIS2_PLACEMENT_3D('',#56900,#44229,#44230);
#36389=AXIS2_PLACEMENT_3D('',#56901,#44231,#44232);
#36390=AXIS2_PLACEMENT_3D('',#56905,#44234,#44235);
#36391=AXIS2_PLACEMENT_3D('',#56907,#44237,#44238);
#36392=AXIS2_PLACEMENT_3D('',#56909,#44239,#44240);
#36393=AXIS2_PLACEMENT_3D('',#56911,#44242,#44243);
#36394=AXIS2_PLACEMENT_3D('',#56914,#44245,#44246);
#36395=AXIS2_PLACEMENT_3D('',#56915,#44247,#44248);
#36396=AXIS2_PLACEMENT_3D('',#56919,#44250,#44251);
#36397=AXIS2_PLACEMENT_3D('',#56921,#44253,#44254);
#36398=AXIS2_PLACEMENT_3D('',#56923,#44255,#44256);
#36399=AXIS2_PLACEMENT_3D('',#56925,#44258,#44259);
#36400=AXIS2_PLACEMENT_3D('',#56928,#44261,#44262);
#36401=AXIS2_PLACEMENT_3D('',#56929,#44263,#44264);
#36402=AXIS2_PLACEMENT_3D('',#56933,#44266,#44267);
#36403=AXIS2_PLACEMENT_3D('',#56935,#44269,#44270);
#36404=AXIS2_PLACEMENT_3D('',#56937,#44271,#44272);
#36405=AXIS2_PLACEMENT_3D('',#56939,#44274,#44275);
#36406=AXIS2_PLACEMENT_3D('',#56942,#44277,#44278);
#36407=AXIS2_PLACEMENT_3D('',#56943,#44279,#44280);
#36408=AXIS2_PLACEMENT_3D('',#56947,#44282,#44283);
#36409=AXIS2_PLACEMENT_3D('',#56949,#44285,#44286);
#36410=AXIS2_PLACEMENT_3D('',#56951,#44287,#44288);
#36411=AXIS2_PLACEMENT_3D('',#56953,#44290,#44291);
#36412=AXIS2_PLACEMENT_3D('',#56956,#44293,#44294);
#36413=AXIS2_PLACEMENT_3D('',#56957,#44295,#44296);
#36414=AXIS2_PLACEMENT_3D('',#56961,#44298,#44299);
#36415=AXIS2_PLACEMENT_3D('',#56963,#44301,#44302);
#36416=AXIS2_PLACEMENT_3D('',#56965,#44303,#44304);
#36417=AXIS2_PLACEMENT_3D('',#56967,#44306,#44307);
#36418=AXIS2_PLACEMENT_3D('',#56970,#44309,#44310);
#36419=AXIS2_PLACEMENT_3D('',#56971,#44311,#44312);
#36420=AXIS2_PLACEMENT_3D('',#56975,#44314,#44315);
#36421=AXIS2_PLACEMENT_3D('',#56977,#44317,#44318);
#36422=AXIS2_PLACEMENT_3D('',#56979,#44319,#44320);
#36423=AXIS2_PLACEMENT_3D('',#56981,#44322,#44323);
#36424=AXIS2_PLACEMENT_3D('',#56984,#44325,#44326);
#36425=AXIS2_PLACEMENT_3D('',#56985,#44327,#44328);
#36426=AXIS2_PLACEMENT_3D('',#56989,#44330,#44331);
#36427=AXIS2_PLACEMENT_3D('',#56991,#44333,#44334);
#36428=AXIS2_PLACEMENT_3D('',#56993,#44335,#44336);
#36429=AXIS2_PLACEMENT_3D('',#56995,#44338,#44339);
#36430=AXIS2_PLACEMENT_3D('',#56998,#44341,#44342);
#36431=AXIS2_PLACEMENT_3D('',#56999,#44343,#44344);
#36432=AXIS2_PLACEMENT_3D('',#57003,#44346,#44347);
#36433=AXIS2_PLACEMENT_3D('',#57005,#44349,#44350);
#36434=AXIS2_PLACEMENT_3D('',#57007,#44351,#44352);
#36435=AXIS2_PLACEMENT_3D('',#57009,#44354,#44355);
#36436=AXIS2_PLACEMENT_3D('',#57012,#44357,#44358);
#36437=AXIS2_PLACEMENT_3D('',#57013,#44359,#44360);
#36438=AXIS2_PLACEMENT_3D('',#57017,#44362,#44363);
#36439=AXIS2_PLACEMENT_3D('',#57019,#44365,#44366);
#36440=AXIS2_PLACEMENT_3D('',#57021,#44367,#44368);
#36441=AXIS2_PLACEMENT_3D('',#57023,#44370,#44371);
#36442=AXIS2_PLACEMENT_3D('',#57026,#44373,#44374);
#36443=AXIS2_PLACEMENT_3D('',#57027,#44375,#44376);
#36444=AXIS2_PLACEMENT_3D('',#57031,#44378,#44379);
#36445=AXIS2_PLACEMENT_3D('',#57033,#44381,#44382);
#36446=AXIS2_PLACEMENT_3D('',#57035,#44383,#44384);
#36447=AXIS2_PLACEMENT_3D('',#57037,#44386,#44387);
#36448=AXIS2_PLACEMENT_3D('',#57040,#44389,#44390);
#36449=AXIS2_PLACEMENT_3D('',#57041,#44391,#44392);
#36450=AXIS2_PLACEMENT_3D('',#57045,#44394,#44395);
#36451=AXIS2_PLACEMENT_3D('',#57047,#44397,#44398);
#36452=AXIS2_PLACEMENT_3D('',#57049,#44399,#44400);
#36453=AXIS2_PLACEMENT_3D('',#57051,#44402,#44403);
#36454=AXIS2_PLACEMENT_3D('',#57054,#44405,#44406);
#36455=AXIS2_PLACEMENT_3D('',#57055,#44407,#44408);
#36456=AXIS2_PLACEMENT_3D('',#57059,#44410,#44411);
#36457=AXIS2_PLACEMENT_3D('',#57061,#44413,#44414);
#36458=AXIS2_PLACEMENT_3D('',#57063,#44415,#44416);
#36459=AXIS2_PLACEMENT_3D('',#57065,#44418,#44419);
#36460=AXIS2_PLACEMENT_3D('',#57068,#44421,#44422);
#36461=AXIS2_PLACEMENT_3D('',#57069,#44423,#44424);
#36462=AXIS2_PLACEMENT_3D('',#57073,#44426,#44427);
#36463=AXIS2_PLACEMENT_3D('',#57075,#44429,#44430);
#36464=AXIS2_PLACEMENT_3D('',#57077,#44431,#44432);
#36465=AXIS2_PLACEMENT_3D('',#57079,#44434,#44435);
#36466=AXIS2_PLACEMENT_3D('',#57082,#44437,#44438);
#36467=AXIS2_PLACEMENT_3D('',#57083,#44439,#44440);
#36468=AXIS2_PLACEMENT_3D('',#57087,#44442,#44443);
#36469=AXIS2_PLACEMENT_3D('',#57089,#44445,#44446);
#36470=AXIS2_PLACEMENT_3D('',#57091,#44447,#44448);
#36471=AXIS2_PLACEMENT_3D('',#57093,#44450,#44451);
#36472=AXIS2_PLACEMENT_3D('',#57096,#44453,#44454);
#36473=AXIS2_PLACEMENT_3D('',#57097,#44455,#44456);
#36474=AXIS2_PLACEMENT_3D('',#57101,#44458,#44459);
#36475=AXIS2_PLACEMENT_3D('',#57103,#44461,#44462);
#36476=AXIS2_PLACEMENT_3D('',#57105,#44463,#44464);
#36477=AXIS2_PLACEMENT_3D('',#57107,#44466,#44467);
#36478=AXIS2_PLACEMENT_3D('',#57110,#44469,#44470);
#36479=AXIS2_PLACEMENT_3D('',#57111,#44471,#44472);
#36480=AXIS2_PLACEMENT_3D('',#57115,#44474,#44475);
#36481=AXIS2_PLACEMENT_3D('',#57117,#44477,#44478);
#36482=AXIS2_PLACEMENT_3D('',#57119,#44479,#44480);
#36483=AXIS2_PLACEMENT_3D('',#57121,#44482,#44483);
#36484=AXIS2_PLACEMENT_3D('',#57124,#44485,#44486);
#36485=AXIS2_PLACEMENT_3D('',#57125,#44487,#44488);
#36486=AXIS2_PLACEMENT_3D('',#57129,#44490,#44491);
#36487=AXIS2_PLACEMENT_3D('',#57131,#44493,#44494);
#36488=AXIS2_PLACEMENT_3D('',#57133,#44495,#44496);
#36489=AXIS2_PLACEMENT_3D('',#57135,#44498,#44499);
#36490=AXIS2_PLACEMENT_3D('',#57138,#44501,#44502);
#36491=AXIS2_PLACEMENT_3D('',#57139,#44503,#44504);
#36492=AXIS2_PLACEMENT_3D('',#57143,#44506,#44507);
#36493=AXIS2_PLACEMENT_3D('',#57145,#44509,#44510);
#36494=AXIS2_PLACEMENT_3D('',#57147,#44511,#44512);
#36495=AXIS2_PLACEMENT_3D('',#57149,#44514,#44515);
#36496=AXIS2_PLACEMENT_3D('',#57152,#44517,#44518);
#36497=AXIS2_PLACEMENT_3D('',#57153,#44519,#44520);
#36498=AXIS2_PLACEMENT_3D('',#57157,#44522,#44523);
#36499=AXIS2_PLACEMENT_3D('',#57159,#44525,#44526);
#36500=AXIS2_PLACEMENT_3D('',#57161,#44527,#44528);
#36501=AXIS2_PLACEMENT_3D('',#57163,#44530,#44531);
#36502=AXIS2_PLACEMENT_3D('',#57166,#44533,#44534);
#36503=AXIS2_PLACEMENT_3D('',#57167,#44535,#44536);
#36504=AXIS2_PLACEMENT_3D('',#57171,#44538,#44539);
#36505=AXIS2_PLACEMENT_3D('',#57173,#44541,#44542);
#36506=AXIS2_PLACEMENT_3D('',#57175,#44543,#44544);
#36507=AXIS2_PLACEMENT_3D('',#57177,#44546,#44547);
#36508=AXIS2_PLACEMENT_3D('',#57180,#44549,#44550);
#36509=AXIS2_PLACEMENT_3D('',#57181,#44551,#44552);
#36510=AXIS2_PLACEMENT_3D('',#57185,#44554,#44555);
#36511=AXIS2_PLACEMENT_3D('',#57187,#44557,#44558);
#36512=AXIS2_PLACEMENT_3D('',#57189,#44559,#44560);
#36513=AXIS2_PLACEMENT_3D('',#57191,#44562,#44563);
#36514=AXIS2_PLACEMENT_3D('',#57194,#44565,#44566);
#36515=AXIS2_PLACEMENT_3D('',#57195,#44567,#44568);
#36516=AXIS2_PLACEMENT_3D('',#57199,#44570,#44571);
#36517=AXIS2_PLACEMENT_3D('',#57201,#44573,#44574);
#36518=AXIS2_PLACEMENT_3D('',#57203,#44575,#44576);
#36519=AXIS2_PLACEMENT_3D('',#57205,#44578,#44579);
#36520=AXIS2_PLACEMENT_3D('',#57208,#44581,#44582);
#36521=AXIS2_PLACEMENT_3D('',#57209,#44583,#44584);
#36522=AXIS2_PLACEMENT_3D('',#57213,#44586,#44587);
#36523=AXIS2_PLACEMENT_3D('',#57215,#44589,#44590);
#36524=AXIS2_PLACEMENT_3D('',#57217,#44591,#44592);
#36525=AXIS2_PLACEMENT_3D('',#57219,#44594,#44595);
#36526=AXIS2_PLACEMENT_3D('',#57222,#44597,#44598);
#36527=AXIS2_PLACEMENT_3D('',#57223,#44599,#44600);
#36528=AXIS2_PLACEMENT_3D('',#57227,#44602,#44603);
#36529=AXIS2_PLACEMENT_3D('',#57229,#44605,#44606);
#36530=AXIS2_PLACEMENT_3D('',#57231,#44607,#44608);
#36531=AXIS2_PLACEMENT_3D('',#57233,#44610,#44611);
#36532=AXIS2_PLACEMENT_3D('',#57236,#44613,#44614);
#36533=AXIS2_PLACEMENT_3D('',#57237,#44615,#44616);
#36534=AXIS2_PLACEMENT_3D('',#57241,#44618,#44619);
#36535=AXIS2_PLACEMENT_3D('',#57243,#44621,#44622);
#36536=AXIS2_PLACEMENT_3D('',#57245,#44623,#44624);
#36537=AXIS2_PLACEMENT_3D('',#57247,#44626,#44627);
#36538=AXIS2_PLACEMENT_3D('',#57250,#44629,#44630);
#36539=AXIS2_PLACEMENT_3D('',#57251,#44631,#44632);
#36540=AXIS2_PLACEMENT_3D('',#57255,#44634,#44635);
#36541=AXIS2_PLACEMENT_3D('',#57257,#44637,#44638);
#36542=AXIS2_PLACEMENT_3D('',#57259,#44639,#44640);
#36543=AXIS2_PLACEMENT_3D('',#57261,#44642,#44643);
#36544=AXIS2_PLACEMENT_3D('',#57264,#44645,#44646);
#36545=AXIS2_PLACEMENT_3D('',#57265,#44647,#44648);
#36546=AXIS2_PLACEMENT_3D('',#57269,#44650,#44651);
#36547=AXIS2_PLACEMENT_3D('',#57271,#44653,#44654);
#36548=AXIS2_PLACEMENT_3D('',#57273,#44655,#44656);
#36549=AXIS2_PLACEMENT_3D('',#57275,#44658,#44659);
#36550=AXIS2_PLACEMENT_3D('',#57278,#44661,#44662);
#36551=AXIS2_PLACEMENT_3D('',#57279,#44663,#44664);
#36552=AXIS2_PLACEMENT_3D('',#57283,#44666,#44667);
#36553=AXIS2_PLACEMENT_3D('',#57285,#44669,#44670);
#36554=AXIS2_PLACEMENT_3D('',#57287,#44671,#44672);
#36555=AXIS2_PLACEMENT_3D('',#57289,#44674,#44675);
#36556=AXIS2_PLACEMENT_3D('',#57292,#44677,#44678);
#36557=AXIS2_PLACEMENT_3D('',#57293,#44679,#44680);
#36558=AXIS2_PLACEMENT_3D('',#57297,#44682,#44683);
#36559=AXIS2_PLACEMENT_3D('',#57299,#44685,#44686);
#36560=AXIS2_PLACEMENT_3D('',#57301,#44687,#44688);
#36561=AXIS2_PLACEMENT_3D('',#57303,#44690,#44691);
#36562=AXIS2_PLACEMENT_3D('',#57306,#44693,#44694);
#36563=AXIS2_PLACEMENT_3D('',#57307,#44695,#44696);
#36564=AXIS2_PLACEMENT_3D('',#57311,#44698,#44699);
#36565=AXIS2_PLACEMENT_3D('',#57313,#44701,#44702);
#36566=AXIS2_PLACEMENT_3D('',#57315,#44703,#44704);
#36567=AXIS2_PLACEMENT_3D('',#57317,#44706,#44707);
#36568=AXIS2_PLACEMENT_3D('',#57320,#44709,#44710);
#36569=AXIS2_PLACEMENT_3D('',#57321,#44711,#44712);
#36570=AXIS2_PLACEMENT_3D('',#57325,#44714,#44715);
#36571=AXIS2_PLACEMENT_3D('',#57327,#44717,#44718);
#36572=AXIS2_PLACEMENT_3D('',#57329,#44719,#44720);
#36573=AXIS2_PLACEMENT_3D('',#57331,#44722,#44723);
#36574=AXIS2_PLACEMENT_3D('',#57334,#44725,#44726);
#36575=AXIS2_PLACEMENT_3D('',#57335,#44727,#44728);
#36576=AXIS2_PLACEMENT_3D('',#57339,#44730,#44731);
#36577=AXIS2_PLACEMENT_3D('',#57341,#44733,#44734);
#36578=AXIS2_PLACEMENT_3D('',#57343,#44735,#44736);
#36579=AXIS2_PLACEMENT_3D('',#57345,#44738,#44739);
#36580=AXIS2_PLACEMENT_3D('',#57348,#44741,#44742);
#36581=AXIS2_PLACEMENT_3D('',#57349,#44743,#44744);
#36582=AXIS2_PLACEMENT_3D('',#57353,#44746,#44747);
#36583=AXIS2_PLACEMENT_3D('',#57355,#44749,#44750);
#36584=AXIS2_PLACEMENT_3D('',#57357,#44751,#44752);
#36585=AXIS2_PLACEMENT_3D('',#57359,#44754,#44755);
#36586=AXIS2_PLACEMENT_3D('',#57362,#44757,#44758);
#36587=AXIS2_PLACEMENT_3D('',#57363,#44759,#44760);
#36588=AXIS2_PLACEMENT_3D('',#57367,#44762,#44763);
#36589=AXIS2_PLACEMENT_3D('',#57369,#44765,#44766);
#36590=AXIS2_PLACEMENT_3D('',#57371,#44767,#44768);
#36591=AXIS2_PLACEMENT_3D('',#57373,#44770,#44771);
#36592=AXIS2_PLACEMENT_3D('',#57376,#44773,#44774);
#36593=AXIS2_PLACEMENT_3D('',#57377,#44775,#44776);
#36594=AXIS2_PLACEMENT_3D('',#57381,#44778,#44779);
#36595=AXIS2_PLACEMENT_3D('',#57383,#44781,#44782);
#36596=AXIS2_PLACEMENT_3D('',#57385,#44783,#44784);
#36597=AXIS2_PLACEMENT_3D('',#57387,#44786,#44787);
#36598=AXIS2_PLACEMENT_3D('',#57390,#44789,#44790);
#36599=AXIS2_PLACEMENT_3D('',#57391,#44791,#44792);
#36600=AXIS2_PLACEMENT_3D('',#57395,#44794,#44795);
#36601=AXIS2_PLACEMENT_3D('',#57397,#44797,#44798);
#36602=AXIS2_PLACEMENT_3D('',#57399,#44799,#44800);
#36603=AXIS2_PLACEMENT_3D('',#57401,#44802,#44803);
#36604=AXIS2_PLACEMENT_3D('',#57404,#44805,#44806);
#36605=AXIS2_PLACEMENT_3D('',#57405,#44807,#44808);
#36606=AXIS2_PLACEMENT_3D('',#57409,#44810,#44811);
#36607=AXIS2_PLACEMENT_3D('',#57411,#44813,#44814);
#36608=AXIS2_PLACEMENT_3D('',#57413,#44815,#44816);
#36609=AXIS2_PLACEMENT_3D('',#57415,#44818,#44819);
#36610=AXIS2_PLACEMENT_3D('',#57418,#44821,#44822);
#36611=AXIS2_PLACEMENT_3D('',#57419,#44823,#44824);
#36612=AXIS2_PLACEMENT_3D('',#57423,#44826,#44827);
#36613=AXIS2_PLACEMENT_3D('',#57425,#44829,#44830);
#36614=AXIS2_PLACEMENT_3D('',#57427,#44831,#44832);
#36615=AXIS2_PLACEMENT_3D('',#57429,#44834,#44835);
#36616=AXIS2_PLACEMENT_3D('',#57432,#44837,#44838);
#36617=AXIS2_PLACEMENT_3D('',#57433,#44839,#44840);
#36618=AXIS2_PLACEMENT_3D('',#57437,#44842,#44843);
#36619=AXIS2_PLACEMENT_3D('',#57439,#44845,#44846);
#36620=AXIS2_PLACEMENT_3D('',#57441,#44847,#44848);
#36621=AXIS2_PLACEMENT_3D('',#57443,#44850,#44851);
#36622=AXIS2_PLACEMENT_3D('',#57446,#44853,#44854);
#36623=AXIS2_PLACEMENT_3D('',#57447,#44855,#44856);
#36624=AXIS2_PLACEMENT_3D('',#57451,#44858,#44859);
#36625=AXIS2_PLACEMENT_3D('',#57453,#44861,#44862);
#36626=AXIS2_PLACEMENT_3D('',#57455,#44863,#44864);
#36627=AXIS2_PLACEMENT_3D('',#57457,#44866,#44867);
#36628=AXIS2_PLACEMENT_3D('',#57460,#44869,#44870);
#36629=AXIS2_PLACEMENT_3D('',#57461,#44871,#44872);
#36630=AXIS2_PLACEMENT_3D('',#57465,#44874,#44875);
#36631=AXIS2_PLACEMENT_3D('',#57467,#44877,#44878);
#36632=AXIS2_PLACEMENT_3D('',#57469,#44879,#44880);
#36633=AXIS2_PLACEMENT_3D('',#57471,#44882,#44883);
#36634=AXIS2_PLACEMENT_3D('',#57474,#44885,#44886);
#36635=AXIS2_PLACEMENT_3D('',#57475,#44887,#44888);
#36636=AXIS2_PLACEMENT_3D('',#57479,#44890,#44891);
#36637=AXIS2_PLACEMENT_3D('',#57481,#44893,#44894);
#36638=AXIS2_PLACEMENT_3D('',#57483,#44895,#44896);
#36639=AXIS2_PLACEMENT_3D('',#57485,#44898,#44899);
#36640=AXIS2_PLACEMENT_3D('',#57488,#44901,#44902);
#36641=AXIS2_PLACEMENT_3D('',#57489,#44903,#44904);
#36642=AXIS2_PLACEMENT_3D('',#57491,#44905,#44906);
#36643=AXIS2_PLACEMENT_3D('',#57493,#44908,#44909);
#36644=AXIS2_PLACEMENT_3D('',#57494,#44910,#44911);
#36645=AXIS2_PLACEMENT_3D('',#57495,#44912,#44913);
#36646=AXIS2_PLACEMENT_3D('',#57496,#44914,#44915);
#36647=AXIS2_PLACEMENT_3D('',#57497,#44916,#44917);
#36648=AXIS2_PLACEMENT_3D('',#57498,#44918,#44919);
#36649=AXIS2_PLACEMENT_3D('',#57499,#44920,#44921);
#36650=AXIS2_PLACEMENT_3D('',#57500,#44922,#44923);
#36651=AXIS2_PLACEMENT_3D('',#57501,#44924,#44925);
#36652=AXIS2_PLACEMENT_3D('',#57502,#44926,#44927);
#36653=AXIS2_PLACEMENT_3D('',#57503,#44928,#44929);
#36654=AXIS2_PLACEMENT_3D('',#57504,#44930,#44931);
#36655=AXIS2_PLACEMENT_3D('',#57505,#44932,#44933);
#36656=AXIS2_PLACEMENT_3D('',#57506,#44934,#44935);
#36657=AXIS2_PLACEMENT_3D('',#57507,#44936,#44937);
#36658=AXIS2_PLACEMENT_3D('',#57508,#44938,#44939);
#36659=AXIS2_PLACEMENT_3D('',#57509,#44940,#44941);
#36660=AXIS2_PLACEMENT_3D('',#57510,#44942,#44943);
#36661=AXIS2_PLACEMENT_3D('',#57511,#44944,#44945);
#36662=AXIS2_PLACEMENT_3D('',#57512,#44946,#44947);
#36663=AXIS2_PLACEMENT_3D('',#57513,#44948,#44949);
#36664=AXIS2_PLACEMENT_3D('',#57514,#44950,#44951);
#36665=AXIS2_PLACEMENT_3D('',#57515,#44952,#44953);
#36666=AXIS2_PLACEMENT_3D('',#57516,#44954,#44955);
#36667=AXIS2_PLACEMENT_3D('',#57517,#44956,#44957);
#36668=AXIS2_PLACEMENT_3D('',#57518,#44958,#44959);
#36669=AXIS2_PLACEMENT_3D('',#57519,#44960,#44961);
#36670=AXIS2_PLACEMENT_3D('',#57520,#44962,#44963);
#36671=AXIS2_PLACEMENT_3D('',#57521,#44964,#44965);
#36672=AXIS2_PLACEMENT_3D('',#57522,#44966,#44967);
#36673=AXIS2_PLACEMENT_3D('',#57523,#44968,#44969);
#36674=AXIS2_PLACEMENT_3D('',#57524,#44970,#44971);
#36675=AXIS2_PLACEMENT_3D('',#57525,#44972,#44973);
#36676=AXIS2_PLACEMENT_3D('',#57526,#44974,#44975);
#36677=AXIS2_PLACEMENT_3D('',#57527,#44976,#44977);
#36678=AXIS2_PLACEMENT_3D('',#57528,#44978,#44979);
#36679=AXIS2_PLACEMENT_3D('',#57529,#44980,#44981);
#36680=AXIS2_PLACEMENT_3D('',#57530,#44982,#44983);
#36681=AXIS2_PLACEMENT_3D('',#57531,#44984,#44985);
#36682=AXIS2_PLACEMENT_3D('',#57532,#44986,#44987);
#36683=AXIS2_PLACEMENT_3D('',#57533,#44988,#44989);
#36684=AXIS2_PLACEMENT_3D('',#57534,#44990,#44991);
#36685=AXIS2_PLACEMENT_3D('',#57535,#44992,#44993);
#36686=AXIS2_PLACEMENT_3D('',#57536,#44994,#44995);
#36687=AXIS2_PLACEMENT_3D('',#57537,#44996,#44997);
#36688=AXIS2_PLACEMENT_3D('',#57538,#44998,#44999);
#36689=AXIS2_PLACEMENT_3D('',#57539,#45000,#45001);
#36690=AXIS2_PLACEMENT_3D('',#57540,#45002,#45003);
#36691=AXIS2_PLACEMENT_3D('',#57541,#45004,#45005);
#36692=AXIS2_PLACEMENT_3D('',#57542,#45006,#45007);
#36693=AXIS2_PLACEMENT_3D('',#57543,#45008,#45009);
#36694=AXIS2_PLACEMENT_3D('',#57544,#45010,#45011);
#36695=AXIS2_PLACEMENT_3D('',#57545,#45012,#45013);
#36696=AXIS2_PLACEMENT_3D('',#57546,#45014,#45015);
#36697=AXIS2_PLACEMENT_3D('',#57547,#45016,#45017);
#36698=AXIS2_PLACEMENT_3D('',#57548,#45018,#45019);
#36699=AXIS2_PLACEMENT_3D('',#57549,#45020,#45021);
#36700=AXIS2_PLACEMENT_3D('',#57550,#45022,#45023);
#36701=AXIS2_PLACEMENT_3D('',#57551,#45024,#45025);
#36702=AXIS2_PLACEMENT_3D('',#57552,#45026,#45027);
#36703=AXIS2_PLACEMENT_3D('',#57553,#45028,#45029);
#36704=AXIS2_PLACEMENT_3D('',#57554,#45030,#45031);
#36705=AXIS2_PLACEMENT_3D('',#57555,#45032,#45033);
#36706=AXIS2_PLACEMENT_3D('',#57556,#45034,#45035);
#36707=AXIS2_PLACEMENT_3D('',#57557,#45036,#45037);
#36708=AXIS2_PLACEMENT_3D('',#57558,#45038,#45039);
#36709=AXIS2_PLACEMENT_3D('',#57559,#45040,#45041);
#36710=AXIS2_PLACEMENT_3D('',#57560,#45042,#45043);
#36711=AXIS2_PLACEMENT_3D('',#57561,#45044,#45045);
#36712=AXIS2_PLACEMENT_3D('',#57562,#45046,#45047);
#36713=AXIS2_PLACEMENT_3D('',#57563,#45048,#45049);
#36714=AXIS2_PLACEMENT_3D('',#57564,#45050,#45051);
#36715=AXIS2_PLACEMENT_3D('',#57565,#45052,#45053);
#36716=AXIS2_PLACEMENT_3D('',#57566,#45054,#45055);
#36717=AXIS2_PLACEMENT_3D('',#57567,#45056,#45057);
#36718=AXIS2_PLACEMENT_3D('',#57568,#45058,#45059);
#36719=AXIS2_PLACEMENT_3D('',#57569,#45060,#45061);
#36720=AXIS2_PLACEMENT_3D('',#57570,#45062,#45063);
#36721=AXIS2_PLACEMENT_3D('',#57571,#45064,#45065);
#36722=AXIS2_PLACEMENT_3D('',#57572,#45066,#45067);
#36723=AXIS2_PLACEMENT_3D('',#57573,#45068,#45069);
#36724=AXIS2_PLACEMENT_3D('',#57574,#45070,#45071);
#36725=AXIS2_PLACEMENT_3D('',#57575,#45072,#45073);
#36726=AXIS2_PLACEMENT_3D('',#57576,#45074,#45075);
#36727=AXIS2_PLACEMENT_3D('',#57577,#45076,#45077);
#36728=AXIS2_PLACEMENT_3D('',#57578,#45078,#45079);
#36729=AXIS2_PLACEMENT_3D('',#57579,#45080,#45081);
#36730=AXIS2_PLACEMENT_3D('',#57580,#45082,#45083);
#36731=AXIS2_PLACEMENT_3D('',#57581,#45084,#45085);
#36732=AXIS2_PLACEMENT_3D('',#57582,#45086,#45087);
#36733=AXIS2_PLACEMENT_3D('',#57583,#45088,#45089);
#36734=AXIS2_PLACEMENT_3D('',#57584,#45090,#45091);
#36735=AXIS2_PLACEMENT_3D('',#57585,#45092,#45093);
#36736=AXIS2_PLACEMENT_3D('',#57589,#45095,#45096);
#36737=AXIS2_PLACEMENT_3D('',#57591,#45098,#45099);
#36738=AXIS2_PLACEMENT_3D('',#57593,#45100,#45101);
#36739=AXIS2_PLACEMENT_3D('',#57595,#45103,#45104);
#36740=AXIS2_PLACEMENT_3D('',#57596,#45105,#45106);
#36741=AXIS2_PLACEMENT_3D('',#57597,#45107,#45108);
#36742=AXIS2_PLACEMENT_3D('',#57598,#45109,#45110);
#36743=AXIS2_PLACEMENT_3D('',#57599,#45111,#45112);
#36744=AXIS2_PLACEMENT_3D('',#57600,#45113,#45114);
#36745=AXIS2_PLACEMENT_3D('',#57601,#45115,#45116);
#36746=AXIS2_PLACEMENT_3D('',#57603,#45117,#45118);
#36747=AXIS2_PLACEMENT_3D('',#57605,#45119,#45120);
#36748=AXIS2_PLACEMENT_3D('',#57607,#45121,#45122);
#36749=AXIS2_PLACEMENT_3D('',#57608,#45123,#45124);
#36750=AXIS2_PLACEMENT_3D('',#57609,#45125,#45126);
#36751=AXIS2_PLACEMENT_3D('',#57612,#45128,#45129);
#36752=AXIS2_PLACEMENT_3D('',#57613,#45130,#45131);
#36753=AXIS2_PLACEMENT_3D('',#57621,#45135,#45136);
#36754=AXIS2_PLACEMENT_3D('',#57622,#45137,#45138);
#36755=AXIS2_PLACEMENT_3D('',#57624,#45139,#45140);
#36756=AXIS2_PLACEMENT_3D('',#57625,#45141,#45142);
#36757=AXIS2_PLACEMENT_3D('',#57626,#45143,#45144);
#36758=AXIS2_PLACEMENT_3D('',#57629,#45145,#45146);
#36759=AXIS2_PLACEMENT_3D('',#57631,#45147,#45148);
#36760=AXIS2_PLACEMENT_3D('',#57633,#45149,#45150);
#36761=AXIS2_PLACEMENT_3D('',#57635,#45151,#45152);
#36762=AXIS2_PLACEMENT_3D('',#57637,#45153,#45154);
#36763=AXIS2_PLACEMENT_3D('',#57639,#45155,#45156);
#36764=AXIS2_PLACEMENT_3D('',#57641,#45157,#45158);
#36765=AXIS2_PLACEMENT_3D('',#57643,#45159,#45160);
#36766=AXIS2_PLACEMENT_3D('',#57645,#45161,#45162);
#36767=AXIS2_PLACEMENT_3D('',#57647,#45163,#45164);
#36768=AXIS2_PLACEMENT_3D('',#57649,#45165,#45166);
#36769=AXIS2_PLACEMENT_3D('',#57651,#45167,#45168);
#36770=AXIS2_PLACEMENT_3D('',#57653,#45169,#45170);
#36771=AXIS2_PLACEMENT_3D('',#57655,#45171,#45172);
#36772=AXIS2_PLACEMENT_3D('',#57657,#45173,#45174);
#36773=AXIS2_PLACEMENT_3D('',#57659,#45175,#45176);
#36774=AXIS2_PLACEMENT_3D('',#57661,#45177,#45178);
#36775=AXIS2_PLACEMENT_3D('',#57663,#45179,#45180);
#36776=AXIS2_PLACEMENT_3D('',#57665,#45181,#45182);
#36777=AXIS2_PLACEMENT_3D('',#57667,#45183,#45184);
#36778=AXIS2_PLACEMENT_3D('',#57669,#45185,#45186);
#36779=AXIS2_PLACEMENT_3D('',#57671,#45187,#45188);
#36780=AXIS2_PLACEMENT_3D('',#57673,#45189,#45190);
#36781=AXIS2_PLACEMENT_3D('',#57675,#45191,#45192);
#36782=AXIS2_PLACEMENT_3D('',#57677,#45193,#45194);
#36783=AXIS2_PLACEMENT_3D('',#57679,#45195,#45196);
#36784=AXIS2_PLACEMENT_3D('',#57681,#45197,#45198);
#36785=AXIS2_PLACEMENT_3D('',#57683,#45199,#45200);
#36786=AXIS2_PLACEMENT_3D('',#57685,#45201,#45202);
#36787=AXIS2_PLACEMENT_3D('',#57687,#45203,#45204);
#36788=AXIS2_PLACEMENT_3D('',#57689,#45205,#45206);
#36789=AXIS2_PLACEMENT_3D('',#57691,#45207,#45208);
#36790=AXIS2_PLACEMENT_3D('',#57693,#45209,#45210);
#36791=AXIS2_PLACEMENT_3D('',#57695,#45211,#45212);
#36792=AXIS2_PLACEMENT_3D('',#57697,#45213,#45214);
#36793=AXIS2_PLACEMENT_3D('',#57699,#45215,#45216);
#36794=AXIS2_PLACEMENT_3D('',#57701,#45217,#45218);
#36795=AXIS2_PLACEMENT_3D('',#57703,#45219,#45220);
#36796=AXIS2_PLACEMENT_3D('',#57705,#45221,#45222);
#36797=AXIS2_PLACEMENT_3D('',#57707,#45223,#45224);
#36798=AXIS2_PLACEMENT_3D('',#57709,#45225,#45226);
#36799=AXIS2_PLACEMENT_3D('',#57711,#45227,#45228);
#36800=AXIS2_PLACEMENT_3D('',#57713,#45229,#45230);
#36801=AXIS2_PLACEMENT_3D('',#57715,#45231,#45232);
#36802=AXIS2_PLACEMENT_3D('',#57717,#45233,#45234);
#36803=AXIS2_PLACEMENT_3D('',#57719,#45235,#45236);
#36804=AXIS2_PLACEMENT_3D('',#57721,#45237,#45238);
#36805=AXIS2_PLACEMENT_3D('',#57723,#45239,#45240);
#36806=AXIS2_PLACEMENT_3D('',#57725,#45241,#45242);
#36807=AXIS2_PLACEMENT_3D('',#57727,#45243,#45244);
#36808=AXIS2_PLACEMENT_3D('',#57729,#45245,#45246);
#36809=AXIS2_PLACEMENT_3D('',#57731,#45247,#45248);
#36810=AXIS2_PLACEMENT_3D('',#57733,#45249,#45250);
#36811=AXIS2_PLACEMENT_3D('',#57735,#45251,#45252);
#36812=AXIS2_PLACEMENT_3D('',#57737,#45253,#45254);
#36813=AXIS2_PLACEMENT_3D('',#57739,#45255,#45256);
#36814=AXIS2_PLACEMENT_3D('',#57741,#45257,#45258);
#36815=AXIS2_PLACEMENT_3D('',#57743,#45259,#45260);
#36816=AXIS2_PLACEMENT_3D('',#57745,#45261,#45262);
#36817=AXIS2_PLACEMENT_3D('',#57747,#45263,#45264);
#36818=AXIS2_PLACEMENT_3D('',#57749,#45265,#45266);
#36819=AXIS2_PLACEMENT_3D('',#57751,#45267,#45268);
#36820=AXIS2_PLACEMENT_3D('',#57753,#45269,#45270);
#36821=AXIS2_PLACEMENT_3D('',#57755,#45271,#45272);
#36822=AXIS2_PLACEMENT_3D('',#57757,#45273,#45274);
#36823=AXIS2_PLACEMENT_3D('',#57759,#45275,#45276);
#36824=AXIS2_PLACEMENT_3D('',#57761,#45277,#45278);
#36825=AXIS2_PLACEMENT_3D('',#57763,#45279,#45280);
#36826=AXIS2_PLACEMENT_3D('',#57765,#45281,#45282);
#36827=AXIS2_PLACEMENT_3D('',#57767,#45283,#45284);
#36828=AXIS2_PLACEMENT_3D('',#57769,#45285,#45286);
#36829=AXIS2_PLACEMENT_3D('',#57771,#45287,#45288);
#36830=AXIS2_PLACEMENT_3D('',#57773,#45289,#45290);
#36831=AXIS2_PLACEMENT_3D('',#57775,#45291,#45292);
#36832=AXIS2_PLACEMENT_3D('',#57777,#45293,#45294);
#36833=AXIS2_PLACEMENT_3D('',#57779,#45295,#45296);
#36834=AXIS2_PLACEMENT_3D('',#57781,#45297,#45298);
#36835=AXIS2_PLACEMENT_3D('',#57783,#45299,#45300);
#36836=AXIS2_PLACEMENT_3D('',#57785,#45301,#45302);
#36837=AXIS2_PLACEMENT_3D('',#57787,#45303,#45304);
#36838=AXIS2_PLACEMENT_3D('',#57789,#45305,#45306);
#36839=AXIS2_PLACEMENT_3D('',#57791,#45307,#45308);
#36840=AXIS2_PLACEMENT_3D('',#57793,#45309,#45310);
#36841=AXIS2_PLACEMENT_3D('',#57795,#45311,#45312);
#36842=AXIS2_PLACEMENT_3D('',#57797,#45313,#45314);
#36843=AXIS2_PLACEMENT_3D('',#57799,#45315,#45316);
#36844=AXIS2_PLACEMENT_3D('',#57801,#45317,#45318);
#36845=AXIS2_PLACEMENT_3D('',#57803,#45319,#45320);
#36846=AXIS2_PLACEMENT_3D('',#57805,#45321,#45322);
#36847=AXIS2_PLACEMENT_3D('',#57807,#45323,#45324);
#36848=AXIS2_PLACEMENT_3D('',#57809,#45325,#45326);
#36849=AXIS2_PLACEMENT_3D('',#57811,#45327,#45328);
#36850=AXIS2_PLACEMENT_3D('',#57813,#45329,#45330);
#36851=AXIS2_PLACEMENT_3D('',#57815,#45331,#45332);
#36852=AXIS2_PLACEMENT_3D('',#57817,#45333,#45334);
#36853=AXIS2_PLACEMENT_3D('',#57819,#45335,#45336);
#36854=AXIS2_PLACEMENT_3D('',#57821,#45337,#45338);
#36855=AXIS2_PLACEMENT_3D('',#57823,#45339,#45340);
#36856=AXIS2_PLACEMENT_3D('',#57825,#45341,#45342);
#36857=AXIS2_PLACEMENT_3D('',#57827,#45343,#45344);
#36858=AXIS2_PLACEMENT_3D('',#57829,#45345,#45346);
#36859=AXIS2_PLACEMENT_3D('',#57831,#45347,#45348);
#36860=AXIS2_PLACEMENT_3D('',#57833,#45349,#45350);
#36861=AXIS2_PLACEMENT_3D('',#57835,#45351,#45352);
#36862=AXIS2_PLACEMENT_3D('',#57837,#45353,#45354);
#36863=AXIS2_PLACEMENT_3D('',#57839,#45355,#45356);
#36864=AXIS2_PLACEMENT_3D('',#57841,#45357,#45358);
#36865=AXIS2_PLACEMENT_3D('',#57843,#45359,#45360);
#36866=AXIS2_PLACEMENT_3D('',#57845,#45361,#45362);
#36867=AXIS2_PLACEMENT_3D('',#57847,#45363,#45364);
#36868=AXIS2_PLACEMENT_3D('',#57849,#45365,#45366);
#36869=AXIS2_PLACEMENT_3D('',#57851,#45367,#45368);
#36870=AXIS2_PLACEMENT_3D('',#57853,#45369,#45370);
#36871=AXIS2_PLACEMENT_3D('',#57855,#45371,#45372);
#36872=AXIS2_PLACEMENT_3D('',#57857,#45373,#45374);
#36873=AXIS2_PLACEMENT_3D('',#57859,#45375,#45376);
#36874=AXIS2_PLACEMENT_3D('',#57861,#45377,#45378);
#36875=AXIS2_PLACEMENT_3D('',#57863,#45379,#45380);
#36876=AXIS2_PLACEMENT_3D('',#57865,#45381,#45382);
#36877=AXIS2_PLACEMENT_3D('',#57867,#45383,#45384);
#36878=AXIS2_PLACEMENT_3D('',#57869,#45385,#45386);
#36879=AXIS2_PLACEMENT_3D('',#57871,#45387,#45388);
#36880=AXIS2_PLACEMENT_3D('',#57873,#45389,#45390);
#36881=AXIS2_PLACEMENT_3D('',#57875,#45391,#45392);
#36882=AXIS2_PLACEMENT_3D('',#57877,#45393,#45394);
#36883=AXIS2_PLACEMENT_3D('',#57879,#45395,#45396);
#36884=AXIS2_PLACEMENT_3D('',#57881,#45397,#45398);
#36885=AXIS2_PLACEMENT_3D('',#57883,#45399,#45400);
#36886=AXIS2_PLACEMENT_3D('',#57885,#45401,#45402);
#36887=AXIS2_PLACEMENT_3D('',#57887,#45403,#45404);
#36888=AXIS2_PLACEMENT_3D('',#57889,#45405,#45406);
#36889=AXIS2_PLACEMENT_3D('',#57891,#45407,#45408);
#36890=AXIS2_PLACEMENT_3D('',#57893,#45409,#45410);
#36891=AXIS2_PLACEMENT_3D('',#57895,#45411,#45412);
#36892=AXIS2_PLACEMENT_3D('',#57897,#45413,#45414);
#36893=AXIS2_PLACEMENT_3D('',#57899,#45415,#45416);
#36894=AXIS2_PLACEMENT_3D('',#57901,#45417,#45418);
#36895=AXIS2_PLACEMENT_3D('',#57903,#45419,#45420);
#36896=AXIS2_PLACEMENT_3D('',#57905,#45421,#45422);
#36897=AXIS2_PLACEMENT_3D('',#57907,#45423,#45424);
#36898=AXIS2_PLACEMENT_3D('',#57909,#45425,#45426);
#36899=AXIS2_PLACEMENT_3D('',#57911,#45427,#45428);
#36900=AXIS2_PLACEMENT_3D('',#57913,#45429,#45430);
#36901=AXIS2_PLACEMENT_3D('',#57915,#45431,#45432);
#36902=AXIS2_PLACEMENT_3D('',#57917,#45433,#45434);
#36903=AXIS2_PLACEMENT_3D('',#57919,#45435,#45436);
#36904=AXIS2_PLACEMENT_3D('',#57921,#45437,#45438);
#36905=AXIS2_PLACEMENT_3D('',#57923,#45439,#45440);
#36906=AXIS2_PLACEMENT_3D('',#57925,#45441,#45442);
#36907=AXIS2_PLACEMENT_3D('',#57927,#45443,#45444);
#36908=AXIS2_PLACEMENT_3D('',#57929,#45445,#45446);
#36909=AXIS2_PLACEMENT_3D('',#57931,#45447,#45448);
#36910=AXIS2_PLACEMENT_3D('',#57933,#45449,#45450);
#36911=AXIS2_PLACEMENT_3D('',#57935,#45451,#45452);
#36912=AXIS2_PLACEMENT_3D('',#57937,#45453,#45454);
#36913=AXIS2_PLACEMENT_3D('',#57939,#45455,#45456);
#36914=AXIS2_PLACEMENT_3D('',#57941,#45457,#45458);
#36915=AXIS2_PLACEMENT_3D('',#57943,#45459,#45460);
#36916=AXIS2_PLACEMENT_3D('',#57945,#45461,#45462);
#36917=AXIS2_PLACEMENT_3D('',#57946,#45463,#45464);
#36918=AXIS2_PLACEMENT_3D('',#57947,#45465,#45466);
#36919=AXIS2_PLACEMENT_3D('',#57953,#45470,#45471);
#36920=AXIS2_PLACEMENT_3D('',#57957,#45474,#45475);
#36921=AXIS2_PLACEMENT_3D('',#57959,#45476,#45477);
#36922=AXIS2_PLACEMENT_3D('',#57961,#45479,#45480);
#36923=AXIS2_PLACEMENT_3D('',#57963,#45482,#45483);
#36924=AXIS2_PLACEMENT_3D('',#57967,#45485,#45486);
#36925=AXIS2_PLACEMENT_3D('',#57969,#45488,#45489);
#36926=AXIS2_PLACEMENT_3D('',#57971,#45490,#45491);
#36927=AXIS2_PLACEMENT_3D('',#57973,#45493,#45494);
#36928=AXIS2_PLACEMENT_3D('',#57976,#45496,#45497);
#36929=AXIS2_PLACEMENT_3D('',#57977,#45498,#45499);
#36930=AXIS2_PLACEMENT_3D('',#57981,#45501,#45502);
#36931=AXIS2_PLACEMENT_3D('',#57983,#45504,#45505);
#36932=AXIS2_PLACEMENT_3D('',#57985,#45506,#45507);
#36933=AXIS2_PLACEMENT_3D('',#57987,#45509,#45510);
#36934=AXIS2_PLACEMENT_3D('',#57990,#45512,#45513);
#36935=AXIS2_PLACEMENT_3D('',#57991,#45514,#45515);
#36936=AXIS2_PLACEMENT_3D('',#57995,#45517,#45518);
#36937=AXIS2_PLACEMENT_3D('',#57997,#45520,#45521);
#36938=AXIS2_PLACEMENT_3D('',#57999,#45522,#45523);
#36939=AXIS2_PLACEMENT_3D('',#58001,#45525,#45526);
#36940=AXIS2_PLACEMENT_3D('',#58004,#45528,#45529);
#36941=AXIS2_PLACEMENT_3D('',#58005,#45530,#45531);
#36942=AXIS2_PLACEMENT_3D('',#58009,#45533,#45534);
#36943=AXIS2_PLACEMENT_3D('',#58011,#45536,#45537);
#36944=AXIS2_PLACEMENT_3D('',#58013,#45538,#45539);
#36945=AXIS2_PLACEMENT_3D('',#58015,#45541,#45542);
#36946=AXIS2_PLACEMENT_3D('',#58018,#45544,#45545);
#36947=AXIS2_PLACEMENT_3D('',#58019,#45546,#45547);
#36948=AXIS2_PLACEMENT_3D('',#58023,#45549,#45550);
#36949=AXIS2_PLACEMENT_3D('',#58025,#45552,#45553);
#36950=AXIS2_PLACEMENT_3D('',#58027,#45554,#45555);
#36951=AXIS2_PLACEMENT_3D('',#58029,#45557,#45558);
#36952=AXIS2_PLACEMENT_3D('',#58032,#45560,#45561);
#36953=AXIS2_PLACEMENT_3D('',#58033,#45562,#45563);
#36954=AXIS2_PLACEMENT_3D('',#58037,#45565,#45566);
#36955=AXIS2_PLACEMENT_3D('',#58039,#45568,#45569);
#36956=AXIS2_PLACEMENT_3D('',#58041,#45570,#45571);
#36957=AXIS2_PLACEMENT_3D('',#58043,#45573,#45574);
#36958=AXIS2_PLACEMENT_3D('',#58046,#45576,#45577);
#36959=AXIS2_PLACEMENT_3D('',#58047,#45578,#45579);
#36960=AXIS2_PLACEMENT_3D('',#58051,#45581,#45582);
#36961=AXIS2_PLACEMENT_3D('',#58053,#45584,#45585);
#36962=AXIS2_PLACEMENT_3D('',#58055,#45586,#45587);
#36963=AXIS2_PLACEMENT_3D('',#58057,#45589,#45590);
#36964=AXIS2_PLACEMENT_3D('',#58060,#45592,#45593);
#36965=AXIS2_PLACEMENT_3D('',#58061,#45594,#45595);
#36966=AXIS2_PLACEMENT_3D('',#58065,#45597,#45598);
#36967=AXIS2_PLACEMENT_3D('',#58067,#45600,#45601);
#36968=AXIS2_PLACEMENT_3D('',#58069,#45602,#45603);
#36969=AXIS2_PLACEMENT_3D('',#58071,#45605,#45606);
#36970=AXIS2_PLACEMENT_3D('',#58074,#45608,#45609);
#36971=AXIS2_PLACEMENT_3D('',#58075,#45610,#45611);
#36972=AXIS2_PLACEMENT_3D('',#58079,#45613,#45614);
#36973=AXIS2_PLACEMENT_3D('',#58081,#45616,#45617);
#36974=AXIS2_PLACEMENT_3D('',#58083,#45618,#45619);
#36975=AXIS2_PLACEMENT_3D('',#58085,#45621,#45622);
#36976=AXIS2_PLACEMENT_3D('',#58088,#45624,#45625);
#36977=AXIS2_PLACEMENT_3D('',#58089,#45626,#45627);
#36978=AXIS2_PLACEMENT_3D('',#58093,#45629,#45630);
#36979=AXIS2_PLACEMENT_3D('',#58095,#45632,#45633);
#36980=AXIS2_PLACEMENT_3D('',#58097,#45634,#45635);
#36981=AXIS2_PLACEMENT_3D('',#58099,#45637,#45638);
#36982=AXIS2_PLACEMENT_3D('',#58102,#45640,#45641);
#36983=AXIS2_PLACEMENT_3D('',#58103,#45642,#45643);
#36984=AXIS2_PLACEMENT_3D('',#58107,#45645,#45646);
#36985=AXIS2_PLACEMENT_3D('',#58109,#45648,#45649);
#36986=AXIS2_PLACEMENT_3D('',#58111,#45650,#45651);
#36987=AXIS2_PLACEMENT_3D('',#58113,#45653,#45654);
#36988=AXIS2_PLACEMENT_3D('',#58116,#45656,#45657);
#36989=AXIS2_PLACEMENT_3D('',#58117,#45658,#45659);
#36990=AXIS2_PLACEMENT_3D('',#58121,#45661,#45662);
#36991=AXIS2_PLACEMENT_3D('',#58123,#45664,#45665);
#36992=AXIS2_PLACEMENT_3D('',#58125,#45666,#45667);
#36993=AXIS2_PLACEMENT_3D('',#58127,#45669,#45670);
#36994=AXIS2_PLACEMENT_3D('',#58130,#45672,#45673);
#36995=AXIS2_PLACEMENT_3D('',#58131,#45674,#45675);
#36996=AXIS2_PLACEMENT_3D('',#58135,#45677,#45678);
#36997=AXIS2_PLACEMENT_3D('',#58137,#45680,#45681);
#36998=AXIS2_PLACEMENT_3D('',#58139,#45682,#45683);
#36999=AXIS2_PLACEMENT_3D('',#58141,#45685,#45686);
#37000=AXIS2_PLACEMENT_3D('',#58144,#45688,#45689);
#37001=AXIS2_PLACEMENT_3D('',#58145,#45690,#45691);
#37002=AXIS2_PLACEMENT_3D('',#58149,#45693,#45694);
#37003=AXIS2_PLACEMENT_3D('',#58151,#45696,#45697);
#37004=AXIS2_PLACEMENT_3D('',#58153,#45698,#45699);
#37005=AXIS2_PLACEMENT_3D('',#58155,#45701,#45702);
#37006=AXIS2_PLACEMENT_3D('',#58158,#45704,#45705);
#37007=AXIS2_PLACEMENT_3D('',#58159,#45706,#45707);
#37008=AXIS2_PLACEMENT_3D('',#58163,#45709,#45710);
#37009=AXIS2_PLACEMENT_3D('',#58165,#45712,#45713);
#37010=AXIS2_PLACEMENT_3D('',#58167,#45714,#45715);
#37011=AXIS2_PLACEMENT_3D('',#58169,#45717,#45718);
#37012=AXIS2_PLACEMENT_3D('',#58172,#45720,#45721);
#37013=AXIS2_PLACEMENT_3D('',#58173,#45722,#45723);
#37014=AXIS2_PLACEMENT_3D('',#58177,#45725,#45726);
#37015=AXIS2_PLACEMENT_3D('',#58179,#45728,#45729);
#37016=AXIS2_PLACEMENT_3D('',#58181,#45730,#45731);
#37017=AXIS2_PLACEMENT_3D('',#58183,#45733,#45734);
#37018=AXIS2_PLACEMENT_3D('',#58186,#45736,#45737);
#37019=AXIS2_PLACEMENT_3D('',#58187,#45738,#45739);
#37020=AXIS2_PLACEMENT_3D('',#58191,#45741,#45742);
#37021=AXIS2_PLACEMENT_3D('',#58193,#45744,#45745);
#37022=AXIS2_PLACEMENT_3D('',#58195,#45746,#45747);
#37023=AXIS2_PLACEMENT_3D('',#58197,#45749,#45750);
#37024=AXIS2_PLACEMENT_3D('',#58200,#45752,#45753);
#37025=AXIS2_PLACEMENT_3D('',#58201,#45754,#45755);
#37026=AXIS2_PLACEMENT_3D('',#58205,#45757,#45758);
#37027=AXIS2_PLACEMENT_3D('',#58207,#45760,#45761);
#37028=AXIS2_PLACEMENT_3D('',#58209,#45762,#45763);
#37029=AXIS2_PLACEMENT_3D('',#58211,#45765,#45766);
#37030=AXIS2_PLACEMENT_3D('',#58214,#45768,#45769);
#37031=AXIS2_PLACEMENT_3D('',#58215,#45770,#45771);
#37032=AXIS2_PLACEMENT_3D('',#58219,#45773,#45774);
#37033=AXIS2_PLACEMENT_3D('',#58221,#45776,#45777);
#37034=AXIS2_PLACEMENT_3D('',#58223,#45778,#45779);
#37035=AXIS2_PLACEMENT_3D('',#58225,#45781,#45782);
#37036=AXIS2_PLACEMENT_3D('',#58228,#45784,#45785);
#37037=AXIS2_PLACEMENT_3D('',#58229,#45786,#45787);
#37038=AXIS2_PLACEMENT_3D('',#58233,#45789,#45790);
#37039=AXIS2_PLACEMENT_3D('',#58235,#45792,#45793);
#37040=AXIS2_PLACEMENT_3D('',#58237,#45794,#45795);
#37041=AXIS2_PLACEMENT_3D('',#58239,#45797,#45798);
#37042=AXIS2_PLACEMENT_3D('',#58242,#45800,#45801);
#37043=AXIS2_PLACEMENT_3D('',#58243,#45802,#45803);
#37044=AXIS2_PLACEMENT_3D('',#58247,#45805,#45806);
#37045=AXIS2_PLACEMENT_3D('',#58249,#45808,#45809);
#37046=AXIS2_PLACEMENT_3D('',#58251,#45810,#45811);
#37047=AXIS2_PLACEMENT_3D('',#58253,#45813,#45814);
#37048=AXIS2_PLACEMENT_3D('',#58256,#45816,#45817);
#37049=AXIS2_PLACEMENT_3D('',#58257,#45818,#45819);
#37050=AXIS2_PLACEMENT_3D('',#58261,#45821,#45822);
#37051=AXIS2_PLACEMENT_3D('',#58263,#45824,#45825);
#37052=AXIS2_PLACEMENT_3D('',#58265,#45826,#45827);
#37053=AXIS2_PLACEMENT_3D('',#58267,#45829,#45830);
#37054=AXIS2_PLACEMENT_3D('',#58270,#45832,#45833);
#37055=AXIS2_PLACEMENT_3D('',#58271,#45834,#45835);
#37056=AXIS2_PLACEMENT_3D('',#58275,#45837,#45838);
#37057=AXIS2_PLACEMENT_3D('',#58277,#45840,#45841);
#37058=AXIS2_PLACEMENT_3D('',#58279,#45842,#45843);
#37059=AXIS2_PLACEMENT_3D('',#58281,#45845,#45846);
#37060=AXIS2_PLACEMENT_3D('',#58284,#45848,#45849);
#37061=AXIS2_PLACEMENT_3D('',#58285,#45850,#45851);
#37062=AXIS2_PLACEMENT_3D('',#58289,#45853,#45854);
#37063=AXIS2_PLACEMENT_3D('',#58291,#45856,#45857);
#37064=AXIS2_PLACEMENT_3D('',#58293,#45858,#45859);
#37065=AXIS2_PLACEMENT_3D('',#58295,#45861,#45862);
#37066=AXIS2_PLACEMENT_3D('',#58298,#45864,#45865);
#37067=AXIS2_PLACEMENT_3D('',#58299,#45866,#45867);
#37068=AXIS2_PLACEMENT_3D('',#58303,#45869,#45870);
#37069=AXIS2_PLACEMENT_3D('',#58305,#45872,#45873);
#37070=AXIS2_PLACEMENT_3D('',#58307,#45874,#45875);
#37071=AXIS2_PLACEMENT_3D('',#58309,#45877,#45878);
#37072=AXIS2_PLACEMENT_3D('',#58312,#45880,#45881);
#37073=AXIS2_PLACEMENT_3D('',#58313,#45882,#45883);
#37074=AXIS2_PLACEMENT_3D('',#58317,#45885,#45886);
#37075=AXIS2_PLACEMENT_3D('',#58319,#45888,#45889);
#37076=AXIS2_PLACEMENT_3D('',#58321,#45890,#45891);
#37077=AXIS2_PLACEMENT_3D('',#58323,#45893,#45894);
#37078=AXIS2_PLACEMENT_3D('',#58326,#45896,#45897);
#37079=AXIS2_PLACEMENT_3D('',#58327,#45898,#45899);
#37080=AXIS2_PLACEMENT_3D('',#58331,#45901,#45902);
#37081=AXIS2_PLACEMENT_3D('',#58333,#45904,#45905);
#37082=AXIS2_PLACEMENT_3D('',#58335,#45906,#45907);
#37083=AXIS2_PLACEMENT_3D('',#58337,#45909,#45910);
#37084=AXIS2_PLACEMENT_3D('',#58340,#45912,#45913);
#37085=AXIS2_PLACEMENT_3D('',#58341,#45914,#45915);
#37086=AXIS2_PLACEMENT_3D('',#58345,#45917,#45918);
#37087=AXIS2_PLACEMENT_3D('',#58347,#45920,#45921);
#37088=AXIS2_PLACEMENT_3D('',#58349,#45922,#45923);
#37089=AXIS2_PLACEMENT_3D('',#58351,#45925,#45926);
#37090=AXIS2_PLACEMENT_3D('',#58354,#45928,#45929);
#37091=AXIS2_PLACEMENT_3D('',#58355,#45930,#45931);
#37092=AXIS2_PLACEMENT_3D('',#58359,#45933,#45934);
#37093=AXIS2_PLACEMENT_3D('',#58361,#45936,#45937);
#37094=AXIS2_PLACEMENT_3D('',#58363,#45938,#45939);
#37095=AXIS2_PLACEMENT_3D('',#58365,#45941,#45942);
#37096=AXIS2_PLACEMENT_3D('',#58368,#45944,#45945);
#37097=AXIS2_PLACEMENT_3D('',#58369,#45946,#45947);
#37098=AXIS2_PLACEMENT_3D('',#58373,#45949,#45950);
#37099=AXIS2_PLACEMENT_3D('',#58375,#45952,#45953);
#37100=AXIS2_PLACEMENT_3D('',#58377,#45954,#45955);
#37101=AXIS2_PLACEMENT_3D('',#58379,#45957,#45958);
#37102=AXIS2_PLACEMENT_3D('',#58382,#45960,#45961);
#37103=AXIS2_PLACEMENT_3D('',#58383,#45962,#45963);
#37104=AXIS2_PLACEMENT_3D('',#58387,#45965,#45966);
#37105=AXIS2_PLACEMENT_3D('',#58389,#45968,#45969);
#37106=AXIS2_PLACEMENT_3D('',#58391,#45970,#45971);
#37107=AXIS2_PLACEMENT_3D('',#58393,#45973,#45974);
#37108=AXIS2_PLACEMENT_3D('',#58396,#45976,#45977);
#37109=AXIS2_PLACEMENT_3D('',#58397,#45978,#45979);
#37110=AXIS2_PLACEMENT_3D('',#58401,#45981,#45982);
#37111=AXIS2_PLACEMENT_3D('',#58403,#45984,#45985);
#37112=AXIS2_PLACEMENT_3D('',#58405,#45986,#45987);
#37113=AXIS2_PLACEMENT_3D('',#58407,#45989,#45990);
#37114=AXIS2_PLACEMENT_3D('',#58410,#45992,#45993);
#37115=AXIS2_PLACEMENT_3D('',#58411,#45994,#45995);
#37116=AXIS2_PLACEMENT_3D('',#58415,#45997,#45998);
#37117=AXIS2_PLACEMENT_3D('',#58417,#46000,#46001);
#37118=AXIS2_PLACEMENT_3D('',#58419,#46002,#46003);
#37119=AXIS2_PLACEMENT_3D('',#58421,#46005,#46006);
#37120=AXIS2_PLACEMENT_3D('',#58424,#46008,#46009);
#37121=AXIS2_PLACEMENT_3D('',#58425,#46010,#46011);
#37122=AXIS2_PLACEMENT_3D('',#58429,#46013,#46014);
#37123=AXIS2_PLACEMENT_3D('',#58431,#46016,#46017);
#37124=AXIS2_PLACEMENT_3D('',#58433,#46018,#46019);
#37125=AXIS2_PLACEMENT_3D('',#58435,#46021,#46022);
#37126=AXIS2_PLACEMENT_3D('',#58438,#46024,#46025);
#37127=AXIS2_PLACEMENT_3D('',#58439,#46026,#46027);
#37128=AXIS2_PLACEMENT_3D('',#58443,#46029,#46030);
#37129=AXIS2_PLACEMENT_3D('',#58445,#46032,#46033);
#37130=AXIS2_PLACEMENT_3D('',#58447,#46034,#46035);
#37131=AXIS2_PLACEMENT_3D('',#58449,#46037,#46038);
#37132=AXIS2_PLACEMENT_3D('',#58452,#46040,#46041);
#37133=AXIS2_PLACEMENT_3D('',#58453,#46042,#46043);
#37134=AXIS2_PLACEMENT_3D('',#58457,#46045,#46046);
#37135=AXIS2_PLACEMENT_3D('',#58459,#46048,#46049);
#37136=AXIS2_PLACEMENT_3D('',#58461,#46050,#46051);
#37137=AXIS2_PLACEMENT_3D('',#58463,#46053,#46054);
#37138=AXIS2_PLACEMENT_3D('',#58466,#46056,#46057);
#37139=AXIS2_PLACEMENT_3D('',#58467,#46058,#46059);
#37140=AXIS2_PLACEMENT_3D('',#58471,#46061,#46062);
#37141=AXIS2_PLACEMENT_3D('',#58473,#46064,#46065);
#37142=AXIS2_PLACEMENT_3D('',#58475,#46066,#46067);
#37143=AXIS2_PLACEMENT_3D('',#58477,#46069,#46070);
#37144=AXIS2_PLACEMENT_3D('',#58480,#46072,#46073);
#37145=AXIS2_PLACEMENT_3D('',#58481,#46074,#46075);
#37146=AXIS2_PLACEMENT_3D('',#58485,#46077,#46078);
#37147=AXIS2_PLACEMENT_3D('',#58487,#46080,#46081);
#37148=AXIS2_PLACEMENT_3D('',#58489,#46082,#46083);
#37149=AXIS2_PLACEMENT_3D('',#58491,#46085,#46086);
#37150=AXIS2_PLACEMENT_3D('',#58494,#46088,#46089);
#37151=AXIS2_PLACEMENT_3D('',#58495,#46090,#46091);
#37152=AXIS2_PLACEMENT_3D('',#58499,#46093,#46094);
#37153=AXIS2_PLACEMENT_3D('',#58501,#46096,#46097);
#37154=AXIS2_PLACEMENT_3D('',#58503,#46098,#46099);
#37155=AXIS2_PLACEMENT_3D('',#58505,#46101,#46102);
#37156=AXIS2_PLACEMENT_3D('',#58508,#46104,#46105);
#37157=AXIS2_PLACEMENT_3D('',#58509,#46106,#46107);
#37158=AXIS2_PLACEMENT_3D('',#58511,#46108,#46109);
#37159=AXIS2_PLACEMENT_3D('',#58513,#46111,#46112);
#37160=AXIS2_PLACEMENT_3D('',#58514,#46113,#46114);
#37161=AXIS2_PLACEMENT_3D('',#58515,#46115,#46116);
#37162=AXIS2_PLACEMENT_3D('',#58516,#46117,#46118);
#37163=AXIS2_PLACEMENT_3D('',#58517,#46119,#46120);
#37164=AXIS2_PLACEMENT_3D('',#58518,#46121,#46122);
#37165=AXIS2_PLACEMENT_3D('',#58519,#46123,#46124);
#37166=AXIS2_PLACEMENT_3D('',#58520,#46125,#46126);
#37167=AXIS2_PLACEMENT_3D('',#58521,#46127,#46128);
#37168=AXIS2_PLACEMENT_3D('',#58522,#46129,#46130);
#37169=AXIS2_PLACEMENT_3D('',#58523,#46131,#46132);
#37170=AXIS2_PLACEMENT_3D('',#58524,#46133,#46134);
#37171=AXIS2_PLACEMENT_3D('',#58525,#46135,#46136);
#37172=AXIS2_PLACEMENT_3D('',#58526,#46137,#46138);
#37173=AXIS2_PLACEMENT_3D('',#58527,#46139,#46140);
#37174=AXIS2_PLACEMENT_3D('',#58528,#46141,#46142);
#37175=AXIS2_PLACEMENT_3D('',#58529,#46143,#46144);
#37176=AXIS2_PLACEMENT_3D('',#58530,#46145,#46146);
#37177=AXIS2_PLACEMENT_3D('',#58531,#46147,#46148);
#37178=AXIS2_PLACEMENT_3D('',#58532,#46149,#46150);
#37179=AXIS2_PLACEMENT_3D('',#58533,#46151,#46152);
#37180=AXIS2_PLACEMENT_3D('',#58534,#46153,#46154);
#37181=AXIS2_PLACEMENT_3D('',#58535,#46155,#46156);
#37182=AXIS2_PLACEMENT_3D('',#58536,#46157,#46158);
#37183=AXIS2_PLACEMENT_3D('',#58537,#46159,#46160);
#37184=AXIS2_PLACEMENT_3D('',#58538,#46161,#46162);
#37185=AXIS2_PLACEMENT_3D('',#58539,#46163,#46164);
#37186=AXIS2_PLACEMENT_3D('',#58540,#46165,#46166);
#37187=AXIS2_PLACEMENT_3D('',#58541,#46167,#46168);
#37188=AXIS2_PLACEMENT_3D('',#58542,#46169,#46170);
#37189=AXIS2_PLACEMENT_3D('',#58543,#46171,#46172);
#37190=AXIS2_PLACEMENT_3D('',#58544,#46173,#46174);
#37191=AXIS2_PLACEMENT_3D('',#58545,#46175,#46176);
#37192=AXIS2_PLACEMENT_3D('',#58546,#46177,#46178);
#37193=AXIS2_PLACEMENT_3D('',#58547,#46179,#46180);
#37194=AXIS2_PLACEMENT_3D('',#58548,#46181,#46182);
#37195=AXIS2_PLACEMENT_3D('',#58549,#46183,#46184);
#37196=AXIS2_PLACEMENT_3D('',#58550,#46185,#46186);
#37197=AXIS2_PLACEMENT_3D('',#58551,#46187,#46188);
#37198=AXIS2_PLACEMENT_3D('',#58552,#46189,#46190);
#37199=AXIS2_PLACEMENT_3D('',#58553,#46191,#46192);
#37200=AXIS2_PLACEMENT_3D('',#58554,#46193,#46194);
#37201=AXIS2_PLACEMENT_3D('',#58555,#46195,#46196);
#37202=AXIS2_PLACEMENT_3D('',#58556,#46197,#46198);
#37203=AXIS2_PLACEMENT_3D('',#58557,#46199,#46200);
#37204=AXIS2_PLACEMENT_3D('',#58558,#46201,#46202);
#37205=AXIS2_PLACEMENT_3D('',#58559,#46203,#46204);
#37206=AXIS2_PLACEMENT_3D('',#58560,#46205,#46206);
#37207=AXIS2_PLACEMENT_3D('',#58561,#46207,#46208);
#37208=AXIS2_PLACEMENT_3D('',#58562,#46209,#46210);
#37209=AXIS2_PLACEMENT_3D('',#58563,#46211,#46212);
#37210=AXIS2_PLACEMENT_3D('',#58564,#46213,#46214);
#37211=AXIS2_PLACEMENT_3D('',#58565,#46215,#46216);
#37212=AXIS2_PLACEMENT_3D('',#58566,#46217,#46218);
#37213=AXIS2_PLACEMENT_3D('',#58567,#46219,#46220);
#37214=AXIS2_PLACEMENT_3D('',#58568,#46221,#46222);
#37215=AXIS2_PLACEMENT_3D('',#58569,#46223,#46224);
#37216=AXIS2_PLACEMENT_3D('',#58570,#46225,#46226);
#37217=AXIS2_PLACEMENT_3D('',#58571,#46227,#46228);
#37218=AXIS2_PLACEMENT_3D('',#58572,#46229,#46230);
#37219=AXIS2_PLACEMENT_3D('',#58573,#46231,#46232);
#37220=AXIS2_PLACEMENT_3D('',#58574,#46233,#46234);
#37221=AXIS2_PLACEMENT_3D('',#58575,#46235,#46236);
#37222=AXIS2_PLACEMENT_3D('',#58576,#46237,#46238);
#37223=AXIS2_PLACEMENT_3D('',#58577,#46239,#46240);
#37224=AXIS2_PLACEMENT_3D('',#58578,#46241,#46242);
#37225=AXIS2_PLACEMENT_3D('',#58579,#46243,#46244);
#37226=AXIS2_PLACEMENT_3D('',#58580,#46245,#46246);
#37227=AXIS2_PLACEMENT_3D('',#58581,#46247,#46248);
#37228=AXIS2_PLACEMENT_3D('',#58582,#46249,#46250);
#37229=AXIS2_PLACEMENT_3D('',#58583,#46251,#46252);
#37230=AXIS2_PLACEMENT_3D('',#58584,#46253,#46254);
#37231=AXIS2_PLACEMENT_3D('',#58585,#46255,#46256);
#37232=AXIS2_PLACEMENT_3D('',#58586,#46257,#46258);
#37233=AXIS2_PLACEMENT_3D('',#58587,#46259,#46260);
#37234=AXIS2_PLACEMENT_3D('',#58588,#46261,#46262);
#37235=AXIS2_PLACEMENT_3D('',#58589,#46263,#46264);
#37236=AXIS2_PLACEMENT_3D('',#58593,#46266,#46267);
#37237=AXIS2_PLACEMENT_3D('',#58595,#46269,#46270);
#37238=AXIS2_PLACEMENT_3D('',#58597,#46271,#46272);
#37239=AXIS2_PLACEMENT_3D('',#58599,#46274,#46275);
#37240=AXIS2_PLACEMENT_3D('',#58600,#46276,#46277);
#37241=AXIS2_PLACEMENT_3D('',#58601,#46278,#46279);
#37242=AXIS2_PLACEMENT_3D('',#58602,#46280,#46281);
#37243=AXIS2_PLACEMENT_3D('',#58603,#46282,#46283);
#37244=AXIS2_PLACEMENT_3D('',#58604,#46284,#46285);
#37245=AXIS2_PLACEMENT_3D('',#58605,#46286,#46287);
#37246=AXIS2_PLACEMENT_3D('',#58606,#46288,#46289);
#37247=AXIS2_PLACEMENT_3D('',#58607,#46290,#46291);
#37248=AXIS2_PLACEMENT_3D('',#58608,#46292,#46293);
#37249=AXIS2_PLACEMENT_3D('',#58611,#46294,#46295);
#37250=AXIS2_PLACEMENT_3D('',#58612,#46296,#46297);
#37251=AXIS2_PLACEMENT_3D('',#58615,#46299,#46300);
#37252=AXIS2_PLACEMENT_3D('',#58616,#46301,#46302);
#37253=AXIS2_PLACEMENT_3D('',#58617,#46303,#46304);
#37254=AXIS2_PLACEMENT_3D('',#58622,#46306,#46307);
#37255=AXIS2_PLACEMENT_3D('',#58623,#46308,#46309);
#37256=AXIS2_PLACEMENT_3D('',#58624,#46310,#46311);
#37257=AXIS2_PLACEMENT_3D('',#58626,#46313,#46314);
#37258=AXIS2_PLACEMENT_3D('',#58628,#46315,#46316);
#37259=AXIS2_PLACEMENT_3D('',#58631,#46318,#46319);
#37260=AXIS2_PLACEMENT_3D('',#58632,#46320,#46321);
#37261=AXIS2_PLACEMENT_3D('',#58634,#46322,#46323);
#37262=AXIS2_PLACEMENT_3D('',#58635,#46324,#46325);
#37263=AXIS2_PLACEMENT_3D('',#58637,#46326,#46327);
#37264=AXIS2_PLACEMENT_3D('',#58638,#46328,#46329);
#37265=AXIS2_PLACEMENT_3D('',#58640,#46331,#46332);
#37266=AXIS2_PLACEMENT_3D('',#58643,#46333,#46334);
#37267=AXIS2_PLACEMENT_3D('',#58644,#46335,#46336);
#37268=AXIS2_PLACEMENT_3D('',#58647,#46338,#46339);
#37269=AXIS2_PLACEMENT_3D('',#58648,#46340,#46341);
#37270=AXIS2_PLACEMENT_3D('',#58649,#46342,#46343);
#37271=AXIS2_PLACEMENT_3D('',#58654,#46345,#46346);
#37272=AXIS2_PLACEMENT_3D('',#58655,#46347,#46348);
#37273=AXIS2_PLACEMENT_3D('',#58656,#46349,#46350);
#37274=AXIS2_PLACEMENT_3D('',#58658,#46352,#46353);
#37275=AXIS2_PLACEMENT_3D('',#58660,#46354,#46355);
#37276=AXIS2_PLACEMENT_3D('',#58663,#46357,#46358);
#37277=AXIS2_PLACEMENT_3D('',#58664,#46359,#46360);
#37278=AXIS2_PLACEMENT_3D('',#58666,#46361,#46362);
#37279=AXIS2_PLACEMENT_3D('',#58667,#46363,#46364);
#37280=AXIS2_PLACEMENT_3D('',#58669,#46365,#46366);
#37281=AXIS2_PLACEMENT_3D('',#58670,#46367,#46368);
#37282=AXIS2_PLACEMENT_3D('',#58672,#46370,#46371);
#37283=AXIS2_PLACEMENT_3D('',#58675,#46372,#46373);
#37284=AXIS2_PLACEMENT_3D('',#58678,#46375,#46376);
#37285=AXIS2_PLACEMENT_3D('',#58679,#46377,#46378);
#37286=AXIS2_PLACEMENT_3D('',#58680,#46379,#46380);
#37287=AXIS2_PLACEMENT_3D('',#58681,#46381,#46382);
#37288=AXIS2_PLACEMENT_3D('',#58684,#46383,#46384);
#37289=AXIS2_PLACEMENT_3D('',#58685,#46385,#46386);
#37290=AXIS2_PLACEMENT_3D('',#58687,#46388,#46389);
#37291=AXIS2_PLACEMENT_3D('',#58690,#46391,#46392);
#37292=AXIS2_PLACEMENT_3D('',#58692,#46393,#46394);
#37293=AXIS2_PLACEMENT_3D('',#58695,#46396,#46397);
#37294=AXIS2_PLACEMENT_3D('',#58696,#46398,#46399);
#37295=AXIS2_PLACEMENT_3D('',#58698,#46400,#46401);
#37296=AXIS2_PLACEMENT_3D('',#58699,#46402,#46403);
#37297=AXIS2_PLACEMENT_3D('',#58701,#46404,#46405);
#37298=AXIS2_PLACEMENT_3D('',#58703,#46407,#46408);
#37299=AXIS2_PLACEMENT_3D('',#58704,#46409,#46410);
#37300=AXIS2_PLACEMENT_3D('',#58706,#46411,#46412);
#37301=AXIS2_PLACEMENT_3D('',#58709,#46414,#46415);
#37302=AXIS2_PLACEMENT_3D('',#58710,#46416,#46417);
#37303=AXIS2_PLACEMENT_3D('',#58712,#46418,#46419);
#37304=AXIS2_PLACEMENT_3D('',#58713,#46420,#46421);
#37305=AXIS2_PLACEMENT_3D('',#58716,#46423,#46424);
#37306=AXIS2_PLACEMENT_3D('',#58717,#46425,#46426);
#37307=AXIS2_PLACEMENT_3D('',#58718,#46427,#46428);
#37308=AXIS2_PLACEMENT_3D('',#58721,#46429,#46430);
#37309=AXIS2_PLACEMENT_3D('',#58722,#46431,#46432);
#37310=AXIS2_PLACEMENT_3D('',#58725,#46434,#46435);
#37311=AXIS2_PLACEMENT_3D('',#58726,#46436,#46437);
#37312=AXIS2_PLACEMENT_3D('',#58727,#46438,#46439);
#37313=AXIS2_PLACEMENT_3D('',#58730,#46440,#46441);
#37314=AXIS2_PLACEMENT_3D('',#58731,#46442,#46443);
#37315=AXIS2_PLACEMENT_3D('',#58733,#46445,#46446);
#37316=AXIS2_PLACEMENT_3D('',#58736,#46448,#46449);
#37317=AXIS2_PLACEMENT_3D('',#58738,#46450,#46451);
#37318=AXIS2_PLACEMENT_3D('',#58741,#46453,#46454);
#37319=AXIS2_PLACEMENT_3D('',#58742,#46455,#46456);
#37320=AXIS2_PLACEMENT_3D('',#58744,#46457,#46458);
#37321=AXIS2_PLACEMENT_3D('',#58745,#46459,#46460);
#37322=AXIS2_PLACEMENT_3D('',#58748,#46462,#46463);
#37323=AXIS2_PLACEMENT_3D('',#58749,#46464,#46465);
#37324=AXIS2_PLACEMENT_3D('',#58750,#46466,#46467);
#37325=AXIS2_PLACEMENT_3D('',#58753,#46468,#46469);
#37326=AXIS2_PLACEMENT_3D('',#58754,#46470,#46471);
#37327=AXIS2_PLACEMENT_3D('',#58757,#46473,#46474);
#37328=AXIS2_PLACEMENT_3D('',#58758,#46475,#46476);
#37329=AXIS2_PLACEMENT_3D('',#58759,#46477,#46478);
#37330=AXIS2_PLACEMENT_3D('',#58762,#46479,#46480);
#37331=AXIS2_PLACEMENT_3D('',#58763,#46481,#46482);
#37332=AXIS2_PLACEMENT_3D('',#58765,#46484,#46485);
#37333=AXIS2_PLACEMENT_3D('',#58768,#46487,#46488);
#37334=AXIS2_PLACEMENT_3D('',#58805,#46503,#46504);
#37335=AXIS2_PLACEMENT_3D('',#58808,#46505,#46506);
#37336=AXIS2_PLACEMENT_3D('',#58812,#46508,#46509);
#37337=AXIS2_PLACEMENT_3D('',#58814,#46511,#46512);
#37338=AXIS2_PLACEMENT_3D('',#58820,#46516,#46517);
#37339=AXIS2_PLACEMENT_3D('',#58823,#46518,#46519);
#37340=AXIS2_PLACEMENT_3D('',#58827,#46521,#46522);
#37341=AXIS2_PLACEMENT_3D('',#58829,#46524,#46525);
#37342=AXIS2_PLACEMENT_3D('',#58839,#46531,#46532);
#37343=AXIS2_PLACEMENT_3D('',#58846,#46537,#46538);
#37344=AXIS2_PLACEMENT_3D('',#58852,#46542,#46543);
#37345=AXIS2_PLACEMENT_3D('',#58853,#46544,#46545);
#37346=AXIS2_PLACEMENT_3D('',#58857,#46547,#46548);
#37347=AXIS2_PLACEMENT_3D('',#58865,#46553,#46554);
#37348=AXIS2_PLACEMENT_3D('',#58869,#46557,#46558);
#37349=AXIS2_PLACEMENT_3D('',#58871,#46559,#46560);
#37350=AXIS2_PLACEMENT_3D('',#58878,#46564,#46565);
#37351=AXIS2_PLACEMENT_3D('',#58880,#46566,#46567);
#37352=AXIS2_PLACEMENT_3D('',#58887,#46571,#46572);
#37353=AXIS2_PLACEMENT_3D('',#58889,#46573,#46574);
#37354=AXIS2_PLACEMENT_3D('',#58890,#46575,#46576);
#37355=AXIS2_PLACEMENT_3D('',#58892,#46577,#46578);
#37356=AXIS2_PLACEMENT_3D('',#58896,#46580,#46581);
#37357=AXIS2_PLACEMENT_3D('',#58897,#46582,#46583);
#37358=AXIS2_PLACEMENT_3D('',#58898,#46584,#46585);
#37359=AXIS2_PLACEMENT_3D('',#58899,#46586,#46587);
#37360=AXIS2_PLACEMENT_3D('',#58901,#46589,#46590);
#37361=AXIS2_PLACEMENT_3D('',#58914,#46597,#46598);
#37362=AXIS2_PLACEMENT_3D('',#58916,#46599,#46600);
#37363=AXIS2_PLACEMENT_3D('',#58918,#46601,#46602);
#37364=AXIS2_PLACEMENT_3D('',#58919,#46603,#46604);
#37365=AXIS2_PLACEMENT_3D('',#58923,#46606,#46607);
#37366=AXIS2_PLACEMENT_3D('',#58924,#46608,#46609);
#37367=AXIS2_PLACEMENT_3D('',#58925,#46610,#46611);
#37368=AXIS2_PLACEMENT_3D('',#58928,#46613,#46614);
#37369=AXIS2_PLACEMENT_3D('',#58929,#46615,#46616);
#37370=AXIS2_PLACEMENT_3D('',#58935,#46619,#46620);
#37371=AXIS2_PLACEMENT_3D('',#58939,#46622,#46623);
#37372=AXIS2_PLACEMENT_3D('',#58949,#46629,#46630);
#37373=AXIS2_PLACEMENT_3D('',#58953,#46632,#46633);
#37374=AXIS2_PLACEMENT_3D('',#58954,#46634,#46635);
#37375=AXIS2_PLACEMENT_3D('',#58955,#46636,#46637);
#37376=AXIS2_PLACEMENT_3D('',#58959,#46640,#46641);
#37377=AXIS2_PLACEMENT_3D('',#58963,#46644,#46645);
#37378=AXIS2_PLACEMENT_3D('',#58967,#46647,#46648);
#37379=AXIS2_PLACEMENT_3D('',#58968,#46649,#46650);
#37380=AXIS2_PLACEMENT_3D('',#58969,#46651,#46652);
#37381=AXIS2_PLACEMENT_3D('',#58977,#46657,#46658);
#37382=AXIS2_PLACEMENT_3D('',#58978,#46659,#46660);
#37383=AXIS2_PLACEMENT_3D('',#58979,#46661,#46662);
#37384=AXIS2_PLACEMENT_3D('',#58983,#46664,#46665);
#37385=AXIS2_PLACEMENT_3D('',#59007,#46675,#46676);
#37386=AXIS2_PLACEMENT_3D('',#59010,#46677,#46678);
#37387=AXIS2_PLACEMENT_3D('',#59014,#46680,#46681);
#37388=AXIS2_PLACEMENT_3D('',#59015,#46682,#46683);
#37389=AXIS2_PLACEMENT_3D('',#59017,#46684,#46685);
#37390=AXIS2_PLACEMENT_3D('',#59021,#46687,#46688);
#37391=AXIS2_PLACEMENT_3D('',#59023,#46689,#46690);
#37392=AXIS2_PLACEMENT_3D('',#59025,#46692,#46693);
#37393=AXIS2_PLACEMENT_3D('',#59028,#46694,#46695);
#37394=AXIS2_PLACEMENT_3D('',#59031,#46697,#46698);
#37395=AXIS2_PLACEMENT_3D('',#59033,#46699,#46700);
#37396=AXIS2_PLACEMENT_3D('',#59037,#46702,#46703);
#37397=AXIS2_PLACEMENT_3D('',#59039,#46704,#46705);
#37398=AXIS2_PLACEMENT_3D('',#59041,#46707,#46708);
#37399=AXIS2_PLACEMENT_3D('',#59045,#46711,#46712);
#37400=AXIS2_PLACEMENT_3D('',#59047,#46714,#46715);
#37401=AXIS2_PLACEMENT_3D('',#59056,#46720,#46721);
#37402=AXIS2_PLACEMENT_3D('',#59062,#46725,#46726);
#37403=AXIS2_PLACEMENT_3D('',#59068,#46730,#46731);
#37404=AXIS2_PLACEMENT_3D('',#59070,#46733,#46734);
#37405=AXIS2_PLACEMENT_3D('',#59076,#46735,#46736);
#37406=AXIS2_PLACEMENT_3D('',#59080,#46737,#46738);
#37407=AXIS2_PLACEMENT_3D('',#59083,#46740,#46741);
#37408=AXIS2_PLACEMENT_3D('',#59084,#46742,#46743);
#37409=AXIS2_PLACEMENT_3D('',#59087,#46744,#46745);
#37410=AXIS2_PLACEMENT_3D('',#59088,#46746,#46747);
#37411=AXIS2_PLACEMENT_3D('',#59091,#46749,#46750);
#37412=AXIS2_PLACEMENT_3D('',#59092,#46751,#46752);
#37413=AXIS2_PLACEMENT_3D('',#59095,#46753,#46754);
#37414=AXIS2_PLACEMENT_3D('',#59096,#46755,#46756);
#37415=AXIS2_PLACEMENT_3D('',#59099,#46758,#46759);
#37416=AXIS2_PLACEMENT_3D('',#59100,#46760,#46761);
#37417=AXIS2_PLACEMENT_3D('',#59103,#46762,#46763);
#37418=AXIS2_PLACEMENT_3D('',#59104,#46764,#46765);
#37419=AXIS2_PLACEMENT_3D('',#59107,#46767,#46768);
#37420=AXIS2_PLACEMENT_3D('',#59108,#46769,#46770);
#37421=AXIS2_PLACEMENT_3D('',#59111,#46771,#46772);
#37422=AXIS2_PLACEMENT_3D('',#59112,#46773,#46774);
#37423=AXIS2_PLACEMENT_3D('',#59115,#46776,#46777);
#37424=AXIS2_PLACEMENT_3D('',#59116,#46778,#46779);
#37425=AXIS2_PLACEMENT_3D('',#59117,#46780,#46781);
#37426=AXIS2_PLACEMENT_3D('',#59126,#46787,#46788);
#37427=AXIS2_PLACEMENT_3D('',#59133,#46793,#46794);
#37428=AXIS2_PLACEMENT_3D('',#59136,#46796,#46797);
#37429=AXIS2_PLACEMENT_3D('',#59137,#46798,#46799);
#37430=AXIS2_PLACEMENT_3D('',#59143,#46803,#46804);
#37431=AXIS2_PLACEMENT_3D('',#59150,#46807,#46808);
#37432=AXIS2_PLACEMENT_3D('',#59152,#46810,#46811);
#37433=AXIS2_PLACEMENT_3D('',#59154,#46812,#46813);
#37434=AXIS2_PLACEMENT_3D('',#59157,#46815,#46816);
#37435=AXIS2_PLACEMENT_3D('',#59158,#46817,#46818);
#37436=AXIS2_PLACEMENT_3D('',#59159,#46819,#46820);
#37437=AXIS2_PLACEMENT_3D('',#59176,#46825,#46826);
#37438=AXIS2_PLACEMENT_3D('',#59190,#46830,#46831);
#37439=AXIS2_PLACEMENT_3D('',#59204,#46835,#46836);
#37440=AXIS2_PLACEMENT_3D('',#59218,#46840,#46841);
#37441=AXIS2_PLACEMENT_3D('',#59223,#46842,#46843);
#37442=AXIS2_PLACEMENT_3D('',#59224,#46844,#46845);
#37443=AXIS2_PLACEMENT_3D('',#59225,#46846,#46847);
#37444=AXIS2_PLACEMENT_3D('',#59226,#46848,#46849);
#37445=AXIS2_PLACEMENT_3D('',#59236,#46850,#46851);
#37446=AXIS2_PLACEMENT_3D('',#59237,#46852,#46853);
#37447=AXIS2_PLACEMENT_3D('',#59242,#46854,#46855);
#37448=AXIS2_PLACEMENT_3D('',#59243,#46856,#46857);
#37449=AXIS2_PLACEMENT_3D('',#59244,#46858,#46859);
#37450=AXIS2_PLACEMENT_3D('',#59245,#46860,#46861);
#37451=AXIS2_PLACEMENT_3D('',#59250,#46865,#46866);
#37452=AXIS2_PLACEMENT_3D('',#59253,#46869,#46870);
#37453=AXIS2_PLACEMENT_3D('',#59254,#46871,#46872);
#37454=AXIS2_PLACEMENT_3D('',#59255,#46873,#46874);
#37455=AXIS2_PLACEMENT_3D('',#59256,#46875,#46876);
#37456=AXIS2_PLACEMENT_3D('',#59273,#46881,#46882);
#37457=AXIS2_PLACEMENT_3D('',#59287,#46886,#46887);
#37458=AXIS2_PLACEMENT_3D('',#59301,#46891,#46892);
#37459=AXIS2_PLACEMENT_3D('',#59315,#46896,#46897);
#37460=AXIS2_PLACEMENT_3D('',#59320,#46898,#46899);
#37461=AXIS2_PLACEMENT_3D('',#59321,#46900,#46901);
#37462=AXIS2_PLACEMENT_3D('',#59322,#46902,#46903);
#37463=AXIS2_PLACEMENT_3D('',#59323,#46904,#46905);
#37464=AXIS2_PLACEMENT_3D('',#59333,#46906,#46907);
#37465=AXIS2_PLACEMENT_3D('',#59334,#46908,#46909);
#37466=AXIS2_PLACEMENT_3D('',#59339,#46910,#46911);
#37467=AXIS2_PLACEMENT_3D('',#59340,#46912,#46913);
#37468=AXIS2_PLACEMENT_3D('',#59341,#46914,#46915);
#37469=AXIS2_PLACEMENT_3D('',#59342,#46916,#46917);
#37470=AXIS2_PLACEMENT_3D('',#59347,#46921,#46922);
#37471=AXIS2_PLACEMENT_3D('',#59350,#46925,#46926);
#37472=AXIS2_PLACEMENT_3D('',#59351,#46927,#46928);
#37473=AXIS2_PLACEMENT_3D('',#59352,#46929,#46930);
#37474=AXIS2_PLACEMENT_3D('',#59353,#46931,#46932);
#37475=AXIS2_PLACEMENT_3D('',#59357,#46935,#46936);
#37476=AXIS2_PLACEMENT_3D('',#59363,#46940,#46941);
#37477=AXIS2_PLACEMENT_3D('',#59367,#46944,#46945);
#37478=AXIS2_PLACEMENT_3D('',#59371,#46948,#46949);
#37479=AXIS2_PLACEMENT_3D('',#59375,#46952,#46953);
#37480=AXIS2_PLACEMENT_3D('',#59379,#46956,#46957);
#37481=AXIS2_PLACEMENT_3D('',#59381,#46959,#46960);
#37482=AXIS2_PLACEMENT_3D('',#59382,#46961,#46962);
#37483=AXIS2_PLACEMENT_3D('',#59384,#46964,#46965);
#37484=AXIS2_PLACEMENT_3D('',#59386,#46967,#46968);
#37485=AXIS2_PLACEMENT_3D('',#59387,#46969,#46970);
#37486=AXIS2_PLACEMENT_3D('',#59388,#46971,#46972);
#37487=AXIS2_PLACEMENT_3D('',#59389,#46973,#46974);
#37488=AXIS2_PLACEMENT_3D('',#59390,#46975,#46976);
#37489=AXIS2_PLACEMENT_3D('',#59391,#46977,#46978);
#37490=AXIS2_PLACEMENT_3D('',#59392,#46979,#46980);
#37491=AXIS2_PLACEMENT_3D('',#59405,#46987,#46988);
#37492=AXIS2_PLACEMENT_3D('',#59411,#46992,#46993);
#37493=AXIS2_PLACEMENT_3D('',#59415,#46996,#46997);
#37494=AXIS2_PLACEMENT_3D('',#59419,#47000,#47001);
#37495=AXIS2_PLACEMENT_3D('',#59423,#47004,#47005);
#37496=AXIS2_PLACEMENT_3D('',#59427,#47008,#47009);
#37497=AXIS2_PLACEMENT_3D('',#59429,#47011,#47012);
#37498=AXIS2_PLACEMENT_3D('',#59430,#47013,#47014);
#37499=AXIS2_PLACEMENT_3D('',#59431,#47015,#47016);
#37500=AXIS2_PLACEMENT_3D('',#59432,#47017,#47018);
#37501=AXIS2_PLACEMENT_3D('',#59445,#47025,#47026);
#37502=AXIS2_PLACEMENT_3D('',#59451,#47030,#47031);
#37503=AXIS2_PLACEMENT_3D('',#59455,#47034,#47035);
#37504=AXIS2_PLACEMENT_3D('',#59459,#47038,#47039);
#37505=AXIS2_PLACEMENT_3D('',#59463,#47042,#47043);
#37506=AXIS2_PLACEMENT_3D('',#59467,#47046,#47047);
#37507=AXIS2_PLACEMENT_3D('',#59469,#47049,#47050);
#37508=AXIS2_PLACEMENT_3D('',#59470,#47051,#47052);
#37509=AXIS2_PLACEMENT_3D('',#59471,#47053,#47054);
#37510=AXIS2_PLACEMENT_3D('',#59472,#47055,#47056);
#37511=AXIS2_PLACEMENT_3D('',#59476,#47059,#47060);
#37512=AXIS2_PLACEMENT_3D('',#59480,#47063,#47064);
#37513=AXIS2_PLACEMENT_3D('',#59482,#47066,#47067);
#37514=AXIS2_PLACEMENT_3D('',#59484,#47068,#47069);
#37515=AXIS2_PLACEMENT_3D('',#59485,#47070,#47071);
#37516=AXIS2_PLACEMENT_3D('',#59487,#47073,#47074);
#37517=AXIS2_PLACEMENT_3D('',#59492,#47076,#47077);
#37518=AXIS2_PLACEMENT_3D('',#59493,#47078,#47079);
#37519=AXIS2_PLACEMENT_3D('',#59494,#47080,#47081);
#37520=AXIS2_PLACEMENT_3D('',#59498,#47083,#47084);
#37521=AXIS2_PLACEMENT_3D('',#59499,#47085,#47086);
#37522=AXIS2_PLACEMENT_3D('',#59500,#47087,#47088);
#37523=AXIS2_PLACEMENT_3D('',#59503,#47090,#47091);
#37524=AXIS2_PLACEMENT_3D('',#59504,#47092,#47093);
#37525=AXIS2_PLACEMENT_3D('',#59509,#47095,#47096);
#37526=AXIS2_PLACEMENT_3D('',#59510,#47097,#47098);
#37527=AXIS2_PLACEMENT_3D('',#59511,#47099,#47100);
#37528=AXIS2_PLACEMENT_3D('',#59515,#47102,#47103);
#37529=AXIS2_PLACEMENT_3D('',#59516,#47104,#47105);
#37530=AXIS2_PLACEMENT_3D('',#59517,#47106,#47107);
#37531=AXIS2_PLACEMENT_3D('',#59520,#47109,#47110);
#37532=AXIS2_PLACEMENT_3D('',#59521,#47111,#47112);
#37533=AXIS2_PLACEMENT_3D('',#59526,#47114,#47115);
#37534=AXIS2_PLACEMENT_3D('',#59527,#47116,#47117);
#37535=AXIS2_PLACEMENT_3D('',#59528,#47118,#47119);
#37536=AXIS2_PLACEMENT_3D('',#59532,#47121,#47122);
#37537=AXIS2_PLACEMENT_3D('',#59533,#47123,#47124);
#37538=AXIS2_PLACEMENT_3D('',#59534,#47125,#47126);
#37539=AXIS2_PLACEMENT_3D('',#59537,#47128,#47129);
#37540=AXIS2_PLACEMENT_3D('',#59538,#47130,#47131);
#37541=AXIS2_PLACEMENT_3D('',#59541,#47132,#47133);
#37542=AXIS2_PLACEMENT_3D('',#59542,#47134,#47135);
#37543=AXIS2_PLACEMENT_3D('',#59545,#47137,#47138);
#37544=AXIS2_PLACEMENT_3D('',#59546,#47139,#47140);
#37545=AXIS2_PLACEMENT_3D('',#59550,#47142,#47143);
#37546=AXIS2_PLACEMENT_3D('',#59551,#47144,#47145);
#37547=AXIS2_PLACEMENT_3D('',#59552,#47146,#47147);
#37548=AXIS2_PLACEMENT_3D('',#59555,#47149,#47150);
#37549=AXIS2_PLACEMENT_3D('',#59558,#47151,#47152);
#37550=AXIS2_PLACEMENT_3D('',#59559,#47153,#47154);
#37551=AXIS2_PLACEMENT_3D('',#59562,#47156,#47157);
#37552=AXIS2_PLACEMENT_3D('',#59563,#47158,#47159);
#37553=AXIS2_PLACEMENT_3D('',#59567,#47161,#47162);
#37554=AXIS2_PLACEMENT_3D('',#59568,#47163,#47164);
#37555=AXIS2_PLACEMENT_3D('',#59569,#47165,#47166);
#37556=AXIS2_PLACEMENT_3D('',#59572,#47168,#47169);
#37557=AXIS2_PLACEMENT_3D('',#59575,#47170,#47171);
#37558=AXIS2_PLACEMENT_3D('',#59576,#47172,#47173);
#37559=AXIS2_PLACEMENT_3D('',#59579,#47175,#47176);
#37560=AXIS2_PLACEMENT_3D('',#59580,#47177,#47178);
#37561=AXIS2_PLACEMENT_3D('',#59584,#47180,#47181);
#37562=AXIS2_PLACEMENT_3D('',#59585,#47182,#47183);
#37563=AXIS2_PLACEMENT_3D('',#59586,#47184,#47185);
#37564=AXIS2_PLACEMENT_3D('',#59589,#47187,#47188);
#37565=AXIS2_PLACEMENT_3D('',#59592,#47189,#47190);
#37566=AXIS2_PLACEMENT_3D('',#59593,#47191,#47192);
#37567=AXIS2_PLACEMENT_3D('',#59596,#47194,#47195);
#37568=AXIS2_PLACEMENT_3D('',#59597,#47196,#47197);
#37569=AXIS2_PLACEMENT_3D('',#59601,#47199,#47200);
#37570=AXIS2_PLACEMENT_3D('',#59602,#47201,#47202);
#37571=AXIS2_PLACEMENT_3D('',#59603,#47203,#47204);
#37572=AXIS2_PLACEMENT_3D('',#59606,#47206,#47207);
#37573=AXIS2_PLACEMENT_3D('',#59609,#47209,#47210);
#37574=AXIS2_PLACEMENT_3D('',#59612,#47212,#47213);
#37575=AXIS2_PLACEMENT_3D('',#59615,#47215,#47216);
#37576=AXIS2_PLACEMENT_3D('',#59618,#47218,#47219);
#37577=AXIS2_PLACEMENT_3D('',#59621,#47221,#47222);
#37578=AXIS2_PLACEMENT_3D('',#59624,#47224,#47225);
#37579=AXIS2_PLACEMENT_3D('',#59627,#47227,#47228);
#37580=AXIS2_PLACEMENT_3D('',#59630,#47230,#47231);
#37581=AXIS2_PLACEMENT_3D('',#59636,#47235,#47236);
#37582=AXIS2_PLACEMENT_3D('',#59640,#47239,#47240);
#37583=AXIS2_PLACEMENT_3D('',#59646,#47244,#47245);
#37584=AXIS2_PLACEMENT_3D('',#59650,#47248,#47249);
#37585=AXIS2_PLACEMENT_3D('',#59654,#47252,#47253);
#37586=AXIS2_PLACEMENT_3D('',#59658,#47256,#47257);
#37587=AXIS2_PLACEMENT_3D('',#59662,#47260,#47261);
#37588=AXIS2_PLACEMENT_3D('',#59664,#47263,#47264);
#37589=AXIS2_PLACEMENT_3D('',#59684,#47275,#47276);
#37590=AXIS2_PLACEMENT_3D('',#59686,#47277,#47278);
#37591=AXIS2_PLACEMENT_3D('',#59688,#47279,#47280);
#37592=AXIS2_PLACEMENT_3D('',#59689,#47281,#47282);
#37593=AXIS2_PLACEMENT_3D('',#59692,#47284,#47285);
#37594=AXIS2_PLACEMENT_3D('',#59693,#47286,#47287);
#37595=AXIS2_PLACEMENT_3D('',#59696,#47288,#47289);
#37596=AXIS2_PLACEMENT_3D('',#59699,#47291,#47292);
#37597=AXIS2_PLACEMENT_3D('',#59700,#47293,#47294);
#37598=AXIS2_PLACEMENT_3D('',#59701,#47295,#47296);
#37599=AXIS2_PLACEMENT_3D('',#59702,#47297,#47298);
#37600=AXIS2_PLACEMENT_3D('',#59704,#47300,#47301);
#37601=AXIS2_PLACEMENT_3D('',#59708,#47304,#47305);
#37602=AXIS2_PLACEMENT_3D('',#59712,#47308,#47309);
#37603=AXIS2_PLACEMENT_3D('',#59716,#47312,#47313);
#37604=AXIS2_PLACEMENT_3D('',#59720,#47316,#47317);
#37605=AXIS2_PLACEMENT_3D('',#59724,#47320,#47321);
#37606=AXIS2_PLACEMENT_3D('',#59726,#47323,#47324);
#37607=AXIS2_PLACEMENT_3D('',#59727,#47325,#47326);
#37608=AXIS2_PLACEMENT_3D('',#59729,#47328,#47329);
#37609=AXIS2_PLACEMENT_3D('',#59730,#47330,#47331);
#37610=AXIS2_PLACEMENT_3D('',#59731,#47332,#47333);
#37611=AXIS2_PLACEMENT_3D('',#59734,#47334,#47335);
#37612=AXIS2_PLACEMENT_3D('',#59735,#47336,#47337);
#37613=AXIS2_PLACEMENT_3D('',#59738,#47339,#47340);
#37614=AXIS2_PLACEMENT_3D('',#59739,#47341,#47342);
#37615=AXIS2_PLACEMENT_3D('',#59819,#47344,#47345);
#37616=AXIS2_PLACEMENT_3D('',#59822,#47347,#47348);
#37617=AXIS2_PLACEMENT_3D('',#59823,#47349,#47350);
#37618=AXIS2_PLACEMENT_3D('',#59826,#47353,#47354);
#37619=AXIS2_PLACEMENT_3D('',#59827,#47355,#47356);
#37620=AXIS2_PLACEMENT_3D('',#59828,#47357,#47358);
#37621=AXIS2_PLACEMENT_3D('',#59830,#47359,#47360);
#37622=AXIS2_PLACEMENT_3D('',#59833,#47362,#47363);
#37623=AXIS2_PLACEMENT_3D('',#59834,#47364,#47365);
#37624=AXIS2_PLACEMENT_3D('',#59837,#47366,#47367);
#37625=AXIS2_PLACEMENT_3D('',#59838,#47368,#47369);
#37626=AXIS2_PLACEMENT_3D('',#59841,#47371,#47372);
#37627=AXIS2_PLACEMENT_3D('',#59842,#47373,#47374);
#37628=AXIS2_PLACEMENT_3D('',#59867,#47387,#47388);
#37629=AXIS2_PLACEMENT_3D('',#59869,#47389,#47390);
#37630=AXIS2_PLACEMENT_3D('',#59870,#47391,#47392);
#37631=AXIS2_PLACEMENT_3D('',#59872,#47393,#47394);
#37632=AXIS2_PLACEMENT_3D('',#59874,#47396,#47397);
#37633=AXIS2_PLACEMENT_3D('',#59875,#47398,#47399);
#37634=AXIS2_PLACEMENT_3D('',#59878,#47400,#47401);
#37635=AXIS2_PLACEMENT_3D('',#59879,#47402,#47403);
#37636=AXIS2_PLACEMENT_3D('',#59882,#47405,#47406);
#37637=AXIS2_PLACEMENT_3D('',#59883,#47407,#47408);
#37638=AXIS2_PLACEMENT_3D('',#59886,#47409,#47410);
#37639=AXIS2_PLACEMENT_3D('',#59887,#47411,#47412);
#37640=AXIS2_PLACEMENT_3D('',#59890,#47414,#47415);
#37641=AXIS2_PLACEMENT_3D('',#59891,#47416,#47417);
#37642=AXIS2_PLACEMENT_3D('',#59898,#47420,#47421);
#37643=AXIS2_PLACEMENT_3D('',#59900,#47423,#47424);
#37644=AXIS2_PLACEMENT_3D('',#59903,#47425,#47426);
#37645=AXIS2_PLACEMENT_3D('',#59912,#47427,#47428);
#37646=AXIS2_PLACEMENT_3D('',#59914,#47429,#47430);
#37647=AXIS2_PLACEMENT_3D('',#59915,#47431,#47432);
#37648=AXIS2_PLACEMENT_3D('',#59919,#47434,#47435);
#37649=AXIS2_PLACEMENT_3D('',#59991,#47437,#47438);
#37650=AXIS2_PLACEMENT_3D('',#59994,#47439,#47440);
#37651=AXIS2_PLACEMENT_3D('',#59995,#47441,#47442);
#37652=AXIS2_PLACEMENT_3D('',#59998,#47444,#47445);
#37653=AXIS2_PLACEMENT_3D('',#59999,#47446,#47447);
#37654=AXIS2_PLACEMENT_3D('',#60002,#47450,#47451);
#37655=AXIS2_PLACEMENT_3D('',#60015,#47458,#47459);
#37656=AXIS2_PLACEMENT_3D('',#60021,#47463,#47464);
#37657=AXIS2_PLACEMENT_3D('',#60025,#47467,#47468);
#37658=AXIS2_PLACEMENT_3D('',#60029,#47471,#47472);
#37659=AXIS2_PLACEMENT_3D('',#60033,#47475,#47476);
#37660=AXIS2_PLACEMENT_3D('',#60037,#47479,#47480);
#37661=AXIS2_PLACEMENT_3D('',#60039,#47482,#47483);
#37662=AXIS2_PLACEMENT_3D('',#60052,#47490,#47491);
#37663=AXIS2_PLACEMENT_3D('',#60058,#47495,#47496);
#37664=AXIS2_PLACEMENT_3D('',#60062,#47499,#47500);
#37665=AXIS2_PLACEMENT_3D('',#60066,#47503,#47504);
#37666=AXIS2_PLACEMENT_3D('',#60070,#47507,#47508);
#37667=AXIS2_PLACEMENT_3D('',#60074,#47511,#47512);
#37668=AXIS2_PLACEMENT_3D('',#60076,#47514,#47515);
#37669=AXIS2_PLACEMENT_3D('',#60078,#47516,#47517);
#37670=AXIS2_PLACEMENT_3D('',#60079,#47518,#47519);
#37671=AXIS2_PLACEMENT_3D('',#60082,#47520,#47521);
#37672=AXIS2_PLACEMENT_3D('',#60083,#47522,#47523);
#37673=AXIS2_PLACEMENT_3D('',#60085,#47525,#47526);
#37674=AXIS2_PLACEMENT_3D('',#60122,#47528,#47529);
#37675=AXIS2_PLACEMENT_3D('',#60125,#47530,#47531);
#37676=AXIS2_PLACEMENT_3D('',#60126,#47532,#47533);
#37677=AXIS2_PLACEMENT_3D('',#60129,#47535,#47536);
#37678=AXIS2_PLACEMENT_3D('',#60130,#47537,#47538);
#37679=AXIS2_PLACEMENT_3D('',#60131,#47539,#47540);
#37680=AXIS2_PLACEMENT_3D('',#60133,#47541,#47542);
#37681=AXIS2_PLACEMENT_3D('',#60134,#47543,#47544);
#37682=AXIS2_PLACEMENT_3D('',#60137,#47545,#47546);
#37683=AXIS2_PLACEMENT_3D('',#60138,#47547,#47548);
#37684=AXIS2_PLACEMENT_3D('',#60140,#47550,#47551);
#37685=AXIS2_PLACEMENT_3D('',#60153,#47558,#47559);
#37686=AXIS2_PLACEMENT_3D('',#60159,#47563,#47564);
#37687=AXIS2_PLACEMENT_3D('',#60163,#47567,#47568);
#37688=AXIS2_PLACEMENT_3D('',#60167,#47571,#47572);
#37689=AXIS2_PLACEMENT_3D('',#60171,#47575,#47576);
#37690=AXIS2_PLACEMENT_3D('',#60175,#47579,#47580);
#37691=AXIS2_PLACEMENT_3D('',#60177,#47582,#47583);
#37692=AXIS2_PLACEMENT_3D('',#60190,#47590,#47591);
#37693=AXIS2_PLACEMENT_3D('',#60196,#47595,#47596);
#37694=AXIS2_PLACEMENT_3D('',#60200,#47599,#47600);
#37695=AXIS2_PLACEMENT_3D('',#60204,#47603,#47604);
#37696=AXIS2_PLACEMENT_3D('',#60208,#47607,#47608);
#37697=AXIS2_PLACEMENT_3D('',#60212,#47611,#47612);
#37698=AXIS2_PLACEMENT_3D('',#60214,#47614,#47615);
#37699=AXIS2_PLACEMENT_3D('',#60216,#47616,#47617);
#37700=AXIS2_PLACEMENT_3D('',#60217,#47618,#47619);
#37701=AXIS2_PLACEMENT_3D('',#60220,#47620,#47621);
#37702=AXIS2_PLACEMENT_3D('',#60221,#47622,#47623);
#37703=AXIS2_PLACEMENT_3D('',#60223,#47625,#47626);
#37704=AXIS2_PLACEMENT_3D('',#60260,#47628,#47629);
#37705=AXIS2_PLACEMENT_3D('',#60263,#47630,#47631);
#37706=AXIS2_PLACEMENT_3D('',#60264,#47632,#47633);
#37707=AXIS2_PLACEMENT_3D('',#60267,#47635,#47636);
#37708=AXIS2_PLACEMENT_3D('',#60268,#47637,#47638);
#37709=AXIS2_PLACEMENT_3D('',#60269,#47639,#47640);
#37710=AXIS2_PLACEMENT_3D('',#60271,#47641,#47642);
#37711=AXIS2_PLACEMENT_3D('',#60272,#47643,#47644);
#37712=AXIS2_PLACEMENT_3D('',#60275,#47645,#47646);
#37713=AXIS2_PLACEMENT_3D('',#60276,#47647,#47648);
#37714=AXIS2_PLACEMENT_3D('',#60278,#47650,#47651);
#37715=AXIS2_PLACEMENT_3D('',#60315,#47653,#47654);
#37716=AXIS2_PLACEMENT_3D('',#60318,#47656,#47657);
#37717=AXIS2_PLACEMENT_3D('',#60319,#47658,#47659);
#37718=AXIS2_PLACEMENT_3D('',#60320,#47660,#47661);
#37719=AXIS2_PLACEMENT_3D('',#60322,#47663,#47664);
#37720=AXIS2_PLACEMENT_3D('',#60324,#47666,#47667);
#37721=AXIS2_PLACEMENT_3D('',#60326,#47668,#47669);
#37722=AXIS2_PLACEMENT_3D('',#60327,#47670,#47671);
#37723=AXIS2_PLACEMENT_3D('',#60329,#47673,#47674);
#37724=AXIS2_PLACEMENT_3D('',#60366,#47676,#47677);
#37725=AXIS2_PLACEMENT_3D('',#60369,#47678,#47679);
#37726=AXIS2_PLACEMENT_3D('',#60370,#47680,#47681);
#37727=AXIS2_PLACEMENT_3D('',#60373,#47683,#47684);
#37728=AXIS2_PLACEMENT_3D('',#60374,#47685,#47686);
#37729=AXIS2_PLACEMENT_3D('',#60376,#47688,#47689);
#37730=AXIS2_PLACEMENT_3D('',#60381,#47690,#47691);
#37731=AXIS2_PLACEMENT_3D('',#60386,#47692,#47693);
#37732=AXIS2_PLACEMENT_3D('',#60387,#47694,#47695);
#37733=AXIS2_PLACEMENT_3D('',#60389,#47696,#47697);
#37734=AXIS2_PLACEMENT_3D('',#60391,#47699,#47700);
#37735=AXIS2_PLACEMENT_3D('',#60393,#47701,#47702);
#37736=AXIS2_PLACEMENT_3D('',#60394,#47703,#47704);
#37737=AXIS2_PLACEMENT_3D('',#60396,#47705,#47706);
#37738=AXIS2_PLACEMENT_3D('',#60397,#47707,#47708);
#37739=AXIS2_PLACEMENT_3D('',#60399,#47710,#47711);
#37740=AXIS2_PLACEMENT_3D('',#60402,#47713,#47714);
#37741=AXIS2_PLACEMENT_3D('',#60403,#47715,#47716);
#37742=AXIS2_PLACEMENT_3D('',#60404,#47717,#47718);
#37743=AXIS2_PLACEMENT_3D('',#60406,#47719,#47720);
#37744=AXIS2_PLACEMENT_3D('',#60407,#47721,#47722);
#37745=AXIS2_PLACEMENT_3D('',#60409,#47724,#47725);
#37746=AXIS2_PLACEMENT_3D('',#60412,#47726,#47727);
#37747=AXIS2_PLACEMENT_3D('',#60416,#47729,#47730);
#37748=AXIS2_PLACEMENT_3D('',#60420,#47732,#47733);
#37749=AXIS2_PLACEMENT_3D('',#60424,#47735,#47736);
#37750=AXIS2_PLACEMENT_3D('',#60428,#47738,#47739);
#37751=AXIS2_PLACEMENT_3D('',#60432,#47741,#47742);
#37752=AXIS2_PLACEMENT_3D('',#60434,#47744,#47745);
#37753=AXIS2_PLACEMENT_3D('',#60442,#47746,#47747);
#37754=AXIS2_PLACEMENT_3D('',#60453,#47750,#47751);
#37755=AXIS2_PLACEMENT_3D('',#60462,#47753,#47754);
#37756=AXIS2_PLACEMENT_3D('',#60470,#47755,#47756);
#37757=AXIS2_PLACEMENT_3D('',#60474,#47757,#47758);
#37758=AXIS2_PLACEMENT_3D('',#60475,#47759,#47760);
#37759=AXIS2_PLACEMENT_3D('',#60483,#47761,#47762);
#37760=AXIS2_PLACEMENT_3D('',#60487,#47763,#47764);
#37761=AXIS2_PLACEMENT_3D('',#60489,#47766,#47767);
#37762=AXIS2_PLACEMENT_3D('',#60491,#47769,#47770);
#37763=AXIS2_PLACEMENT_3D('',#60493,#47772,#47773);
#37764=AXIS2_PLACEMENT_3D('',#60494,#47774,#47775);
#37765=AXIS2_PLACEMENT_3D('',#60497,#47776,#47777);
#37766=AXIS2_PLACEMENT_3D('',#60501,#47779,#47780);
#37767=AXIS2_PLACEMENT_3D('',#60505,#47782,#47783);
#37768=AXIS2_PLACEMENT_3D('',#60509,#47785,#47786);
#37769=AXIS2_PLACEMENT_3D('',#60513,#47788,#47789);
#37770=AXIS2_PLACEMENT_3D('',#60517,#47791,#47792);
#37771=AXIS2_PLACEMENT_3D('',#60519,#47794,#47795);
#37772=AXIS2_PLACEMENT_3D('',#60527,#47796,#47797);
#37773=AXIS2_PLACEMENT_3D('',#60538,#47800,#47801);
#37774=AXIS2_PLACEMENT_3D('',#60547,#47803,#47804);
#37775=AXIS2_PLACEMENT_3D('',#60555,#47805,#47806);
#37776=AXIS2_PLACEMENT_3D('',#60559,#47807,#47808);
#37777=AXIS2_PLACEMENT_3D('',#60560,#47809,#47810);
#37778=AXIS2_PLACEMENT_3D('',#60568,#47811,#47812);
#37779=AXIS2_PLACEMENT_3D('',#60572,#47813,#47814);
#37780=AXIS2_PLACEMENT_3D('',#60574,#47816,#47817);
#37781=AXIS2_PLACEMENT_3D('',#60576,#47819,#47820);
#37782=AXIS2_PLACEMENT_3D('',#60578,#47822,#47823);
#37783=AXIS2_PLACEMENT_3D('',#60579,#47824,#47825);
#37784=AXIS2_PLACEMENT_3D('',#60581,#47826,#47827);
#37785=AXIS2_PLACEMENT_3D('',#60582,#47828,#47829);
#37786=AXIS2_PLACEMENT_3D('',#60584,#47830,#47831);
#37787=AXIS2_PLACEMENT_3D('',#60585,#47832,#47833);
#37788=AXIS2_PLACEMENT_3D('',#60587,#47834,#47835);
#37789=AXIS2_PLACEMENT_3D('',#60588,#47836,#47837);
#37790=AXIS2_PLACEMENT_3D('',#60590,#47838,#47839);
#37791=AXIS2_PLACEMENT_3D('',#60593,#47841,#47842);
#37792=AXIS2_PLACEMENT_3D('',#60594,#47843,#47844);
#37793=AXIS2_PLACEMENT_3D('',#60596,#47845,#47846);
#37794=AXIS2_PLACEMENT_3D('',#60599,#47848,#47849);
#37795=AXIS2_PLACEMENT_3D('',#60600,#47850,#47851);
#37796=AXIS2_PLACEMENT_3D('',#60602,#47852,#47853);
#37797=AXIS2_PLACEMENT_3D('',#60604,#47855,#47856);
#37798=AXIS2_PLACEMENT_3D('',#60606,#47857,#47858);
#37799=AXIS2_PLACEMENT_3D('',#60609,#47860,#47861);
#37800=AXIS2_PLACEMENT_3D('',#60610,#47862,#47863);
#37801=AXIS2_PLACEMENT_3D('',#60612,#47864,#47865);
#37802=AXIS2_PLACEMENT_3D('',#60615,#47867,#47868);
#37803=AXIS2_PLACEMENT_3D('',#60616,#47869,#47870);
#37804=AXIS2_PLACEMENT_3D('',#60618,#47871,#47872);
#37805=AXIS2_PLACEMENT_3D('',#60621,#47874,#47875);
#37806=AXIS2_PLACEMENT_3D('',#60622,#47876,#47877);
#37807=AXIS2_PLACEMENT_3D('',#60624,#47878,#47879);
#37808=AXIS2_PLACEMENT_3D('',#60627,#47881,#47882);
#37809=AXIS2_PLACEMENT_3D('',#60628,#47883,#47884);
#37810=AXIS2_PLACEMENT_3D('',#60631,#47885,#47886);
#37811=AXIS2_PLACEMENT_3D('',#60633,#47887,#47888);
#37812=AXIS2_PLACEMENT_3D('',#60637,#47890,#47891);
#37813=AXIS2_PLACEMENT_3D('',#60639,#47892,#47893);
#37814=AXIS2_PLACEMENT_3D('',#60641,#47894,#47895);
#37815=AXIS2_PLACEMENT_3D('',#60644,#47897,#47898);
#37816=AXIS2_PLACEMENT_3D('',#60645,#47899,#47900);
#37817=AXIS2_PLACEMENT_3D('',#60654,#47905,#47906);
#37818=AXIS2_PLACEMENT_3D('',#60656,#47907,#47908);
#37819=AXIS2_PLACEMENT_3D('',#60659,#47910,#47911);
#37820=AXIS2_PLACEMENT_3D('',#60660,#47912,#47913);
#37821=AXIS2_PLACEMENT_3D('',#60662,#47914,#47915);
#37822=AXIS2_PLACEMENT_3D('',#60665,#47917,#47918);
#37823=AXIS2_PLACEMENT_3D('',#60666,#47919,#47920);
#37824=AXIS2_PLACEMENT_3D('',#60668,#47921,#47922);
#37825=AXIS2_PLACEMENT_3D('',#60671,#47924,#47925);
#37826=AXIS2_PLACEMENT_3D('',#60672,#47926,#47927);
#37827=AXIS2_PLACEMENT_3D('',#60678,#47931,#47932);
#37828=AXIS2_PLACEMENT_3D('',#60680,#47933,#47934);
#37829=AXIS2_PLACEMENT_3D('',#60683,#47936,#47937);
#37830=AXIS2_PLACEMENT_3D('',#60684,#47938,#47939);
#37831=AXIS2_PLACEMENT_3D('',#60686,#47940,#47941);
#37832=AXIS2_PLACEMENT_3D('',#60689,#47943,#47944);
#37833=AXIS2_PLACEMENT_3D('',#60690,#47945,#47946);
#37834=AXIS2_PLACEMENT_3D('',#60691,#47947,#47948);
#37835=AXIS2_PLACEMENT_3D('',#60692,#47949,#47950);
#37836=AXIS2_PLACEMENT_3D('',#60693,#47951,#47952);
#37837=AXIS2_PLACEMENT_3D('',#60694,#47953,#47954);
#37838=AXIS2_PLACEMENT_3D('',#60703,#47959,#47960);
#37839=AXIS2_PLACEMENT_3D('',#60705,#47961,#47962);
#37840=AXIS2_PLACEMENT_3D('',#60708,#47964,#47965);
#37841=AXIS2_PLACEMENT_3D('',#60709,#47966,#47967);
#37842=AXIS2_PLACEMENT_3D('',#60711,#47968,#47969);
#37843=AXIS2_PLACEMENT_3D('',#60714,#47971,#47972);
#37844=AXIS2_PLACEMENT_3D('',#60715,#47973,#47974);
#37845=AXIS2_PLACEMENT_3D('',#60717,#47975,#47976);
#37846=AXIS2_PLACEMENT_3D('',#60720,#47978,#47979);
#37847=AXIS2_PLACEMENT_3D('',#60721,#47980,#47981);
#37848=AXIS2_PLACEMENT_3D('',#60727,#47985,#47986);
#37849=AXIS2_PLACEMENT_3D('',#60729,#47987,#47988);
#37850=AXIS2_PLACEMENT_3D('',#60732,#47990,#47991);
#37851=AXIS2_PLACEMENT_3D('',#60733,#47992,#47993);
#37852=AXIS2_PLACEMENT_3D('',#60735,#47994,#47995);
#37853=AXIS2_PLACEMENT_3D('',#60738,#47997,#47998);
#37854=AXIS2_PLACEMENT_3D('',#60739,#47999,#48000);
#37855=AXIS2_PLACEMENT_3D('',#60740,#48001,#48002);
#37856=AXIS2_PLACEMENT_3D('',#60741,#48003,#48004);
#37857=AXIS2_PLACEMENT_3D('',#60742,#48005,#48006);
#37858=AXIS2_PLACEMENT_3D('',#60743,#48007,#48008);
#37859=AXIS2_PLACEMENT_3D('',#60752,#48013,#48014);
#37860=AXIS2_PLACEMENT_3D('',#60754,#48015,#48016);
#37861=AXIS2_PLACEMENT_3D('',#60757,#48018,#48019);
#37862=AXIS2_PLACEMENT_3D('',#60758,#48020,#48021);
#37863=AXIS2_PLACEMENT_3D('',#60760,#48022,#48023);
#37864=AXIS2_PLACEMENT_3D('',#60763,#48025,#48026);
#37865=AXIS2_PLACEMENT_3D('',#60764,#48027,#48028);
#37866=AXIS2_PLACEMENT_3D('',#60766,#48029,#48030);
#37867=AXIS2_PLACEMENT_3D('',#60769,#48032,#48033);
#37868=AXIS2_PLACEMENT_3D('',#60770,#48034,#48035);
#37869=AXIS2_PLACEMENT_3D('',#60776,#48039,#48040);
#37870=AXIS2_PLACEMENT_3D('',#60778,#48041,#48042);
#37871=AXIS2_PLACEMENT_3D('',#60781,#48044,#48045);
#37872=AXIS2_PLACEMENT_3D('',#60782,#48046,#48047);
#37873=AXIS2_PLACEMENT_3D('',#60784,#48048,#48049);
#37874=AXIS2_PLACEMENT_3D('',#60787,#48051,#48052);
#37875=AXIS2_PLACEMENT_3D('',#60788,#48053,#48054);
#37876=AXIS2_PLACEMENT_3D('',#60789,#48055,#48056);
#37877=AXIS2_PLACEMENT_3D('',#60790,#48057,#48058);
#37878=AXIS2_PLACEMENT_3D('',#60791,#48059,#48060);
#37879=AXIS2_PLACEMENT_3D('',#60792,#48061,#48062);
#37880=AXIS2_PLACEMENT_3D('',#60795,#48064,#48065);
#37881=AXIS2_PLACEMENT_3D('',#60796,#48066,#48067);
#37882=AXIS2_PLACEMENT_3D('',#60799,#48069,#48070);
#37883=AXIS2_PLACEMENT_3D('',#60800,#48071,#48072);
#37884=AXIS2_PLACEMENT_3D('',#60803,#48074,#48075);
#37885=AXIS2_PLACEMENT_3D('',#60804,#48076,#48077);
#37886=AXIS2_PLACEMENT_3D('',#60807,#48078,#48079);
#37887=AXIS2_PLACEMENT_3D('',#60809,#48080,#48081);
#37888=AXIS2_PLACEMENT_3D('',#60811,#48082,#48083);
#37889=AXIS2_PLACEMENT_3D('',#60812,#48084,#48085);
#37890=AXIS2_PLACEMENT_3D('',#60813,#48086,#48087);
#37891=AXIS2_PLACEMENT_3D('',#60815,#48089,#48090);
#37892=AXIS2_PLACEMENT_3D('',#60818,#48091,#48092);
#37893=AXIS2_PLACEMENT_3D('',#60820,#48093,#48094);
#37894=AXIS2_PLACEMENT_3D('',#60822,#48095,#48096);
#37895=AXIS2_PLACEMENT_3D('',#60823,#48097,#48098);
#37896=AXIS2_PLACEMENT_3D('',#60824,#48099,#48100);
#37897=AXIS2_PLACEMENT_3D('',#60826,#48102,#48103);
#37898=AXIS2_PLACEMENT_3D('',#60829,#48104,#48105);
#37899=AXIS2_PLACEMENT_3D('',#60831,#48106,#48107);
#37900=AXIS2_PLACEMENT_3D('',#60833,#48108,#48109);
#37901=AXIS2_PLACEMENT_3D('',#60834,#48110,#48111);
#37902=AXIS2_PLACEMENT_3D('',#60835,#48112,#48113);
#37903=AXIS2_PLACEMENT_3D('',#60837,#48115,#48116);
#37904=AXIS2_PLACEMENT_3D('',#60844,#48119,#48120);
#37905=AXIS2_PLACEMENT_3D('',#60849,#48123,#48124);
#37906=AXIS2_PLACEMENT_3D('',#60850,#48125,#48126);
#37907=AXIS2_PLACEMENT_3D('',#60855,#48128,#48129);
#37908=AXIS2_PLACEMENT_3D('',#60861,#48132,#48133);
#37909=AXIS2_PLACEMENT_3D('',#60863,#48135,#48136);
#37910=AXIS2_PLACEMENT_3D('',#60868,#48138,#48139);
#37911=AXIS2_PLACEMENT_3D('',#60874,#48142,#48143);
#37912=AXIS2_PLACEMENT_3D('',#60877,#48145,#48146);
#37913=AXIS2_PLACEMENT_3D('',#60878,#48147,#48148);
#37914=AXIS2_PLACEMENT_3D('',#60880,#48149,#48150);
#37915=AXIS2_PLACEMENT_3D('',#60884,#48152,#48153);
#37916=AXIS2_PLACEMENT_3D('',#60885,#48154,#48155);
#37917=AXIS2_PLACEMENT_3D('',#60886,#48156,#48157);
#37918=AXIS2_PLACEMENT_3D('',#60892,#48161,#48162);
#37919=AXIS2_PLACEMENT_3D('',#60898,#48166,#48167);
#37920=AXIS2_PLACEMENT_3D('',#60904,#48171,#48172);
#37921=AXIS2_PLACEMENT_3D('',#60910,#48176,#48177);
#37922=AXIS2_PLACEMENT_3D('',#60922,#48185,#48186);
#37923=AXIS2_PLACEMENT_3D('',#60925,#48188,#48189);
#37924=AXIS2_PLACEMENT_3D('',#60926,#48190,#48191);
#37925=AXIS2_PLACEMENT_3D('',#60936,#48198,#48199);
#37926=AXIS2_PLACEMENT_3D('',#60939,#48201,#48202);
#37927=AXIS2_PLACEMENT_3D('',#60940,#48203,#48204);
#37928=AXIS2_PLACEMENT_3D('',#60953,#48212,#48213);
#37929=AXIS2_PLACEMENT_3D('',#60955,#48214,#48215);
#37930=AXIS2_PLACEMENT_3D('',#60958,#48217,#48218);
#37931=AXIS2_PLACEMENT_3D('',#60959,#48219,#48220);
#37932=AXIS2_PLACEMENT_3D('',#60964,#48222,#48223);
#37933=AXIS2_PLACEMENT_3D('',#60968,#48225,#48226);
#37934=AXIS2_PLACEMENT_3D('',#60978,#48233,#48234);
#37935=AXIS2_PLACEMENT_3D('',#60979,#48235,#48236);
#37936=AXIS2_PLACEMENT_3D('',#60980,#48237,#48238);
#37937=AXIS2_PLACEMENT_3D('',#60986,#48241,#48242);
#37938=AXIS2_PLACEMENT_3D('',#60991,#48245,#48246);
#37939=AXIS2_PLACEMENT_3D('',#60996,#48249,#48250);
#37940=AXIS2_PLACEMENT_3D('',#61000,#48253,#48254);
#37941=AXIS2_PLACEMENT_3D('',#61001,#48255,#48256);
#37942=AXIS2_PLACEMENT_3D('',#61005,#48259,#48260);
#37943=AXIS2_PLACEMENT_3D('',#61007,#48261,#48262);
#37944=AXIS2_PLACEMENT_3D('',#61009,#48264,#48265);
#37945=AXIS2_PLACEMENT_3D('',#61011,#48267,#48268);
#37946=AXIS2_PLACEMENT_3D('',#61013,#48270,#48271);
#37947=AXIS2_PLACEMENT_3D('',#61015,#48273,#48274);
#37948=AXIS2_PLACEMENT_3D('',#61016,#48275,#48276);
#37949=AXIS2_PLACEMENT_3D('',#61018,#48278,#48279);
#37950=AXIS2_PLACEMENT_3D('',#61020,#48281,#48282);
#37951=AXIS2_PLACEMENT_3D('',#61021,#48283,#48284);
#37952=AXIS2_PLACEMENT_3D('',#61023,#48286,#48287);
#37953=AXIS2_PLACEMENT_3D('',#61025,#48289,#48290);
#37954=AXIS2_PLACEMENT_3D('',#61026,#48291,#48292);
#37955=AXIS2_PLACEMENT_3D('',#61027,#48293,#48294);
#37956=AXIS2_PLACEMENT_3D('',#61028,#48295,#48296);
#37957=AXIS2_PLACEMENT_3D('',#61029,#48297,#48298);
#37958=AXIS2_PLACEMENT_3D('',#61030,#48299,#48300);
#37959=AXIS2_PLACEMENT_3D('',#61031,#48301,#48302);
#37960=AXIS2_PLACEMENT_3D('',#61034,#48303,#48304);
#37961=AXIS2_PLACEMENT_3D('',#61038,#48306,#48307);
#37962=AXIS2_PLACEMENT_3D('',#61040,#48309,#48310);
#37963=AXIS2_PLACEMENT_3D('',#61046,#48314,#48315);
#37964=AXIS2_PLACEMENT_3D('',#61048,#48316,#48317);
#37965=AXIS2_PLACEMENT_3D('',#61051,#48319,#48320);
#37966=AXIS2_PLACEMENT_3D('',#61052,#48321,#48322);
#37967=AXIS2_PLACEMENT_3D('',#61054,#48323,#48324);
#37968=AXIS2_PLACEMENT_3D('',#61057,#48326,#48327);
#37969=AXIS2_PLACEMENT_3D('',#61058,#48328,#48329);
#37970=AXIS2_PLACEMENT_3D('',#61060,#48330,#48331);
#37971=AXIS2_PLACEMENT_3D('',#61063,#48333,#48334);
#37972=AXIS2_PLACEMENT_3D('',#61064,#48335,#48336);
#37973=AXIS2_PLACEMENT_3D('',#61070,#48340,#48341);
#37974=AXIS2_PLACEMENT_3D('',#61072,#48342,#48343);
#37975=AXIS2_PLACEMENT_3D('',#61075,#48345,#48346);
#37976=AXIS2_PLACEMENT_3D('',#61076,#48347,#48348);
#37977=AXIS2_PLACEMENT_3D('',#61077,#48349,#48350);
#37978=AXIS2_PLACEMENT_3D('',#61078,#48351,#48352);
#37979=AXIS2_PLACEMENT_3D('',#61079,#48353,#48354);
#37980=AXIS2_PLACEMENT_3D('',#61080,#48355,#48356);
#37981=AXIS2_PLACEMENT_3D('',#61089,#48361,#48362);
#37982=AXIS2_PLACEMENT_3D('',#61091,#48363,#48364);
#37983=AXIS2_PLACEMENT_3D('',#61094,#48366,#48367);
#37984=AXIS2_PLACEMENT_3D('',#61095,#48368,#48369);
#37985=AXIS2_PLACEMENT_3D('',#61097,#48370,#48371);
#37986=AXIS2_PLACEMENT_3D('',#61100,#48373,#48374);
#37987=AXIS2_PLACEMENT_3D('',#61101,#48375,#48376);
#37988=AXIS2_PLACEMENT_3D('',#61103,#48377,#48378);
#37989=AXIS2_PLACEMENT_3D('',#61106,#48380,#48381);
#37990=AXIS2_PLACEMENT_3D('',#61107,#48382,#48383);
#37991=AXIS2_PLACEMENT_3D('',#61113,#48387,#48388);
#37992=AXIS2_PLACEMENT_3D('',#61115,#48389,#48390);
#37993=AXIS2_PLACEMENT_3D('',#61118,#48392,#48393);
#37994=AXIS2_PLACEMENT_3D('',#61119,#48394,#48395);
#37995=AXIS2_PLACEMENT_3D('',#61121,#48396,#48397);
#37996=AXIS2_PLACEMENT_3D('',#61124,#48399,#48400);
#37997=AXIS2_PLACEMENT_3D('',#61125,#48401,#48402);
#37998=AXIS2_PLACEMENT_3D('',#61126,#48403,#48404);
#37999=AXIS2_PLACEMENT_3D('',#61127,#48405,#48406);
#38000=AXIS2_PLACEMENT_3D('',#61128,#48407,#48408);
#38001=AXIS2_PLACEMENT_3D('',#61129,#48409,#48410);
#38002=AXIS2_PLACEMENT_3D('',#61132,#48411,#48412);
#38003=AXIS2_PLACEMENT_3D('',#61136,#48414,#48415);
#38004=AXIS2_PLACEMENT_3D('',#61138,#48417,#48418);
#38005=AXIS2_PLACEMENT_3D('',#61140,#48419,#48420);
#38006=AXIS2_PLACEMENT_3D('',#61143,#48422,#48423);
#38007=AXIS2_PLACEMENT_3D('',#61144,#48424,#48425);
#38008=AXIS2_PLACEMENT_3D('',#61150,#48429,#48430);
#38009=AXIS2_PLACEMENT_3D('',#61152,#48431,#48432);
#38010=AXIS2_PLACEMENT_3D('',#61155,#48434,#48435);
#38011=AXIS2_PLACEMENT_3D('',#61156,#48436,#48437);
#38012=AXIS2_PLACEMENT_3D('',#61158,#48438,#48439);
#38013=AXIS2_PLACEMENT_3D('',#61161,#48441,#48442);
#38014=AXIS2_PLACEMENT_3D('',#61162,#48443,#48444);
#38015=AXIS2_PLACEMENT_3D('',#61164,#48445,#48446);
#38016=AXIS2_PLACEMENT_3D('',#61167,#48448,#48449);
#38017=AXIS2_PLACEMENT_3D('',#61168,#48450,#48451);
#38018=AXIS2_PLACEMENT_3D('',#61174,#48455,#48456);
#38019=AXIS2_PLACEMENT_3D('',#61175,#48457,#48458);
#38020=AXIS2_PLACEMENT_3D('',#61176,#48459,#48460);
#38021=AXIS2_PLACEMENT_3D('',#61177,#48461,#48462);
#38022=AXIS2_PLACEMENT_3D('',#61178,#48463,#48464);
#38023=AXIS2_PLACEMENT_3D('',#61181,#48465,#48466);
#38024=AXIS2_PLACEMENT_3D('',#61185,#48468,#48469);
#38025=AXIS2_PLACEMENT_3D('',#61187,#48471,#48472);
#38026=AXIS2_PLACEMENT_3D('',#61189,#48473,#48474);
#38027=AXIS2_PLACEMENT_3D('',#61192,#48476,#48477);
#38028=AXIS2_PLACEMENT_3D('',#61193,#48478,#48479);
#38029=AXIS2_PLACEMENT_3D('',#61199,#48483,#48484);
#38030=AXIS2_PLACEMENT_3D('',#61201,#48485,#48486);
#38031=AXIS2_PLACEMENT_3D('',#61204,#48488,#48489);
#38032=AXIS2_PLACEMENT_3D('',#61205,#48490,#48491);
#38033=AXIS2_PLACEMENT_3D('',#61207,#48492,#48493);
#38034=AXIS2_PLACEMENT_3D('',#61210,#48495,#48496);
#38035=AXIS2_PLACEMENT_3D('',#61211,#48497,#48498);
#38036=AXIS2_PLACEMENT_3D('',#61213,#48499,#48500);
#38037=AXIS2_PLACEMENT_3D('',#61216,#48502,#48503);
#38038=AXIS2_PLACEMENT_3D('',#61217,#48504,#48505);
#38039=AXIS2_PLACEMENT_3D('',#61223,#48509,#48510);
#38040=AXIS2_PLACEMENT_3D('',#61224,#48511,#48512);
#38041=AXIS2_PLACEMENT_3D('',#61225,#48513,#48514);
#38042=AXIS2_PLACEMENT_3D('',#61226,#48515,#48516);
#38043=AXIS2_PLACEMENT_3D('',#61227,#48517,#48518);
#38044=AXIS2_PLACEMENT_3D('',#61230,#48519,#48520);
#38045=AXIS2_PLACEMENT_3D('',#61233,#48523,#48524);
#38046=AXIS2_PLACEMENT_3D('',#61235,#48525,#48526);
#38047=AXIS2_PLACEMENT_3D('',#61237,#48528,#48529);
#38048=AXIS2_PLACEMENT_3D('',#61241,#48532,#48533);
#38049=AXIS2_PLACEMENT_3D('',#61243,#48534,#48535);
#38050=AXIS2_PLACEMENT_3D('',#61245,#48537,#48538);
#38051=AXIS2_PLACEMENT_3D('',#61247,#48539,#48540);
#38052=AXIS2_PLACEMENT_3D('',#61249,#48542,#48543);
#38053=AXIS2_PLACEMENT_3D('',#61251,#48544,#48545);
#38054=AXIS2_PLACEMENT_3D('',#61253,#48547,#48548);
#38055=AXIS2_PLACEMENT_3D('',#61255,#48549,#48550);
#38056=AXIS2_PLACEMENT_3D('',#61257,#48552,#48553);
#38057=AXIS2_PLACEMENT_3D('',#61259,#48555,#48556);
#38058=AXIS2_PLACEMENT_3D('',#61261,#48557,#48558);
#38059=AXIS2_PLACEMENT_3D('',#61262,#48559,#48560);
#38060=AXIS2_PLACEMENT_3D('',#61263,#48561,#48562);
#38061=AXIS2_PLACEMENT_3D('',#61280,#48571,#48572);
#38062=AXIS2_PLACEMENT_3D('',#61283,#48575,#48576);
#38063=AXIS2_PLACEMENT_3D('',#61286,#48579,#48580);
#38064=AXIS2_PLACEMENT_3D('',#61287,#48581,#48582);
#38065=AXIS2_PLACEMENT_3D('',#61290,#48585,#48586);
#38066=AXIS2_PLACEMENT_3D('',#61292,#48588,#48589);
#38067=AXIS2_PLACEMENT_3D('',#61293,#48590,#48591);
#38068=AXIS2_PLACEMENT_3D('',#61295,#48593,#48594);
#38069=AXIS2_PLACEMENT_3D('',#61296,#48595,#48596);
#38070=AXIS2_PLACEMENT_3D('',#61297,#48597,#48598);
#38071=AXIS2_PLACEMENT_3D('',#61298,#48599,#48600);
#38072=AXIS2_PLACEMENT_3D('',#61301,#48601,#48602);
#38073=AXIS2_PLACEMENT_3D('',#61302,#48603,#48604);
#38074=AXIS2_PLACEMENT_3D('',#61305,#48606,#48607);
#38075=AXIS2_PLACEMENT_3D('',#61306,#48608,#48609);
#38076=AXIS2_PLACEMENT_3D('',#61310,#48611,#48612);
#38077=AXIS2_PLACEMENT_3D('',#61311,#48613,#48614);
#38078=AXIS2_PLACEMENT_3D('',#61312,#48615,#48616);
#38079=AXIS2_PLACEMENT_3D('',#61314,#48618,#48619);
#38080=AXIS2_PLACEMENT_3D('',#61323,#48624,#48625);
#38081=AXIS2_PLACEMENT_3D('',#61329,#48629,#48630);
#38082=AXIS2_PLACEMENT_3D('',#61335,#48634,#48635);
#38083=AXIS2_PLACEMENT_3D('',#61341,#48639,#48640);
#38084=AXIS2_PLACEMENT_3D('',#61347,#48644,#48645);
#38085=AXIS2_PLACEMENT_3D('',#61349,#48647,#48648);
#38086=AXIS2_PLACEMENT_3D('',#61351,#48650,#48651);
#38087=AXIS2_PLACEMENT_3D('',#61352,#48652,#48653);
#38088=AXIS2_PLACEMENT_3D('',#61353,#48654,#48655);
#38089=AXIS2_PLACEMENT_3D('',#61355,#48656,#48657);
#38090=AXIS2_PLACEMENT_3D('',#61358,#48659,#48660);
#38091=AXIS2_PLACEMENT_3D('',#61429,#48661,#48662);
#38092=AXIS2_PLACEMENT_3D('',#61501,#48664,#48665);
#38093=AXIS2_PLACEMENT_3D('',#61573,#48667,#48668);
#38094=AXIS2_PLACEMENT_3D('',#61613,#48670,#48671);
#38095=AXIS2_PLACEMENT_3D('',#61653,#48673,#48674);
#38096=AXIS2_PLACEMENT_3D('',#61655,#48675,#48676);
#38097=AXIS2_PLACEMENT_3D('',#61656,#48677,#48678);
#38098=AXIS2_PLACEMENT_3D('',#61659,#48680,#48681);
#38099=AXIS2_PLACEMENT_3D('',#61660,#48682,#48683);
#38100=AXIS2_PLACEMENT_3D('',#61663,#48684,#48685);
#38101=AXIS2_PLACEMENT_3D('',#61664,#48686,#48687);
#38102=AXIS2_PLACEMENT_3D('',#61668,#48689,#48690);
#38103=AXIS2_PLACEMENT_3D('',#61669,#48691,#48692);
#38104=AXIS2_PLACEMENT_3D('',#61670,#48693,#48694);
#38105=AXIS2_PLACEMENT_3D('',#61673,#48696,#48697);
#38106=AXIS2_PLACEMENT_3D('',#61674,#48698,#48699);
#38107=AXIS2_PLACEMENT_3D('',#61675,#48700,#48701);
#38108=AXIS2_PLACEMENT_3D('',#61678,#48702,#48703);
#38109=AXIS2_PLACEMENT_3D('',#61679,#48704,#48705);
#38110=AXIS2_PLACEMENT_3D('',#61682,#48707,#48708);
#38111=AXIS2_PLACEMENT_3D('',#61683,#48709,#48710);
#38112=AXIS2_PLACEMENT_3D('',#61687,#48712,#48713);
#38113=AXIS2_PLACEMENT_3D('',#61688,#48714,#48715);
#38114=AXIS2_PLACEMENT_3D('',#61689,#48716,#48717);
#38115=AXIS2_PLACEMENT_3D('',#61690,#48718,#48719);
#38116=AXIS2_PLACEMENT_3D('',#61692,#48721,#48722);
#38117=AXIS2_PLACEMENT_3D('',#61693,#48723,#48724);
#38118=AXIS2_PLACEMENT_3D('',#61694,#48725,#48726);
#38119=AXIS2_PLACEMENT_3D('',#61695,#48727,#48728);
#38120=AXIS2_PLACEMENT_3D('',#61696,#48729,#48730);
#38121=AXIS2_PLACEMENT_3D('',#61697,#48731,#48732);
#38122=AXIS2_PLACEMENT_3D('',#61698,#48733,#48734);
#38123=AXIS2_PLACEMENT_3D('',#61699,#48735,#48736);
#38124=AXIS2_PLACEMENT_3D('',#61700,#48737,#48738);
#38125=AXIS2_PLACEMENT_3D('',#61701,#48739,#48740);
#38126=AXIS2_PLACEMENT_3D('',#61702,#48741,#48742);
#38127=AXIS2_PLACEMENT_3D('',#61703,#48743,#48744);
#38128=AXIS2_PLACEMENT_3D('',#61704,#48745,#48746);
#38129=AXIS2_PLACEMENT_3D('',#61705,#48747,#48748);
#38130=AXIS2_PLACEMENT_3D('',#61706,#48749,#48750);
#38131=AXIS2_PLACEMENT_3D('',#61707,#48751,#48752);
#38132=AXIS2_PLACEMENT_3D('',#61708,#48753,#48754);
#38133=AXIS2_PLACEMENT_3D('',#61709,#48755,#48756);
#38134=AXIS2_PLACEMENT_3D('',#61710,#48757,#48758);
#38135=AXIS2_PLACEMENT_3D('',#61711,#48759,#48760);
#38136=AXIS2_PLACEMENT_3D('',#61712,#48761,#48762);
#38137=AXIS2_PLACEMENT_3D('',#61713,#48763,#48764);
#38138=AXIS2_PLACEMENT_3D('',#61714,#48765,#48766);
#38139=AXIS2_PLACEMENT_3D('',#61715,#48767,#48768);
#38140=AXIS2_PLACEMENT_3D('',#61716,#48769,#48770);
#38141=AXIS2_PLACEMENT_3D('',#61717,#48771,#48772);
#38142=AXIS2_PLACEMENT_3D('',#61718,#48773,#48774);
#38143=AXIS2_PLACEMENT_3D('',#61719,#48775,#48776);
#38144=AXIS2_PLACEMENT_3D('',#61720,#48777,#48778);
#38145=AXIS2_PLACEMENT_3D('',#61721,#48779,#48780);
#38146=AXIS2_PLACEMENT_3D('',#61722,#48781,#48782);
#38147=AXIS2_PLACEMENT_3D('',#61723,#48783,#48784);
#38148=AXIS2_PLACEMENT_3D('',#61724,#48785,#48786);
#38149=AXIS2_PLACEMENT_3D('',#61725,#48787,#48788);
#38150=AXIS2_PLACEMENT_3D('',#61726,#48789,#48790);
#38151=AXIS2_PLACEMENT_3D('',#61727,#48791,#48792);
#38152=AXIS2_PLACEMENT_3D('',#61728,#48793,#48794);
#38153=AXIS2_PLACEMENT_3D('',#61729,#48795,#48796);
#38154=AXIS2_PLACEMENT_3D('',#61730,#48797,#48798);
#38155=AXIS2_PLACEMENT_3D('',#61731,#48799,#48800);
#38156=AXIS2_PLACEMENT_3D('',#61732,#48801,#48802);
#38157=AXIS2_PLACEMENT_3D('',#61733,#48803,#48804);
#38158=AXIS2_PLACEMENT_3D('',#61734,#48805,#48806);
#38159=AXIS2_PLACEMENT_3D('',#61735,#48807,#48808);
#38160=AXIS2_PLACEMENT_3D('',#61736,#48809,#48810);
#38161=AXIS2_PLACEMENT_3D('',#61737,#48811,#48812);
#38162=AXIS2_PLACEMENT_3D('',#61738,#48813,#48814);
#38163=AXIS2_PLACEMENT_3D('',#61739,#48815,#48816);
#38164=AXIS2_PLACEMENT_3D('',#61740,#48817,#48818);
#38165=AXIS2_PLACEMENT_3D('',#61741,#48819,#48820);
#38166=AXIS2_PLACEMENT_3D('',#61742,#48821,#48822);
#38167=AXIS2_PLACEMENT_3D('',#61743,#48823,#48824);
#38168=AXIS2_PLACEMENT_3D('',#61744,#48825,#48826);
#38169=AXIS2_PLACEMENT_3D('',#61745,#48827,#48828);
#38170=AXIS2_PLACEMENT_3D('',#61746,#48829,#48830);
#38171=AXIS2_PLACEMENT_3D('',#61747,#48831,#48832);
#38172=AXIS2_PLACEMENT_3D('',#61748,#48833,#48834);
#38173=AXIS2_PLACEMENT_3D('',#61749,#48835,#48836);
#38174=DIRECTION('axis',(0.,0.,1.));
#38175=DIRECTION('refdir',(1.,0.,0.));
#38176=DIRECTION('axis',(0.,0.,1.));
#38177=DIRECTION('refdir',(1.,0.,0.));
#38178=DIRECTION('center_axis',(0.996957691137886,-6.79465961587148E-16,
0.077944609056791));
#38179=DIRECTION('ref_axis',(0.077944609056791,2.83369376080442E-15,-0.996957691137886));
#38180=DIRECTION('',(-0.077944609056791,-2.83369376080442E-15,0.996957691137886));
#38181=DIRECTION('',(-4.56527663898138E-16,-1.,-2.87803349790671E-15));
#38182=DIRECTION('',(0.077944609056791,2.83369376080442E-15,-0.996957691137886));
#38183=DIRECTION('',(-4.56527663898138E-16,-1.,-2.87803349790671E-15));
#38184=DIRECTION('center_axis',(-0.996957691137886,6.79465961587148E-16,
-0.077944609056791));
#38185=DIRECTION('ref_axis',(-0.077944609056791,-2.83369376080442E-15,0.996957691137886));
#38186=DIRECTION('',(0.077944609056791,2.83369376080442E-15,-0.996957691137886));
#38187=DIRECTION('',(4.56527663898138E-16,1.,2.87803349790671E-15));
#38188=DIRECTION('',(-0.077944609056791,-2.83369376080442E-15,0.996957691137886));
#38189=DIRECTION('',(-4.56527663898138E-16,-1.,-2.87803349790671E-15));
#38190=DIRECTION('center_axis',(0.0779446090567893,2.83369376080442E-15,
-0.996957691137886));
#38191=DIRECTION('ref_axis',(-0.996957691137886,6.79465961587143E-16,-0.0779446090567894));
#38192=DIRECTION('',(0.996957691137886,-6.79465961587143E-16,0.0779446090567893));
#38193=DIRECTION('',(-0.996957691137886,6.79465961587143E-16,-0.0779446090567893));
#38194=DIRECTION('center_axis',(4.56527663898138E-16,1.,2.87803349790671E-15));
#38195=DIRECTION('ref_axis',(0.902362991552081,8.2841209666094E-16,-0.430976834037722));
#38196=DIRECTION('',(0.267735638451905,-2.89519216216193E-15,0.963492411959093));
#38197=DIRECTION('',(-0.0779446090567835,-2.83369376080443E-15,0.996957691137886));
#38198=DIRECTION('center_axis',(4.56527663898138E-16,1.,2.87803349790671E-15));
#38199=DIRECTION('ref_axis',(0.267735638451906,-2.89519216216193E-15,0.963492411959093));
#38200=DIRECTION('',(0.963492411959093,3.30691196032757E-16,-0.267735638451905));
#38201=DIRECTION('center_axis',(4.56527663898138E-16,1.,2.87803349790671E-15));
#38202=DIRECTION('ref_axis',(0.902362991552081,8.2841209666094E-16,-0.430976834037722));
#38203=DIRECTION('',(-0.968276724336069,1.16120910450874E-15,-0.249880341581751));
#38204=DIRECTION('',(-0.824418382495298,2.00528166414349E-15,-0.565980857100164));
#38205=DIRECTION('center_axis',(4.56527663898138E-16,1.,2.87803349790671E-15));
#38206=DIRECTION('ref_axis',(-0.968276724336069,1.16120910450873E-15,-0.24988034158175));
#38207=DIRECTION('',(-0.249880341581751,-2.67265555928621E-15,0.968276724336069));
#38208=DIRECTION('center_axis',(4.56527663898138E-16,1.,2.87803349790671E-15));
#38209=DIRECTION('ref_axis',(0.902362991552081,8.2841209666094E-16,-0.430976834037722));
#38210=DIRECTION('',(0.700541085884164,1.73398305765319E-15,-0.713612070377342));
#38211=DIRECTION('',(0.902362991552081,8.2841209666094E-16,-0.430976834037722));
#38212=DIRECTION('center_axis',(4.56527663898138E-16,1.,2.87803349790671E-15));
#38213=DIRECTION('ref_axis',(0.700541085884163,1.73398305765319E-15,-0.713612070377343));
#38214=DIRECTION('',(-0.713612070377342,2.34196436325345E-15,-0.700541085884164));
#38215=DIRECTION('center_axis',(4.56527663898138E-16,1.,2.87803349790671E-15));
#38216=DIRECTION('ref_axis',(0.902362991552081,8.2841209666094E-16,-0.430976834037722));
#38217=DIRECTION('center_axis',(4.56527663898138E-16,1.,2.87803349790671E-15));
#38218=DIRECTION('ref_axis',(-0.902362991552081,-8.2841209666094E-16,0.430976834037722));
#38219=DIRECTION('center_axis',(4.56527663898138E-16,1.,2.87803349790671E-15));
#38220=DIRECTION('ref_axis',(-0.0779446090567806,-2.83369376080443E-15,
0.996957691137887));
#38221=DIRECTION('center_axis',(-4.56527663898138E-16,-1.,-2.87803349790671E-15));
#38222=DIRECTION('ref_axis',(-0.902362991552081,-8.2841209666094E-16,0.430976834037722));
#38223=DIRECTION('center_axis',(0.267735638451905,-2.89519216216193E-15,
0.963492411959093));
#38224=DIRECTION('ref_axis',(0.963492411959093,3.30691196032758E-16,-0.267735638451905));
#38225=DIRECTION('',(4.56527663898138E-16,1.,2.87803349790671E-15));
#38226=DIRECTION('',(4.56527663898138E-16,1.,2.87803349790671E-15));
#38227=DIRECTION('',(-0.963492411959093,-3.30691196032757E-16,0.267735638451905));
#38228=DIRECTION('center_axis',(4.56527663898138E-16,1.,2.87803349790671E-15));
#38229=DIRECTION('ref_axis',(0.267735638451906,-2.89519216216193E-15,0.963492411959093));
#38230=DIRECTION('',(4.56527663898138E-16,1.,2.87803349790671E-15));
#38231=DIRECTION('center_axis',(-4.56527663898138E-16,-1.,-2.87803349790671E-15));
#38232=DIRECTION('ref_axis',(0.267735638451906,-2.89519216216193E-15,0.963492411959093));
#38233=DIRECTION('center_axis',(-0.996957691137886,6.79465961587129E-16,
-0.0779446090567844));
#38234=DIRECTION('ref_axis',(-0.0779446090567843,-2.83369376080442E-15,
0.996957691137886));
#38235=DIRECTION('',(4.56527663898138E-16,1.,2.87803349790671E-15));
#38236=DIRECTION('',(0.0779446090567835,2.83369376080443E-15,-0.996957691137886));
#38237=DIRECTION('center_axis',(-0.963492411959093,-3.30691196032757E-16,
0.267735638451905));
#38238=DIRECTION('ref_axis',(0.267735638451905,-2.89519216216193E-15,0.963492411959093));
#38239=DIRECTION('',(-4.56527663898138E-16,-1.,-2.87803349790671E-15));
#38240=DIRECTION('',(-0.267735638451905,2.89519216216193E-15,-0.963492411959093));
#38241=DIRECTION('center_axis',(-0.968276724336069,1.16120910450874E-15,
-0.249880341581751));
#38242=DIRECTION('ref_axis',(-0.24988034158175,-2.67265555928621E-15,0.968276724336069));
#38243=DIRECTION('',(4.56527663898138E-16,1.,2.87803349790671E-15));
#38244=DIRECTION('',(4.56527663898138E-16,1.,2.87803349790671E-15));
#38245=DIRECTION('',(0.249880341581751,2.67265555928621E-15,-0.968276724336069));
#38246=DIRECTION('center_axis',(4.56527663898138E-16,1.,2.87803349790671E-15));
#38247=DIRECTION('ref_axis',(-0.968276724336069,1.16120910450873E-15,-0.24988034158175));
#38248=DIRECTION('',(4.56527663898138E-16,1.,2.87803349790671E-15));
#38249=DIRECTION('center_axis',(-4.56527663898138E-16,-1.,-2.87803349790671E-15));
#38250=DIRECTION('ref_axis',(-0.968276724336069,1.16120910450873E-15,-0.24988034158175));
#38251=DIRECTION('center_axis',(0.565980857100164,2.11431780260853E-15,
-0.824418382495298));
#38252=DIRECTION('ref_axis',(-0.824418382495298,2.00528166414349E-15,-0.565980857100164));
#38253=DIRECTION('',(4.56527663898138E-16,1.,2.87803349790671E-15));
#38254=DIRECTION('',(0.824418382495298,-2.00528166414349E-15,0.565980857100164));
#38255=DIRECTION('center_axis',(0.249880341581751,2.67265555928621E-15,
-0.968276724336069));
#38256=DIRECTION('ref_axis',(-0.968276724336069,1.16120910450874E-15,-0.24988034158175));
#38257=DIRECTION('',(-4.56527663898138E-16,-1.,-2.87803349790671E-15));
#38258=DIRECTION('',(0.968276724336069,-1.16120910450874E-15,0.249880341581751));
#38259=DIRECTION('center_axis',(4.56527663898138E-16,1.,2.87803349790671E-15));
#38260=DIRECTION('ref_axis',(-0.910727040524933,-7.72881033974921E-16,0.413008786415856));
#38261=DIRECTION('center_axis',(4.56527663898138E-16,1.,2.87803349790671E-15));
#38262=DIRECTION('ref_axis',(0.902362991552081,8.2841209666094E-16,-0.430976834037722));
#38263=DIRECTION('',(-4.56527663898138E-16,-1.,-2.87803349790671E-15));
#38264=DIRECTION('center_axis',(4.56527663898138E-16,1.,2.87803349790671E-15));
#38265=DIRECTION('ref_axis',(0.902362991552081,8.2841209666094E-16,-0.430976834037722));
#38266=DIRECTION('center_axis',(4.56527663898138E-16,1.,2.87803349790671E-15));
#38267=DIRECTION('ref_axis',(0.902362991552081,8.2841209666094E-16,-0.430976834037722));
#38268=DIRECTION('center_axis',(4.56527663898138E-16,1.,2.87803349790671E-15));
#38269=DIRECTION('ref_axis',(0.700541085884163,1.73398305765319E-15,-0.713612070377343));
#38270=DIRECTION('',(4.56527663898138E-16,1.,2.87803349790671E-15));
#38271=DIRECTION('center_axis',(-4.56527663898138E-16,-1.,-2.87803349790671E-15));
#38272=DIRECTION('ref_axis',(0.700541085884163,1.73398305765319E-15,-0.713612070377343));
#38273=DIRECTION('',(4.56527663898138E-16,1.,2.87803349790671E-15));
#38274=DIRECTION('center_axis',(0.430976834037722,-2.79378376419566E-15,
0.902362991552081));
#38275=DIRECTION('ref_axis',(0.902362991552081,8.2841209666094E-16,-0.430976834037722));
#38276=DIRECTION('',(4.56527663898138E-16,1.,2.87803349790671E-15));
#38277=DIRECTION('',(-0.902362991552081,-8.2841209666094E-16,0.430976834037722));
#38278=DIRECTION('center_axis',(0.713612070377342,-2.34196436325345E-15,
0.700541085884164));
#38279=DIRECTION('ref_axis',(0.700541085884164,1.73398305765319E-15,-0.713612070377342));
#38280=DIRECTION('',(-0.700541085884164,-1.73398305765319E-15,0.713612070377342));
#38281=DIRECTION('center_axis',(0.700541085884164,1.73398305765319E-15,
-0.713612070377342));
#38282=DIRECTION('ref_axis',(-0.713612070377342,2.34196436325345E-15,-0.700541085884164));
#38283=DIRECTION('',(4.56527663898138E-16,1.,2.87803349790671E-15));
#38284=DIRECTION('',(0.713612070377342,-2.34196436325345E-15,0.700541085884164));
#38285=DIRECTION('center_axis',(4.56527663898138E-16,1.,2.87803349790671E-15));
#38286=DIRECTION('ref_axis',(0.902362991552081,8.2841209666094E-16,-0.430976834037722));
#38287=DIRECTION('center_axis',(4.56527663898138E-16,1.,2.87803349790671E-15));
#38288=DIRECTION('ref_axis',(0.902362991552081,8.2841209666094E-16,-0.430976834037722));
#38289=DIRECTION('center_axis',(4.56527663898138E-16,1.,2.87803349790671E-15));
#38290=DIRECTION('ref_axis',(0.902362991552081,8.2841209666094E-16,-0.430976834037722));
#38291=DIRECTION('axis',(0.,0.,1.));
#38292=DIRECTION('refdir',(1.,0.,0.));
#38293=DIRECTION('center_axis',(5.00596043934461E-16,1.,1.12027918221652E-15));
#38294=DIRECTION('ref_axis',(1.,-5.00596043934455E-16,-5.57179392097267E-15));
#38295=DIRECTION('center_axis',(-5.00596043934461E-16,-1.,-1.12027918221652E-15));
#38296=DIRECTION('ref_axis',(-1.,5.00596043934455E-16,5.57179392097267E-15));
#38297=DIRECTION('',(1.,-5.00596043934455E-16,-5.57179392097267E-15));
#38298=DIRECTION('center_axis',(-5.00596043934461E-16,-1.,-1.12027918221652E-15));
#38299=DIRECTION('ref_axis',(-5.57179392097266E-15,1.12027918221652E-15,
-1.));
#38300=DIRECTION('',(5.57179392097266E-15,-1.12027918221652E-15,1.));
#38301=DIRECTION('center_axis',(-5.00596043934461E-16,-1.,-1.12027918221652E-15));
#38302=DIRECTION('ref_axis',(1.,-5.00596043934455E-16,-5.57179392097267E-15));
#38303=DIRECTION('',(-1.,5.00596043934455E-16,5.57179392097267E-15));
#38304=DIRECTION('center_axis',(-5.00596043934461E-16,-1.,-1.12027918221652E-15));
#38305=DIRECTION('ref_axis',(5.57179392097266E-15,-1.12027918221652E-15,
1.));
#38306=DIRECTION('',(-5.57179392097266E-15,1.12027918221652E-15,-1.));
#38307=DIRECTION('center_axis',(5.00596043934461E-16,1.,1.12027918221652E-15));
#38308=DIRECTION('ref_axis',(1.,-5.00596043934455E-16,-5.57179392097267E-15));
#38309=DIRECTION('center_axis',(5.00596043934461E-16,1.,1.12027918221652E-15));
#38310=DIRECTION('ref_axis',(1.,-5.00596043934455E-16,-5.57179392097267E-15));
#38311=DIRECTION('center_axis',(5.00596043934461E-16,1.,1.12027918221652E-15));
#38312=DIRECTION('ref_axis',(1.,-5.00596043934455E-16,-5.57179392097267E-15));
#38313=DIRECTION('center_axis',(5.00596043934461E-16,1.,1.12027918221652E-15));
#38314=DIRECTION('ref_axis',(1.,-5.00596043934455E-16,-5.57179392097267E-15));
#38315=DIRECTION('center_axis',(-5.00596043934461E-16,-1.,-1.12027918221652E-15));
#38316=DIRECTION('ref_axis',(5.57179392097266E-15,-1.12027918221652E-15,
1.));
#38317=DIRECTION('',(1.,-5.00596043934455E-16,-5.57179392097266E-15));
#38318=DIRECTION('center_axis',(-5.00596043934461E-16,-1.,-1.12027918221652E-15));
#38319=DIRECTION('ref_axis',(1.,-5.00596043934455E-16,-5.57179392097267E-15));
#38320=DIRECTION('',(-5.57179392097266E-15,1.12027918221652E-15,-1.));
#38321=DIRECTION('center_axis',(-5.00596043934461E-16,-1.,-1.12027918221652E-15));
#38322=DIRECTION('ref_axis',(-5.57179392097266E-15,1.12027918221652E-15,
-1.));
#38323=DIRECTION('',(-1.,5.00596043934455E-16,5.57179392097266E-15));
#38324=DIRECTION('center_axis',(-5.00596043934461E-16,-1.,-1.12027918221652E-15));
#38325=DIRECTION('ref_axis',(-1.,5.00596043934455E-16,5.57179392097267E-15));
#38326=DIRECTION('',(5.57179392097266E-15,-1.12027918221652E-15,1.));
#38327=DIRECTION('center_axis',(5.00596043934461E-16,1.,1.12027918221652E-15));
#38328=DIRECTION('ref_axis',(1.,-5.00596043934455E-16,-5.57179392097267E-15));
#38329=DIRECTION('center_axis',(-5.00596043934461E-16,-1.,-1.12027918221652E-15));
#38330=DIRECTION('ref_axis',(-1.,5.00596043934455E-16,5.57179392097267E-15));
#38331=DIRECTION('',(5.14815917377939E-11,1.,1.12027918192968E-15));
#38332=DIRECTION('',(5.00596044180201E-16,1.,4.41054475357122E-11));
#38333=DIRECTION('center_axis',(5.00596043934461E-16,1.,1.12027918221652E-15));
#38334=DIRECTION('ref_axis',(-0.999766740157022,0.,0.0215978071989372));
#38335=DIRECTION('center_axis',(2.79269661923508E-9,1.12027918081851E-15,
-1.));
#38336=DIRECTION('ref_axis',(-1.,5.00596047063061E-16,-2.79269661923508E-9));
#38337=DIRECTION('center_axis',(-5.00596043934461E-16,-1.,-1.12027918221652E-15));
#38338=DIRECTION('ref_axis',(-1.,5.00596043934455E-16,5.57179392097267E-15));
#38339=DIRECTION('center_axis',(1.,-5.00596043934455E-16,-5.57179392097267E-15));
#38340=DIRECTION('ref_axis',(-5.57179392097266E-15,1.12027918221652E-15,
-1.));
#38341=DIRECTION('center_axis',(1.,-5.00596043934455E-16,-5.57179392097267E-15));
#38342=DIRECTION('ref_axis',(-5.57179392097266E-15,1.12027918221652E-15,
-1.));
#38343=DIRECTION('',(1.,-5.00596043934455E-16,-5.57179392097267E-15));
#38344=DIRECTION('center_axis',(1.,-5.00596043934455E-16,-5.57179392097267E-15));
#38345=DIRECTION('ref_axis',(-5.57179392097266E-15,1.12027918221652E-15,
-1.));
#38346=DIRECTION('',(0.999999999999992,-1.07234894352195E-7,7.46977803037953E-8));
#38347=DIRECTION('center_axis',(5.00596043934461E-16,1.,1.12027918221652E-15));
#38348=DIRECTION('ref_axis',(1.,-5.00596043934455E-16,-5.57179392097267E-15));
#38349=DIRECTION('center_axis',(5.00596043934461E-16,1.,1.12027918221652E-15));
#38350=DIRECTION('ref_axis',(0.560028488394602,-1.20846949316291E-15,0.828473350317593));
#38351=DIRECTION('',(0.626626299212589,1.16622759427748E-9,0.779319883703178));
#38352=DIRECTION('',(-1.,5.00596043934455E-16,5.57179392097267E-15));
#38353=DIRECTION('center_axis',(-5.00596043934461E-16,-1.,-1.12027918221652E-15));
#38354=DIRECTION('ref_axis',(1.,-5.00596043934455E-16,-5.57179392097267E-15));
#38355=DIRECTION('',(5.57179392097267E-15,-1.12027918221652E-15,1.));
#38356=DIRECTION('',(-0.779319883703586,-1.08364385785013E-9,-0.626626299212081));
#38357=DIRECTION('center_axis',(5.00596043934461E-16,1.,1.12027918221652E-15));
#38358=DIRECTION('ref_axis',(1.,-5.00596043934455E-16,-5.57179392097267E-15));
#38359=DIRECTION('center_axis',(5.00596043934461E-16,1.,1.12027918221652E-15));
#38360=DIRECTION('ref_axis',(1.,-5.00596043934455E-16,-5.57179392097267E-15));
#38361=DIRECTION('center_axis',(5.00596043934461E-16,1.,1.12027918221652E-15));
#38362=DIRECTION('ref_axis',(0.828473350317593,2.12657775322542E-16,-0.560028488394602));
#38363=DIRECTION('',(0.779319883703892,1.08347942622894E-9,-0.626626299211701));
#38364=DIRECTION('',(5.57179392097267E-15,-1.12027918221652E-15,1.));
#38365=DIRECTION('center_axis',(-5.00596043934461E-16,-1.,-1.12027918221652E-15));
#38366=DIRECTION('ref_axis',(-5.57179392097267E-15,1.12027918221652E-15,
-1.));
#38367=DIRECTION('',(1.,-5.00596043934455E-16,-5.57179392097267E-15));
#38368=DIRECTION('',(-0.626626299195176,-2.0704530707019E-10,0.77931988371718));
#38369=DIRECTION('center_axis',(5.00596043934461E-16,1.,1.12027918221652E-15));
#38370=DIRECTION('ref_axis',(1.,-5.00596043934455E-16,-5.57179392097267E-15));
#38371=DIRECTION('center_axis',(5.00596043934461E-16,1.,1.12027918221652E-15));
#38372=DIRECTION('ref_axis',(1.,-5.00596043934455E-16,-5.57179392097267E-15));
#38373=DIRECTION('center_axis',(5.00596043934461E-16,1.,1.12027918221652E-15));
#38374=DIRECTION('ref_axis',(-0.560028488394602,1.20846949316291E-15,-0.828473350317593));
#38375=DIRECTION('',(-0.626626299212589,1.16622995081446E-9,-0.779319883703178));
#38376=DIRECTION('',(-5.57179392097267E-15,1.12027918221652E-15,-1.));
#38377=DIRECTION('',(0.779319883703586,-1.08364601666983E-9,0.626626299212081));
#38378=DIRECTION('center_axis',(5.00596043934461E-16,1.,1.12027918221652E-15));
#38379=DIRECTION('ref_axis',(1.,-5.00596043934455E-16,-5.57179392097267E-15));
#38380=DIRECTION('center_axis',(5.00596043934461E-16,1.,1.12027918221652E-15));
#38381=DIRECTION('ref_axis',(1.,-5.00596043934455E-16,-5.57179392097267E-15));
#38382=DIRECTION('center_axis',(5.00596043934461E-16,1.,1.12027918221652E-15));
#38383=DIRECTION('ref_axis',(-0.828473350317593,-2.12657775322542E-16,0.560028488394602));
#38384=DIRECTION('',(-0.779319883703892,1.08347879401104E-9,0.626626299211701));
#38385=DIRECTION('',(-5.57179392097267E-15,1.12027918221652E-15,-1.));
#38386=DIRECTION('center_axis',(-5.00596043934461E-16,-1.,-1.12027918221652E-15));
#38387=DIRECTION('ref_axis',(5.57179392097267E-15,-1.12027918221652E-15,
1.));
#38388=DIRECTION('',(-1.,5.00596043934455E-16,5.57179392097267E-15));
#38389=DIRECTION('',(0.626626299195176,-2.07044188331798E-10,-0.77931988371718));
#38390=DIRECTION('center_axis',(5.00596043934461E-16,1.,1.12027918221652E-15));
#38391=DIRECTION('ref_axis',(1.,-5.00596043934455E-16,-5.57179392097267E-15));
#38392=DIRECTION('center_axis',(5.00596043934461E-16,1.,1.12027918221652E-15));
#38393=DIRECTION('ref_axis',(1.,-5.00596043934455E-16,-5.57179392097267E-15));
#38394=DIRECTION('',(5.00596043934461E-16,1.,1.12027918221652E-15));
#38395=DIRECTION('center_axis',(5.00596043934461E-16,1.,1.12027918221652E-15));
#38396=DIRECTION('ref_axis',(1.,-5.00596043934455E-16,-5.57179392097267E-15));
#38397=DIRECTION('',(5.00596043934461E-16,1.,1.12027918221652E-15));
#38398=DIRECTION('center_axis',(5.00596043934461E-16,1.,1.12027918221652E-15));
#38399=DIRECTION('ref_axis',(1.,-5.00596043934455E-16,-5.57179392097267E-15));
#38400=DIRECTION('',(5.00596043934461E-16,1.,1.12027918221652E-15));
#38401=DIRECTION('center_axis',(5.00596043934461E-16,1.,1.12027918221652E-15));
#38402=DIRECTION('ref_axis',(1.,-5.00596043934455E-16,-5.57179392097267E-15));
#38403=DIRECTION('',(5.00596043934461E-16,1.,1.12027918221652E-15));
#38404=DIRECTION('center_axis',(5.00596043934461E-16,1.,1.12027918221652E-15));
#38405=DIRECTION('ref_axis',(-0.00546733966186705,-1.08624916607697E-15,
0.999985053986819));
#38406=DIRECTION('center_axis',(0.560028451650215,-2.46470073675675E-8,
-0.828473375155932));
#38407=DIRECTION('ref_axis',(-6.58554294166816E-9,-1.,2.52982371904519E-8));
#38408=DIRECTION('center_axis',(5.00596043934461E-16,1.,1.12027918221652E-15));
#38409=DIRECTION('ref_axis',(0.560028488394602,-1.20846949316291E-15,0.828473350317593));
#38410=DIRECTION('center_axis',(0.828473350319084,2.12657775319325E-16,
-0.560028488392396));
#38411=DIRECTION('ref_axis',(-2.1601502742123E-11,-1.,-3.19563778939926E-11));
#38412=DIRECTION('center_axis',(0.442362010728513,0.862800087335627,-0.244728136424609));
#38413=DIRECTION('ref_axis',(0.67492455342951,-0.499967312100476,-0.542687326191612));
#38414=DIRECTION('center_axis',(5.00596043934461E-16,1.,1.12027918221652E-15));
#38415=DIRECTION('ref_axis',(-5.57179392097266E-15,1.12027918221652E-15,
-1.));
#38416=DIRECTION('center_axis',(5.00596043934461E-16,1.,1.12027918221652E-15));
#38417=DIRECTION('ref_axis',(5.57179392097266E-15,-1.12027918221652E-15,
1.));
#38418=DIRECTION('',(-5.00596043934461E-16,-1.,-1.12027918221652E-15));
#38419=DIRECTION('center_axis',(5.00596043934461E-16,1.,1.12027918221652E-15));
#38420=DIRECTION('ref_axis',(5.57179392097266E-15,-1.12027918221652E-15,
1.));
#38421=DIRECTION('center_axis',(5.00596043934461E-16,1.,1.12027918221652E-15));
#38422=DIRECTION('ref_axis',(0.875020006168853,-9.80343870285712E-16,0.484086757517968));
#38423=DIRECTION('center_axis',(5.00596043934461E-16,1.,1.12027918221652E-15));
#38424=DIRECTION('ref_axis',(0.828473350317593,2.12657775322542E-16,-0.560028488394602));
#38425=DIRECTION('center_axis',(5.00596043934461E-16,1.,1.12027918221652E-15));
#38426=DIRECTION('ref_axis',(-5.57179392097266E-15,1.12027918221652E-15,
-1.));
#38427=DIRECTION('center_axis',(5.00596043934461E-16,1.,1.12027918221652E-15));
#38428=DIRECTION('ref_axis',(-0.560028488394602,1.20846949316291E-15,-0.828473350317593));
#38429=DIRECTION('center_axis',(5.00596043934461E-16,1.,1.12027918221652E-15));
#38430=DIRECTION('ref_axis',(-0.875020006168853,9.80343870285712E-16,-0.484086757517968));
#38431=DIRECTION('center_axis',(5.00596043934461E-16,1.,1.12027918221652E-15));
#38432=DIRECTION('ref_axis',(-0.828473350317593,-2.12657775322542E-16,0.560028488394602));
#38433=DIRECTION('center_axis',(5.00596043934461E-16,1.,1.12027918221652E-15));
#38434=DIRECTION('ref_axis',(5.57179392097266E-15,-1.12027918221652E-15,
1.));
#38435=DIRECTION('center_axis',(5.00596043934461E-16,1.,1.12027918221652E-15));
#38436=DIRECTION('ref_axis',(5.57179392097266E-15,-1.12027918221652E-15,
1.));
#38437=DIRECTION('center_axis',(5.00596043934461E-16,1.,1.12027918221652E-15));
#38438=DIRECTION('ref_axis',(-0.00546733966186705,-1.08624916607697E-15,
0.999985053986819));
#38439=DIRECTION('center_axis',(-5.00596043934461E-16,-1.,-1.12027918221652E-15));
#38440=DIRECTION('ref_axis',(0.484075514152618,-1.22259995249413E-15,0.875026226234322));
#38441=DIRECTION('center_axis',(0.875024443058473,1.04269557576734E-16,
-0.484078737448991));
#38442=DIRECTION('ref_axis',(-5.00596043934461E-16,-1.,-1.12027918221652E-15));
#38443=DIRECTION('center_axis',(0.875024443058478,-9.80337106658779E-16,
0.484078737448981));
#38444=DIRECTION('ref_axis',(-5.00596043934461E-16,-1.,-1.12027918221652E-15));
#38445=DIRECTION('center_axis',(5.00596043934461E-16,1.,1.12027918221652E-15));
#38446=DIRECTION('ref_axis',(1.,-5.00596043934455E-16,-5.57179392097267E-15));
#38447=DIRECTION('',(0.626626299213187,8.21459917499281E-8,-0.779319883702693));
#38448=DIRECTION('',(-1.,-7.69979604021266E-13,5.5717939209718E-15));
#38449=DIRECTION('',(0.626626299213087,-8.21413452539801E-8,0.779319883702774));
#38450=DIRECTION('center_axis',(5.00596043934461E-16,1.,1.12027918221652E-15));
#38451=DIRECTION('ref_axis',(1.,-5.00596043934455E-16,-5.57179392097267E-15));
#38452=DIRECTION('center_axis',(5.00596043934461E-16,1.,1.12027918221652E-15));
#38453=DIRECTION('ref_axis',(0.875024725126116,-9.80336676666241E-16,0.484078227581002));
#38454=DIRECTION('',(-0.779319883702693,8.21478081333498E-8,-0.626626299213187));
#38455=DIRECTION('',(5.57179392097228E-15,-7.71593186762516E-13,1.));
#38456=DIRECTION('',(0.779319883702774,-8.21427723649357E-8,-0.626626299213086));
#38457=DIRECTION('center_axis',(5.00596043934461E-16,1.,1.12027918221652E-15));
#38458=DIRECTION('ref_axis',(1.,-5.00596043934455E-16,-5.57179392097267E-15));
#38459=DIRECTION('center_axis',(-5.00596043934461E-16,-1.,-1.12027918221652E-15));
#38460=DIRECTION('ref_axis',(-0.484075514152618,1.22259995249413E-15,-0.875026226234322));
#38461=DIRECTION('',(-0.626626299213187,8.21459906311898E-8,0.779319883702693));
#38462=DIRECTION('',(1.,-7.70973503624234E-13,-5.57179392097353E-15));
#38463=DIRECTION('',(-0.626626299213087,-8.21413428804951E-8,-0.779319883702774));
#38464=DIRECTION('center_axis',(5.00596043934461E-16,1.,1.12027918221652E-15));
#38465=DIRECTION('ref_axis',(1.,-5.00596043934455E-16,-5.57179392097267E-15));
#38466=DIRECTION('center_axis',(5.00596043934461E-16,1.,1.12027918221652E-15));
#38467=DIRECTION('ref_axis',(-0.875025039198583,9.80336197883637E-16,-0.484077659859984));
#38468=DIRECTION('',(0.779319883702693,8.21474230077581E-8,0.626626299213187));
#38469=DIRECTION('',(-5.57179392097305E-15,-7.69352628398084E-13,-1.));
#38470=DIRECTION('',(-0.779319883702773,-8.21432340431895E-8,0.626626299213087));
#38471=DIRECTION('center_axis',(0.626626299211202,-1.18674248841174E-15,
0.779319883704293));
#38472=DIRECTION('ref_axis',(-5.00596043934461E-16,-1.,-1.12027918221652E-15));
#38473=DIRECTION('center_axis',(-0.626626299211202,1.18674248841174E-15,
-0.779319883704293));
#38474=DIRECTION('ref_axis',(0.674910816962253,-0.499999999999999,-0.542674293796331));
#38475=DIRECTION('',(0.626626006620295,2.71817970602453E-7,0.779320118967185));
#38476=DIRECTION('center_axis',(0.887935155463387,-0.383064347768995,0.254622986316092));
#38477=DIRECTION('ref_axis',(0.125932648739722,-0.329956706076109,-0.935558410841783));
#38478=DIRECTION('center_axis',(0.626626299211202,-1.18674248841174E-15,
0.779319883704293));
#38479=DIRECTION('ref_axis',(5.00596043934461E-16,1.,1.12027918221652E-15));
#38480=DIRECTION('center_axis',(-0.626626299211202,1.18674248841174E-15,
-0.779319883704293));
#38481=DIRECTION('ref_axis',(-0.674910816962253,0.499999999999999,0.542674293796331));
#38482=DIRECTION('center_axis',(-0.705697508381116,0.522807970064417,-0.478187048237203));
#38483=DIRECTION('ref_axis',(-0.384232653056518,0.284654389439118,0.87825801840814));
#38484=DIRECTION('center_axis',(-0.595274941165209,-0.803522087077111,2.41658023188801E-15));
#38485=DIRECTION('ref_axis',(5.39575063434723E-7,-3.99734514942978E-7,0.999999999999775));
#38486=DIRECTION('center_axis',(-1.,5.00596043934455E-16,5.57179392097267E-15));
#38487=DIRECTION('ref_axis',(5.57179392097266E-15,-1.12027918221652E-15,
1.));
#38488=DIRECTION('center_axis',(-1.,5.00596043934455E-16,5.57179392097267E-15));
#38489=DIRECTION('ref_axis',(5.57179392097266E-15,-1.12027918221652E-15,
1.));
#38490=DIRECTION('',(-0.999999999999992,-1.07234893281703E-7,-7.46977803037956E-8));
#38491=DIRECTION('center_axis',(-1.,5.00596043934455E-16,5.57179392097267E-15));
#38492=DIRECTION('ref_axis',(5.57179392097266E-15,-1.12027918221652E-15,
1.));
#38493=DIRECTION('center_axis',(5.00596043934461E-16,1.,1.12027918221652E-15));
#38494=DIRECTION('ref_axis',(0.999766740157022,0.,-0.0215978071989372));
#38495=DIRECTION('center_axis',(-5.00596043934461E-16,-1.,-1.12027918221652E-15));
#38496=DIRECTION('ref_axis',(1.,-5.00596043934455E-16,-5.57179392097267E-15));
#38497=DIRECTION('center_axis',(-2.79269672678808E-9,-1.12027918081851E-15,
1.));
#38498=DIRECTION('ref_axis',(1.,-5.00596047063061E-16,2.79269672678808E-9));
#38499=DIRECTION('center_axis',(5.00596043934461E-16,1.,1.12027918221652E-15));
#38500=DIRECTION('ref_axis',(1.,-5.00596043934455E-16,-5.57179392097267E-15));
#38501=DIRECTION('',(-5.14805905457061E-11,1.,1.12027918250336E-15));
#38502=DIRECTION('',(5.00596043688721E-16,1.,-4.41032069773478E-11));
#38503=DIRECTION('center_axis',(1.,-5.00596043934455E-16,-5.57179392097267E-15));
#38504=DIRECTION('ref_axis',(-5.57179392097267E-15,1.12027918221652E-15,
-1.));
#38505=DIRECTION('',(-7.46977803037955E-8,-1.07234894902578E-7,0.999999999999991));
#38506=DIRECTION('',(2.15527966388097E-12,-1.1202791822176E-15,1.));
#38507=DIRECTION('',(7.46713262143734E-8,1.0748494691062E-7,0.999999999999991));
#38508=DIRECTION('',(5.00596044221303E-16,1.,5.14822114209322E-11));
#38509=DIRECTION('center_axis',(5.57179392097266E-15,-1.12027918221652E-15,
1.));
#38510=DIRECTION('ref_axis',(1.,-5.00596043934455E-16,-5.57179392097267E-15));
#38511=DIRECTION('center_axis',(5.57179392097266E-15,-1.12027918221652E-15,
1.));
#38512=DIRECTION('ref_axis',(1.,-5.00596043934455E-16,-5.57179392097267E-15));
#38513=DIRECTION('center_axis',(5.57179392097266E-15,-1.12027918221652E-15,
1.));
#38514=DIRECTION('ref_axis',(1.,-5.00596043934455E-16,-5.57179392097267E-15));
#38515=DIRECTION('center_axis',(5.00596043934461E-16,1.,1.12027918221652E-15));
#38516=DIRECTION('ref_axis',(-0.0215978071989372,1.23572649697409E-15,-0.999766740157022));
#38517=DIRECTION('center_axis',(-5.00596043934461E-16,-1.,-1.12027918221652E-15));
#38518=DIRECTION('ref_axis',(-5.57179392097266E-15,1.12027918221652E-15,
-1.));
#38519=DIRECTION('center_axis',(1.,-5.0059604706306E-16,2.79269541533708E-9));
#38520=DIRECTION('ref_axis',(2.79269541533708E-9,1.12027918081851E-15,-1.));
#38521=DIRECTION('center_axis',(5.00596043934461E-16,1.,1.12027918221652E-15));
#38522=DIRECTION('ref_axis',(1.,-5.00596043934455E-16,-5.57179392097267E-15));
#38523=DIRECTION('',(-4.41048824446361E-11,1.,1.12027918246227E-15));
#38524=DIRECTION('center_axis',(-5.57179392097266E-15,1.12027918221652E-15,
-1.));
#38525=DIRECTION('ref_axis',(-1.,5.00596043934455E-16,5.57179392097267E-15));
#38526=DIRECTION('',(0.999999999999991,1.07484947530303E-7,-7.46713284325632E-8));
#38527=DIRECTION('',(1.,-5.00596043932047E-16,-2.15527966388097E-12));
#38528=DIRECTION('center_axis',(0.999999999999976,2.17635944148899E-7,-5.57179367715952E-15));
#38529=DIRECTION('ref_axis',(-5.75848107867473E-13,2.62032228371319E-6,
-0.999999999996567));
#38530=DIRECTION('center_axis',(-0.626626299211194,-5.59369195590911E-16,
0.7793198837043));
#38531=DIRECTION('ref_axis',(-5.00596043934461E-16,-1.,-1.12027918221652E-15));
#38532=DIRECTION('center_axis',(-0.626626299211194,-5.59369195590911E-16,
0.7793198837043));
#38533=DIRECTION('ref_axis',(-5.00596043934461E-16,-1.,-1.12027918221652E-15));
#38534=DIRECTION('',(-0.626626006343689,-2.71886424419567E-7,0.779320119189595));
#38535=DIRECTION('center_axis',(0.342295357878412,-0.707106781186532,-0.618735717390642));
#38536=DIRECTION('ref_axis',(-0.342295357878411,-0.707106781186553,0.618735717390618));
#38537=DIRECTION('center_axis',(-0.875024443058478,9.80337106658779E-16,
-0.484078737448981));
#38538=DIRECTION('ref_axis',(-5.00596043934461E-16,-1.,-1.12027918221652E-15));
#38539=DIRECTION('center_axis',(-0.442362657739701,-0.862799639016597,-0.244728547477197));
#38540=DIRECTION('ref_axis',(0.674924135928914,-0.49996807137079,0.542687145923303));
#38541=DIRECTION('center_axis',(-0.82847335444329,2.83557470020383E-8,-0.560028482291286));
#38542=DIRECTION('ref_axis',(-2.28233127966104E-8,-1.,-1.68692143143682E-8));
#38543=DIRECTION('center_axis',(-0.626626299211194,-5.59369195590911E-16,
0.7793198837043));
#38544=DIRECTION('ref_axis',(5.00596043934461E-16,1.,1.12027918221652E-15));
#38545=DIRECTION('center_axis',(-0.626626299211194,-5.59369195590911E-16,
0.7793198837043));
#38546=DIRECTION('ref_axis',(5.00596043934461E-16,1.,1.12027918221652E-15));
#38547=DIRECTION('center_axis',(0.,0.707106781186545,0.70710678118655));
#38548=DIRECTION('ref_axis',(0.,0.707106781186548,-0.707106781186548));
#38549=DIRECTION('center_axis',(1.,-5.00596043934455E-16,-5.57179392097267E-15));
#38550=DIRECTION('ref_axis',(-5.57179392097266E-15,1.12027918221652E-15,
-1.));
#38551=DIRECTION('center_axis',(1.,-5.00596043934455E-16,-5.57179392097267E-15));
#38552=DIRECTION('ref_axis',(-5.57179392097266E-15,1.12027918221652E-15,
-1.));
#38553=DIRECTION('center_axis',(5.00596043934461E-16,1.,1.12027918221652E-15));
#38554=DIRECTION('ref_axis',(-0.00546733966186705,-1.08624916607697E-15,
0.999985053986819));
#38555=DIRECTION('center_axis',(-0.560028488398899,1.2084694931618E-15,
-0.828473350314689));
#38556=DIRECTION('ref_axis',(-7.44149101541802E-12,-1.,5.02881413593191E-12));
#38557=DIRECTION('center_axis',(-0.244728038654104,0.862800306783108,-0.442361636799001));
#38558=DIRECTION('ref_axis',(-0.542687484719605,-0.499966948603119,-0.674924695231397));
#38559=DIRECTION('center_axis',(0.779319883704293,3.11871947293856E-16,
-0.626626299211202));
#38560=DIRECTION('ref_axis',(5.00596043934461E-16,1.,1.12027918221652E-15));
#38561=DIRECTION('',(0.779320120962128,2.74269932471282E-7,-0.62662600413923));
#38562=DIRECTION('center_axis',(-0.779319883704293,-3.11871947293856E-16,
0.626626299211202));
#38563=DIRECTION('ref_axis',(0.54267429379633,0.499999999999998,0.674910816962253));
#38564=DIRECTION('center_axis',(-0.478187048237203,0.522807970064417,0.705697508381116));
#38565=DIRECTION('ref_axis',(0.87825801840814,0.284654389439118,0.384232653056518));
#38566=DIRECTION('center_axis',(2.91450932048691E-15,-0.803522087077112,
0.595274941165208));
#38567=DIRECTION('ref_axis',(0.999999999999775,-3.99734512055927E-7,-5.39575060374155E-7));
#38568=DIRECTION('center_axis',(5.57179392097266E-15,-1.12027918221652E-15,
1.));
#38569=DIRECTION('ref_axis',(1.,-5.00596043934455E-16,-5.57179392097267E-15));
#38570=DIRECTION('center_axis',(5.57179392097266E-15,-1.12027918221652E-15,
1.));
#38571=DIRECTION('ref_axis',(1.,-5.00596043934455E-16,-5.57179392097267E-15));
#38572=DIRECTION('center_axis',(5.57179402992023E-15,2.17635943782516E-7,
0.999999999999976));
#38573=DIRECTION('ref_axis',(0.999999999996567,2.62032228244231E-6,-5.75848106983604E-13));
#38574=DIRECTION('center_axis',(-0.7793198837043,1.09212084877752E-15,-0.626626299211194));
#38575=DIRECTION('ref_axis',(-5.00596043934461E-16,-1.,-1.12027918221652E-15));
#38576=DIRECTION('center_axis',(-0.7793198837043,1.09212084877752E-15,-0.626626299211194));
#38577=DIRECTION('ref_axis',(-5.00596043934461E-16,-1.,-1.12027918221652E-15));
#38578=DIRECTION('',(-0.779320120541394,-2.73779246727676E-7,-0.626626004662488));
#38579=DIRECTION('center_axis',(0.618735717390639,-0.707106781186534,0.342295357878411));
#38580=DIRECTION('ref_axis',(-0.618735717390618,-0.707106781186553,-0.342295357878411));
#38581=DIRECTION('center_axis',(0.484078737448981,7.3794376656927E-16,-0.875024443058478));
#38582=DIRECTION('ref_axis',(-5.00596043934461E-16,-1.,-1.12027918221652E-15));
#38583=DIRECTION('center_axis',(0.244728012110787,-0.862800336285763,-0.442361593940383));
#38584=DIRECTION('ref_axis',(-0.542687494645365,-0.499966898890162,0.674924724076465));
#38585=DIRECTION('center_axis',(-0.7793198837043,1.09212084877752E-15,-0.626626299211194));
#38586=DIRECTION('ref_axis',(5.00596043934461E-16,1.,1.12027918221652E-15));
#38587=DIRECTION('center_axis',(-0.7793198837043,1.09212084877752E-15,-0.626626299211194));
#38588=DIRECTION('ref_axis',(5.00596043934461E-16,1.,1.12027918221652E-15));
#38589=DIRECTION('center_axis',(-0.70710678118655,0.707106781186545,0.));
#38590=DIRECTION('ref_axis',(0.70710678118655,0.707106781186545,0.));
#38591=DIRECTION('center_axis',(5.57179392097266E-15,-1.12027918221652E-15,
1.));
#38592=DIRECTION('ref_axis',(1.,-5.00596043934455E-16,-5.57179392097267E-15));
#38593=DIRECTION('center_axis',(5.57179392097266E-15,-1.12027918221652E-15,
1.));
#38594=DIRECTION('ref_axis',(1.,-5.00596043934455E-16,-5.57179392097267E-15));
#38595=DIRECTION('center_axis',(5.00596043934461E-16,1.,1.12027918221652E-15));
#38596=DIRECTION('ref_axis',(-0.00546733966186705,-1.08624916607697E-15,
0.999985053986819));
#38597=DIRECTION('center_axis',(-0.484078737448991,1.22259956840877E-15,
-0.875024443058473));
#38598=DIRECTION('ref_axis',(-5.00596043934461E-16,-1.,-1.12027918221652E-15));
#38599=DIRECTION('center_axis',(0.254622986316092,-0.383064347768995,-0.887935155463387));
#38600=DIRECTION('ref_axis',(-0.935558410841783,-0.329956706076109,-0.125932648739722));
#38601=DIRECTION('center_axis',(-0.779319883704293,-3.11871947293856E-16,
0.626626299211202));
#38602=DIRECTION('ref_axis',(-0.54267429379633,-0.499999999999998,-0.674910816962253));
#38603=DIRECTION('center_axis',(0.779319883704293,3.11871947293856E-16,
-0.626626299211202));
#38604=DIRECTION('ref_axis',(-5.00596043934461E-16,-1.,-1.12027918221652E-15));
#38605=DIRECTION('center_axis',(5.00596043934461E-16,1.,1.12027918221652E-15));
#38606=DIRECTION('ref_axis',(0.00546733966186705,1.08624916607697E-15,-0.999985053986819));
#38607=DIRECTION('center_axis',(-0.875024443058473,-1.04269557576734E-16,
0.484078737448991));
#38608=DIRECTION('ref_axis',(-5.00596043934461E-16,-1.,-1.12027918221652E-15));
#38609=DIRECTION('center_axis',(0.4423626577397,-0.862799639016598,0.244728547477196));
#38610=DIRECTION('ref_axis',(-0.674924135928915,-0.499968071370788,-0.542687145923305));
#38611=DIRECTION('center_axis',(0.82847335444329,2.83557475385409E-8,0.560028482291286));
#38612=DIRECTION('ref_axis',(2.28233165805793E-8,-1.,1.68692096745776E-8));
#38613=DIRECTION('center_axis',(0.626626299211194,5.59369195590911E-16,
-0.7793198837043));
#38614=DIRECTION('ref_axis',(5.00596043934461E-16,1.,1.12027918221652E-15));
#38615=DIRECTION('center_axis',(0.626626299211194,5.59369195590911E-16,
-0.7793198837043));
#38616=DIRECTION('ref_axis',(5.00596043934461E-16,1.,1.12027918221652E-15));
#38617=DIRECTION('',(0.626626006343689,-2.71886423154627E-7,-0.779320119189595));
#38618=DIRECTION('center_axis',(0.626626299211194,5.59369195590911E-16,
-0.7793198837043));
#38619=DIRECTION('ref_axis',(-5.00596043934461E-16,-1.,-1.12027918221652E-15));
#38620=DIRECTION('center_axis',(0.626626299211194,5.59369195590911E-16,
-0.7793198837043));
#38621=DIRECTION('ref_axis',(-5.00596043934461E-16,-1.,-1.12027918221652E-15));
#38622=DIRECTION('center_axis',(-0.342295357878412,-0.707106781186532,0.618735717390642));
#38623=DIRECTION('ref_axis',(0.342295357878402,-0.707106781186555,-0.618735717390621));
#38624=DIRECTION('center_axis',(-0.999999999999976,2.17635947033991E-7,
5.57179416478555E-15));
#38625=DIRECTION('ref_axis',(5.75848115427344E-13,2.62032228147263E-6,0.999999999996567));
#38626=DIRECTION('center_axis',(-1.,5.00596043934455E-16,5.57179392097267E-15));
#38627=DIRECTION('ref_axis',(5.57179392097266E-15,-1.12027918221652E-15,
1.));
#38628=DIRECTION('',(-1.,5.00596043932046E-16,2.15551302339697E-12));
#38629=DIRECTION('center_axis',(-1.,5.00596043934455E-16,5.57179392097267E-15));
#38630=DIRECTION('ref_axis',(5.57179392097266E-15,-1.12027918221652E-15,
1.));
#38631=DIRECTION('center_axis',(5.57179392097266E-15,-1.12027918221652E-15,
1.));
#38632=DIRECTION('ref_axis',(1.,-5.00596043934455E-16,-5.57179392097267E-15));
#38633=DIRECTION('',(-0.999999999999991,1.07484948739395E-7,7.46713262143735E-8));
#38634=DIRECTION('',(4.41048278525739E-11,1.,1.12027918197078E-15));
#38635=DIRECTION('center_axis',(5.00596043934461E-16,1.,1.12027918221652E-15));
#38636=DIRECTION('ref_axis',(-0.707106781189596,-4.38182149261264E-16,0.707106781183499));
#38637=DIRECTION('center_axis',(-5.00596043934461E-16,-1.,-1.12027918221652E-15));
#38638=DIRECTION('ref_axis',(5.57179392097266E-15,-1.12027918221652E-15,
1.));
#38639=DIRECTION('',(5.00596043647619E-16,1.,-5.14799708625678E-11));
#38640=DIRECTION('center_axis',(5.00596043934461E-16,1.,1.12027918221652E-15));
#38641=DIRECTION('ref_axis',(0.0215978071989347,-1.23572649697409E-15,0.999766740157022));
#38642=DIRECTION('center_axis',(-1.,5.00596047063061E-16,-2.79269621677908E-9));
#38643=DIRECTION('ref_axis',(-2.79269621677908E-9,-1.12027918081851E-15,
1.));
#38644=DIRECTION('center_axis',(-5.57179392097266E-15,1.12027918221652E-15,
-1.));
#38645=DIRECTION('ref_axis',(-1.,5.00596043934455E-16,5.57179392097267E-15));
#38646=DIRECTION('center_axis',(-5.57179392097266E-15,1.12027918221652E-15,
-1.));
#38647=DIRECTION('ref_axis',(-1.,5.00596043934455E-16,5.57179392097267E-15));
#38648=DIRECTION('center_axis',(-5.57179392097266E-15,1.12027918221652E-15,
-1.));
#38649=DIRECTION('ref_axis',(-1.,5.00596043934455E-16,5.57179392097267E-15));
#38650=DIRECTION('',(7.46977803037954E-8,-1.0723489266202E-7,-0.999999999999991));
#38651=DIRECTION('center_axis',(-1.,5.00596043934455E-16,5.57179392097267E-15));
#38652=DIRECTION('ref_axis',(5.57179392097267E-15,-1.12027918221652E-15,
1.));
#38653=DIRECTION('',(-2.15527966388097E-12,1.1202791822176E-15,-1.));
#38654=DIRECTION('',(-7.46713339879133E-8,1.07302226011078E-7,-0.999999999999991));
#38655=DIRECTION('center_axis',(-5.57179392097266E-15,1.12027918221652E-15,
-1.));
#38656=DIRECTION('ref_axis',(-1.,5.00596043934455E-16,5.57179392097267E-15));
#38657=DIRECTION('center_axis',(-5.57179392097266E-15,1.12027918221652E-15,
-1.));
#38658=DIRECTION('ref_axis',(-1.,5.00596043934455E-16,5.57179392097267E-15));
#38659=DIRECTION('center_axis',(-0.47818704823722,-0.522807970064411,-0.705697508381108));
#38660=DIRECTION('ref_axis',(-0.87825801840813,0.284654389439118,0.38423265305654));
#38661=DIRECTION('center_axis',(0.7793198837043,-1.09212084877752E-15,0.626626299211194));
#38662=DIRECTION('ref_axis',(5.00596043934461E-16,1.,1.12027918221652E-15));
#38663=DIRECTION('center_axis',(-2.91450932149465E-15,0.803522086951483,
-0.595274941334786));
#38664=DIRECTION('ref_axis',(-0.999999999999775,-3.99555386113565E-7,-5.39333260137364E-7));
#38665=DIRECTION('center_axis',(0.7793198837043,-1.09212084877752E-15,0.626626299211194));
#38666=DIRECTION('ref_axis',(5.00596043934461E-16,1.,1.12027918221652E-15));
#38667=DIRECTION('',(0.779320120539837,-2.73783421093733E-7,0.626626004664424));
#38668=DIRECTION('center_axis',(-0.244728012110788,-0.862800336285764,0.442361593940382));
#38669=DIRECTION('ref_axis',(0.542687494645364,-0.499966898890161,-0.674924724076466));
#38670=DIRECTION('center_axis',(-0.560028451650283,-2.46469991572629E-8,
0.828473375155886));
#38671=DIRECTION('ref_axis',(6.58553923956407E-9,-1.,-2.52982297828268E-8));
#38672=DIRECTION('center_axis',(5.00596043934461E-16,1.,1.12027918221652E-15));
#38673=DIRECTION('ref_axis',(0.00546733966186705,1.08624916607697E-15,-0.999985053986819));
#38674=DIRECTION('center_axis',(-0.828473350319084,-2.12657775319325E-16,
0.560028488392396));
#38675=DIRECTION('ref_axis',(2.16005015500351E-11,-1.,3.19541373356282E-11));
#38676=DIRECTION('center_axis',(-0.442362010728512,0.862800087335627,0.244728136424611));
#38677=DIRECTION('ref_axis',(-0.674924553429511,-0.499967312100476,0.542687326191611));
#38678=DIRECTION('center_axis',(-0.626626299211202,1.18674248841174E-15,
-0.779319883704293));
#38679=DIRECTION('ref_axis',(5.00596043934461E-16,1.,1.12027918221652E-15));
#38680=DIRECTION('',(-0.626626006620295,2.71817973008439E-7,-0.779320118967185));
#38681=DIRECTION('center_axis',(0.626626299211202,-1.18674248841174E-15,
0.779319883704293));
#38682=DIRECTION('ref_axis',(0.674910816962253,0.499999999999999,-0.54267429379633));
#38683=DIRECTION('center_axis',(0.705697508381122,0.522807970064412,0.478187048237199));
#38684=DIRECTION('ref_axis',(0.384232653056518,0.284654389439118,-0.87825801840814));
#38685=DIRECTION('center_axis',(0.595274941165208,-0.803522087077112,-4.21691836509533E-15));
#38686=DIRECTION('ref_axis',(-5.39575061594927E-7,-3.99734511339439E-7,
-0.999999999999775));
#38687=DIRECTION('center_axis',(1.,-5.00596043934455E-16,-5.57179392097267E-15));
#38688=DIRECTION('ref_axis',(-5.57179392097266E-15,1.12027918221652E-15,
-1.));
#38689=DIRECTION('center_axis',(1.,-5.00596043934455E-16,-5.57179392097267E-15));
#38690=DIRECTION('ref_axis',(-5.57179392097266E-15,1.12027918221652E-15,
-1.));
#38691=DIRECTION('center_axis',(-0.626626299211202,1.18674248841174E-15,
-0.779319883704293));
#38692=DIRECTION('ref_axis',(-5.00596043934461E-16,-1.,-1.12027918221652E-15));
#38693=DIRECTION('center_axis',(0.626626299211202,-1.18674248841174E-15,
0.779319883704293));
#38694=DIRECTION('ref_axis',(-0.674910816962253,-0.499999999999999,0.54267429379633));
#38695=DIRECTION('center_axis',(-0.887935155463387,-0.383064347768995,-0.254622986316092));
#38696=DIRECTION('ref_axis',(-0.125932648739722,-0.329956706076109,0.935558410841783));
#38697=DIRECTION('center_axis',(-0.618735717390635,-0.707106781186537,-0.342295357878415));
#38698=DIRECTION('ref_axis',(0.618735717390611,-0.707106781186558,0.342295357878414));
#38699=DIRECTION('center_axis',(0.7793198837043,-1.09212084877752E-15,0.626626299211194));
#38700=DIRECTION('ref_axis',(-5.00596043934461E-16,-1.,-1.12027918221652E-15));
#38701=DIRECTION('center_axis',(-0.484078737448981,-7.3794376656927E-16,
0.875024443058478));
#38702=DIRECTION('ref_axis',(-5.00596043934461E-16,-1.,-1.12027918221652E-15));
#38703=DIRECTION('center_axis',(0.7793198837043,-1.09212084877752E-15,0.626626299211194));
#38704=DIRECTION('ref_axis',(-5.00596043934461E-16,-1.,-1.12027918221652E-15));
#38705=DIRECTION('center_axis',(-5.57179381202484E-15,2.17635945960674E-7,
-0.999999999999976));
#38706=DIRECTION('ref_axis',(-0.999999999996567,2.62032228309351E-6,5.75848112614908E-13));
#38707=DIRECTION('center_axis',(-5.57179392097266E-15,1.12027918221652E-15,
-1.));
#38708=DIRECTION('ref_axis',(-1.,5.00596043934455E-16,5.57179392097267E-15));
#38709=DIRECTION('center_axis',(-5.57179392097266E-15,1.12027918221652E-15,
-1.));
#38710=DIRECTION('ref_axis',(-1.,5.00596043934455E-16,5.57179392097267E-15));
#38711=DIRECTION('center_axis',(-3.71898927649643E-15,-0.803522087077111,
-0.59527494116521));
#38712=DIRECTION('ref_axis',(-0.999999999999775,-3.9973451068302E-7,5.395750598724E-7));
#38713=DIRECTION('center_axis',(-0.779319883704293,-3.11871947293856E-16,
0.626626299211202));
#38714=DIRECTION('ref_axis',(-5.00596043934461E-16,-1.,-1.12027918221652E-15));
#38715=DIRECTION('center_axis',(0.779319883704293,3.11871947293856E-16,
-0.626626299211202));
#38716=DIRECTION('ref_axis',(0.54267429379633,-0.5,0.674910816962252));
#38717=DIRECTION('',(-0.779320120961903,2.7427056598253E-7,0.62662600413951));
#38718=DIRECTION('center_axis',(0.618735717390635,0.707106781186537,-0.342295357878415));
#38719=DIRECTION('ref_axis',(0.618735717390611,-0.707106781186558,-0.342295357878414));
#38720=DIRECTION('center_axis',(0.24472801409699,0.862800334966154,0.442361595415376));
#38721=DIRECTION('ref_axis',(0.542687498153732,-0.499966900858982,0.674924719797037));
#38722=DIRECTION('center_axis',(0.484078737448991,-1.22259956840877E-15,
0.875024443058473));
#38723=DIRECTION('ref_axis',(-5.00596043934461E-16,-1.,-1.12027918221652E-15));
#38724=DIRECTION('center_axis',(5.00596043934461E-16,1.,1.12027918221652E-15));
#38725=DIRECTION('ref_axis',(0.00546733966186705,1.08624916607697E-15,-0.999985053986819));
#38726=DIRECTION('center_axis',(0.560028488398899,-1.2084694931618E-15,
0.828473350314689));
#38727=DIRECTION('ref_axis',(7.44048982333015E-12,-1.,-5.03105469429634E-12));
#38728=DIRECTION('center_axis',(5.00596043934461E-16,1.,1.12027918221652E-15));
#38729=DIRECTION('ref_axis',(0.00546733966186705,1.08624916607697E-15,-0.999985053986819));
#38730=DIRECTION('center_axis',(-0.779319883704293,-3.11871947293856E-16,
0.626626299211202));
#38731=DIRECTION('ref_axis',(5.00596043934461E-16,1.,1.12027918221652E-15));
#38732=DIRECTION('center_axis',(0.779319883704293,3.11871947293856E-16,
-0.626626299211202));
#38733=DIRECTION('ref_axis',(-0.54267429379633,0.5,-0.674910816962252));
#38734=DIRECTION('center_axis',(0.478187048237211,0.522807970064414,-0.705697508381112));
#38735=DIRECTION('ref_axis',(-0.878258018408137,0.284654389439121,-0.384232653056521));
#38736=DIRECTION('center_axis',(-1.,5.00596043934455E-16,5.57179392097267E-15));
#38737=DIRECTION('ref_axis',(5.57179392097266E-15,-1.12027918221652E-15,
1.));
#38738=DIRECTION('center_axis',(-1.,5.00596043934455E-16,5.57179392097267E-15));
#38739=DIRECTION('ref_axis',(5.57179392097266E-15,-1.12027918221652E-15,
1.));
#38740=DIRECTION('center_axis',(0.,0.707106781186545,-0.70710678118655));
#38741=DIRECTION('ref_axis',(0.,0.707106781186545,0.70710678118655));
#38742=DIRECTION('center_axis',(5.00596043934461E-16,1.,1.12027918221652E-15));
#38743=DIRECTION('ref_axis',(0.00546733966186688,1.05265590482978E-15,-0.999985053986819));
#38744=DIRECTION('center_axis',(5.00596043934461E-16,1.,1.12027918221652E-15));
#38745=DIRECTION('ref_axis',(-5.57179392097267E-15,1.12027918221652E-15,
-1.));
#38746=DIRECTION('center_axis',(0.999985053986819,-5.06713508824686E-16,
0.00546733966186613));
#38747=DIRECTION('ref_axis',(-0.00546733966186613,-1.12784561231762E-15,
0.999985053986819));
#38748=DIRECTION('center_axis',(5.00596043934461E-16,1.,1.12027918221652E-15));
#38749=DIRECTION('ref_axis',(-5.57179392097267E-15,1.12027918221652E-15,
-1.));
#38750=DIRECTION('center_axis',(-5.00596043934461E-16,-1.,-1.12027918221652E-15));
#38751=DIRECTION('ref_axis',(-5.57179392097266E-15,1.12027918221652E-15,
-1.));
#38752=DIRECTION('center_axis',(5.00596043934461E-16,1.,1.12027918221652E-15));
#38753=DIRECTION('ref_axis',(-0.0102648972912855,1.04414803197664E-15,-0.999947314553922));
#38754=DIRECTION('center_axis',(5.00596043934461E-16,1.,1.12027918221652E-15));
#38755=DIRECTION('ref_axis',(5.57179392097266E-15,-1.12027918221652E-15,
1.));
#38756=DIRECTION('center_axis',(5.00596043934461E-16,1.,1.12027918221652E-15));
#38757=DIRECTION('ref_axis',(5.57179392097266E-15,-1.12027918221652E-15,
1.));
#38758=DIRECTION('center_axis',(0.999947314553922,-4.89070119065563E-16,
-0.0102648972912858));
#38759=DIRECTION('ref_axis',(0.0102648972912858,-1.08765419997566E-15,0.999947314553921));
#38760=DIRECTION('center_axis',(5.00596043934461E-16,1.,1.12027918221652E-15));
#38761=DIRECTION('ref_axis',(-5.57179392097266E-15,1.12027918221652E-15,
-1.));
#38762=DIRECTION('center_axis',(-5.00596043934461E-16,-1.,-1.12027918221652E-15));
#38763=DIRECTION('ref_axis',(5.57179392097266E-15,-1.12027918221652E-15,
1.));
#38764=DIRECTION('',(-5.00596043934461E-16,-1.,-1.12027918221652E-15));
#38765=DIRECTION('center_axis',(5.00596043934461E-16,1.,1.12027918221652E-15));
#38766=DIRECTION('ref_axis',(-5.57179392097267E-15,1.12027918221652E-15,
-1.));
#38767=DIRECTION('center_axis',(-5.00596043934461E-16,-1.,-1.12027918221652E-15));
#38768=DIRECTION('ref_axis',(5.57179392097266E-15,-1.12027918221652E-15,
1.));
#38769=DIRECTION('center_axis',(5.00596043934461E-16,1.,1.12027918221652E-15));
#38770=DIRECTION('ref_axis',(-5.57179392097266E-15,1.12027918221652E-15,
-1.));
#38771=DIRECTION('center_axis',(-5.00596043934461E-16,-1.,-1.12027918221652E-15));
#38772=DIRECTION('ref_axis',(5.57179392097266E-15,-1.12027918221652E-15,
1.));
#38773=DIRECTION('',(5.00596043934461E-16,1.,1.12027918221652E-15));
#38774=DIRECTION('center_axis',(5.00596043934461E-16,1.,1.12027918221652E-15));
#38775=DIRECTION('ref_axis',(-5.57179392097267E-15,1.12027918221652E-15,
-1.));
#38776=DIRECTION('center_axis',(-5.00596043934461E-16,-1.,-1.12027918221652E-15));
#38777=DIRECTION('ref_axis',(5.57179392097266E-15,-1.12027918221652E-15,
1.));
#38778=DIRECTION('center_axis',(5.00596043934461E-16,1.,1.12027918221652E-15));
#38779=DIRECTION('ref_axis',(-5.57179392097266E-15,1.12027918221652E-15,
-1.));
#38780=DIRECTION('center_axis',(-5.00596043934461E-16,-1.,-1.12027918221652E-15));
#38781=DIRECTION('ref_axis',(5.57179392097266E-15,-1.12027918221652E-15,
1.));
#38782=DIRECTION('',(-5.00596043934461E-16,-1.,-1.12027918221652E-15));
#38783=DIRECTION('center_axis',(5.00596043934461E-16,1.,1.12027918221652E-15));
#38784=DIRECTION('ref_axis',(-5.57179392097267E-15,1.12027918221652E-15,
-1.));
#38785=DIRECTION('center_axis',(-5.00596043934461E-16,-1.,-1.12027918221652E-15));
#38786=DIRECTION('ref_axis',(5.57179392097266E-15,-1.12027918221652E-15,
1.));
#38787=DIRECTION('center_axis',(5.00596043934461E-16,1.,1.12027918221652E-15));
#38788=DIRECTION('ref_axis',(-5.57179392097266E-15,1.12027918221652E-15,
-1.));
#38789=DIRECTION('center_axis',(-5.00596043934461E-16,-1.,-1.12027918221652E-15));
#38790=DIRECTION('ref_axis',(5.57179392097266E-15,-1.12027918221652E-15,
1.));
#38791=DIRECTION('',(5.00596043934461E-16,1.,1.12027918221652E-15));
#38792=DIRECTION('center_axis',(5.00596043934461E-16,1.,1.12027918221652E-15));
#38793=DIRECTION('ref_axis',(-5.57179392097267E-15,1.12027918221652E-15,
-1.));
#38794=DIRECTION('center_axis',(-5.00596043934461E-16,-1.,-1.12027918221652E-15));
#38795=DIRECTION('ref_axis',(5.57179392097266E-15,-1.12027918221652E-15,
1.));
#38796=DIRECTION('center_axis',(5.00596043934461E-16,1.,1.12027918221652E-15));
#38797=DIRECTION('ref_axis',(-5.57179392097266E-15,1.12027918221652E-15,
-1.));
#38798=DIRECTION('center_axis',(-5.00596043934461E-16,-1.,-1.12027918221652E-15));
#38799=DIRECTION('ref_axis',(5.57179392097266E-15,-1.12027918221652E-15,
1.));
#38800=DIRECTION('',(-5.00596043934461E-16,-1.,-1.12027918221652E-15));
#38801=DIRECTION('center_axis',(5.00596043934461E-16,1.,1.12027918221652E-15));
#38802=DIRECTION('ref_axis',(-5.57179392097267E-15,1.12027918221652E-15,
-1.));
#38803=DIRECTION('center_axis',(-5.00596043934461E-16,-1.,-1.12027918221652E-15));
#38804=DIRECTION('ref_axis',(5.57179392097266E-15,-1.12027918221652E-15,
1.));
#38805=DIRECTION('center_axis',(5.00596043934461E-16,1.,1.12027918221652E-15));
#38806=DIRECTION('ref_axis',(-5.57179392097266E-15,1.12027918221652E-15,
-1.));
#38807=DIRECTION('center_axis',(-5.00596043934461E-16,-1.,-1.12027918221652E-15));
#38808=DIRECTION('ref_axis',(5.57179392097266E-15,-1.12027918221652E-15,
1.));
#38809=DIRECTION('',(5.00596043934461E-16,1.,1.12027918221652E-15));
#38810=DIRECTION('center_axis',(5.00596043934461E-16,1.,1.12027918221652E-15));
#38811=DIRECTION('ref_axis',(-5.57179392097267E-15,1.12027918221652E-15,
-1.));
#38812=DIRECTION('center_axis',(-5.00596043934461E-16,-1.,-1.12027918221652E-15));
#38813=DIRECTION('ref_axis',(-1.,5.00596043934455E-16,5.57179392097267E-15));
#38814=DIRECTION('center_axis',(5.00596043934461E-16,1.,1.12027918221652E-15));
#38815=DIRECTION('ref_axis',(-5.57179392097266E-15,1.12027918221652E-15,
-1.));
#38816=DIRECTION('center_axis',(5.00596043934461E-16,1.,1.12027918221652E-15));
#38817=DIRECTION('ref_axis',(1.,-5.00596043934455E-16,-5.57179392097267E-15));
#38818=DIRECTION('',(5.00596043934461E-16,1.,1.12027918221652E-15));
#38819=DIRECTION('center_axis',(-5.00596043934461E-16,-1.,-1.12027918221652E-15));
#38820=DIRECTION('ref_axis',(-1.,5.00596043934455E-16,5.57179392097267E-15));
#38821=DIRECTION('center_axis',(5.00596043934461E-16,1.,1.12027918221652E-15));
#38822=DIRECTION('ref_axis',(-1.,5.00596043934455E-16,5.57179392097267E-15));
#38823=DIRECTION('',(5.57179392097266E-15,-1.12027918221652E-15,1.));
#38824=DIRECTION('center_axis',(5.00596043934461E-16,1.,1.12027918221652E-15));
#38825=DIRECTION('ref_axis',(-5.57179392097266E-15,1.12027918221652E-15,
-1.));
#38826=DIRECTION('',(-1.,5.00596043934455E-16,5.57179392097266E-15));
#38827=DIRECTION('center_axis',(5.00596043934461E-16,1.,1.12027918221652E-15));
#38828=DIRECTION('ref_axis',(1.,-5.00596043934455E-16,-5.57179392097267E-15));
#38829=DIRECTION('',(-5.57179392097266E-15,1.12027918221652E-15,-1.));
#38830=DIRECTION('center_axis',(5.00596043934461E-16,1.,1.12027918221652E-15));
#38831=DIRECTION('ref_axis',(5.57179392097266E-15,-1.12027918221652E-15,
1.));
#38832=DIRECTION('',(1.,-5.00596043934455E-16,-5.57179392097266E-15));
#38833=DIRECTION('center_axis',(-5.00596043934461E-16,-1.,-1.12027918221652E-15));
#38834=DIRECTION('ref_axis',(-1.,5.00596043934455E-16,5.57179392097267E-15));
#38835=DIRECTION('',(5.00596043934461E-16,1.,1.12027918221652E-15));
#38836=DIRECTION('',(5.00596043934461E-16,1.,1.12027918221652E-15));
#38837=DIRECTION('center_axis',(-5.57179392097266E-15,1.12027918221652E-15,
-1.));
#38838=DIRECTION('ref_axis',(1.,-5.00596043934455E-16,-5.57179392097267E-15));
#38839=DIRECTION('',(5.00596043934461E-16,1.,1.12027918221652E-15));
#38840=DIRECTION('center_axis',(-5.00596043934461E-16,-1.,-1.12027918221652E-15));
#38841=DIRECTION('ref_axis',(-1.,5.00596043934455E-16,5.57179392097267E-15));
#38842=DIRECTION('',(5.00596043934461E-16,1.,1.12027918221652E-15));
#38843=DIRECTION('center_axis',(-1.,5.00596043934455E-16,5.57179392097267E-15));
#38844=DIRECTION('ref_axis',(-5.57179392097267E-15,1.12027918221652E-15,
-1.));
#38845=DIRECTION('',(5.00596043934461E-16,1.,1.12027918221652E-15));
#38846=DIRECTION('center_axis',(-5.00596043934461E-16,-1.,-1.12027918221652E-15));
#38847=DIRECTION('ref_axis',(-1.,5.00596043934455E-16,5.57179392097267E-15));
#38848=DIRECTION('',(5.00596043934461E-16,1.,1.12027918221652E-15));
#38849=DIRECTION('center_axis',(5.57179392097266E-15,-1.12027918221652E-15,
1.));
#38850=DIRECTION('ref_axis',(-1.,5.00596043934455E-16,5.57179392097267E-15));
#38851=DIRECTION('',(5.00596043934461E-16,1.,1.12027918221652E-15));
#38852=DIRECTION('center_axis',(-5.00596043934461E-16,-1.,-1.12027918221652E-15));
#38853=DIRECTION('ref_axis',(-1.,5.00596043934455E-16,5.57179392097267E-15));
#38854=DIRECTION('',(5.00596043934461E-16,1.,1.12027918221652E-15));
#38855=DIRECTION('center_axis',(1.,-5.00596043934455E-16,-5.57179392097267E-15));
#38856=DIRECTION('ref_axis',(5.57179392097267E-15,-1.12027918221652E-15,
1.));
#38857=DIRECTION('axis',(0.,0.,1.));
#38858=DIRECTION('refdir',(1.,0.,0.));
#38859=DIRECTION('center_axis',(-5.00596043934461E-16,-1.,-1.12083973155589E-15));
#38860=DIRECTION('ref_axis',(1.,0.,-9.16829336464647E-15));
#38861=DIRECTION('center_axis',(5.00596043934461E-16,1.,1.12083973155589E-15));
#38862=DIRECTION('ref_axis',(-5.58323629842488E-15,1.12083973155589E-15,
-1.));
#38863=DIRECTION('center_axis',(5.00596043934461E-16,1.,1.12083973155589E-15));
#38864=DIRECTION('ref_axis',(-5.58323629842488E-15,1.12083973155589E-15,
-1.));
#38865=DIRECTION('center_axis',(0.,-1.12083973155589E-15,1.));
#38866=DIRECTION('ref_axis',(-1.,0.,0.));
#38867=DIRECTION('center_axis',(-5.00596043934461E-16,-1.,-1.12083973155589E-15));
#38868=DIRECTION('ref_axis',(-5.58323629842488E-15,1.12083973155589E-15,
-1.));
#38869=DIRECTION('center_axis',(-5.00596043934461E-16,-1.,-1.12083973155589E-15));
#38870=DIRECTION('ref_axis',(5.46077161851015E-15,-1.12083973155589E-15,
1.));
#38871=DIRECTION('center_axis',(-5.00596043934461E-16,-1.,-1.12083973155589E-15));
#38872=DIRECTION('ref_axis',(-5.46077161851015E-15,1.12083973155589E-15,
-1.));
#38873=DIRECTION('center_axis',(-5.00596043934461E-16,-1.,-1.12083973155589E-15));
#38874=DIRECTION('ref_axis',(-5.46077161851015E-15,1.12083973155589E-15,
-1.));
#38875=DIRECTION('',(5.00596043934461E-16,1.,1.12083973155589E-15));
#38876=DIRECTION('center_axis',(-5.00596043934461E-16,-1.,-1.12083973155589E-15));
#38877=DIRECTION('ref_axis',(1.,-5.00596043934455E-16,-5.46077161851015E-15));
#38878=DIRECTION('center_axis',(-5.00596043934461E-16,-1.,-1.12083973155589E-15));
#38879=DIRECTION('ref_axis',(5.46077161851015E-15,-1.12083973155589E-15,
1.));
#38880=DIRECTION('center_axis',(5.00596043934461E-16,1.,1.12083973155589E-15));
#38881=DIRECTION('ref_axis',(-5.46077161851015E-15,1.12083973155589E-15,
-1.));
#38882=DIRECTION('',(-4.30191910488433E-15,-0.707106781186548,-0.707106781186547));
#38883=DIRECTION('center_axis',(5.00596043934461E-16,1.,1.12083973155589E-15));
#38884=DIRECTION('ref_axis',(-5.46077161851015E-15,1.12083973155589E-15,
-1.));
#38885=DIRECTION('center_axis',(-5.00596043934461E-16,-1.,-1.12083973155589E-15));
#38886=DIRECTION('ref_axis',(1.,-5.00596043934455E-16,-5.46077161851015E-15));
#38887=DIRECTION('center_axis',(-5.00596043934461E-16,-1.,-1.12083973155589E-15));
#38888=DIRECTION('ref_axis',(1.,-7.89491928622333E-16,-6.31593542897867E-15));
#38889=DIRECTION('center_axis',(5.00596043934461E-16,1.,1.12083973155589E-15));
#38890=DIRECTION('ref_axis',(-5.58323629842488E-15,1.12083973155589E-15,
-1.));
#38891=DIRECTION('center_axis',(5.00596043934461E-16,1.,1.12083973155589E-15));
#38892=DIRECTION('ref_axis',(-5.58323629842488E-15,1.12083973155589E-15,
-1.));
#38893=DIRECTION('center_axis',(-7.89491928622335E-15,1.1208397315559E-15,
-1.));
#38894=DIRECTION('ref_axis',(-1.,9.86864910777919E-16,7.89491928622335E-15));
#38895=DIRECTION('center_axis',(-5.00596043934461E-16,-1.,-1.12083973155589E-15));
#38896=DIRECTION('ref_axis',(-5.58323629842488E-15,1.12083973155589E-15,
-1.));
#38897=DIRECTION('center_axis',(5.00596043934461E-16,1.,1.12083973155589E-15));
#38898=DIRECTION('ref_axis',(-1.,5.00596043934455E-16,5.46077161851015E-15));
#38899=DIRECTION('',(-1.,5.00596043934454E-16,6.22995669306358E-15));
#38900=DIRECTION('',(-0.500000000000005,1.22097370306556E-15,-0.866025403784436));
#38901=DIRECTION('',(0.499999999999995,7.20377659131108E-16,-0.866025403784441));
#38902=DIRECTION('',(1.,-5.00596043934455E-16,-5.55691975282933E-15));
#38903=DIRECTION('',(0.500000000000005,-1.22097370306556E-15,0.866025403784436));
#38904=DIRECTION('',(-0.499999999999995,-7.20377659131108E-16,0.866025403784441));
#38905=DIRECTION('center_axis',(-5.00596043934461E-16,-1.,-1.12083973155589E-15));
#38906=DIRECTION('ref_axis',(5.46077161851015E-15,-1.12083973155589E-15,
1.));
#38907=DIRECTION('',(5.00596043934461E-16,1.,1.12083973155589E-15));
#38908=DIRECTION('center_axis',(0.866025403784436,1.26890974696718E-16,
-0.500000000000005));
#38909=DIRECTION('ref_axis',(5.00353318950476E-16,1.,1.12041931955136E-15));
#38910=DIRECTION('',(5.00596043934461E-16,1.,1.12083973155589E-15));
#38911=DIRECTION('',(5.00596043934461E-16,1.,1.12083973155589E-15));
#38912=DIRECTION('center_axis',(0.866025403784442,-9.93948756859176E-16,
0.499999999999995));
#38913=DIRECTION('ref_axis',(5.00838768918447E-16,1.,1.12041931955136E-15));
#38914=DIRECTION('',(5.00596043934461E-16,1.,1.12083973155589E-15));
#38915=DIRECTION('center_axis',(6.22995669306358E-15,-1.1208397315559E-15,
1.));
#38916=DIRECTION('ref_axis',(-1.,5.00596043934454E-16,6.22995669306358E-15));
#38917=DIRECTION('',(5.00596043934461E-16,1.,1.12083973155589E-15));
#38918=DIRECTION('center_axis',(-0.866025403784436,-1.26890974696719E-16,
0.500000000000005));
#38919=DIRECTION('ref_axis',(-5.00353318950476E-16,-1.,-1.12041931955136E-15));
#38920=DIRECTION('',(-5.00596043934461E-16,-1.,-1.12083973155589E-15));
#38921=DIRECTION('center_axis',(-5.55691975282933E-15,1.12083973155589E-15,
-1.));
#38922=DIRECTION('ref_axis',(1.,-5.00596043934455E-16,-5.55691975282933E-15));
#38923=DIRECTION('',(5.00596043934461E-16,1.,1.12083973155589E-15));
#38924=DIRECTION('center_axis',(-0.866025403784442,9.93948756859176E-16,
-0.499999999999995));
#38925=DIRECTION('ref_axis',(-5.00838768918447E-16,-1.,-1.12041931955136E-15));
#38926=DIRECTION('center_axis',(5.00596043934461E-16,1.,1.12083973155589E-15));
#38927=DIRECTION('ref_axis',(5.46077161851015E-15,-1.12083973155589E-15,
1.));
#38928=DIRECTION('',(-4.58492644780011E-15,0.500000000000001,-0.866025403784438));
#38929=DIRECTION('axis',(0.,0.,1.));
#38930=DIRECTION('refdir',(1.,0.,0.));
#38931=DIRECTION('center_axis',(-1.,5.00264601743691E-16,3.82282413363175E-15));
#38932=DIRECTION('ref_axis',(0.,0.,1.));
#38933=DIRECTION('center_axis',(1.,-5.00264601743691E-16,-3.82282413363175E-15));
#38934=DIRECTION('ref_axis',(-5.00264601743696E-16,-1.,-1.24274386213125E-15));
#38935=DIRECTION('center_axis',(1.,-5.00264601743691E-16,-3.82282413363175E-15));
#38936=DIRECTION('ref_axis',(-5.00264601743696E-16,-1.,-1.24274386213125E-15));
#38937=DIRECTION('center_axis',(5.00264601743691E-16,1.,0.));
#38938=DIRECTION('ref_axis',(0.,0.,-1.));
#38939=DIRECTION('center_axis',(-1.,5.00264601743691E-16,3.82282413363175E-15));
#38940=DIRECTION('ref_axis',(-5.00264601743696E-16,-1.,-1.24274386213126E-15));
#38941=DIRECTION('center_axis',(-1.,5.00264601743691E-16,3.82282413363175E-15));
#38942=DIRECTION('ref_axis',(5.00264601743695E-16,1.,1.12027918221652E-15));
#38943=DIRECTION('center_axis',(-1.,5.00264601743691E-16,3.82282413363175E-15));
#38944=DIRECTION('ref_axis',(-5.00264601743695E-16,-1.,-1.12027918221652E-15));
#38945=DIRECTION('center_axis',(-1.,5.00264601743691E-16,3.82282413363175E-15));
#38946=DIRECTION('ref_axis',(-5.00264601743695E-16,-1.,-1.12027918221652E-15));
#38947=DIRECTION('',(1.,-5.00264601743691E-16,-3.82282413363175E-15));
#38948=DIRECTION('center_axis',(-1.,5.00264601743691E-16,3.82282413363175E-15));
#38949=DIRECTION('ref_axis',(3.82282413363175E-15,-1.12027918221652E-15,
1.));
#38950=DIRECTION('center_axis',(-1.,5.00264601743691E-16,3.82282413363175E-15));
#38951=DIRECTION('ref_axis',(5.00264601743695E-16,1.,1.12027918221652E-15));
#38952=DIRECTION('center_axis',(1.,-5.00264601743691E-16,-3.82282413363175E-15));
#38953=DIRECTION('ref_axis',(-5.00264601743695E-16,-1.,-1.12027918221652E-15));
#38954=DIRECTION('',(-0.707106781186548,-0.707106781186547,1.82439225598363E-15));
#38955=DIRECTION('center_axis',(1.,-5.00264601743691E-16,-3.82282413363175E-15));
#38956=DIRECTION('ref_axis',(-5.00264601743695E-16,-1.,-1.12027918221652E-15));
#38957=DIRECTION('center_axis',(-1.,5.00264601743691E-16,3.82282413363175E-15));
#38958=DIRECTION('ref_axis',(3.82282413363175E-15,-1.12027918221652E-15,
1.));
#38959=DIRECTION('center_axis',(-1.,5.00264601743691E-16,3.82282413363175E-15));
#38960=DIRECTION('ref_axis',(0.,-1.77635683940025E-15,1.));
#38961=DIRECTION('center_axis',(1.,-5.00264601743691E-16,-3.82282413363175E-15));
#38962=DIRECTION('ref_axis',(-5.00264601743696E-16,-1.,-1.24274386213126E-15));
#38963=DIRECTION('center_axis',(1.,-5.00264601743691E-16,-3.82282413363175E-15));
#38964=DIRECTION('ref_axis',(-5.00264601743696E-16,-1.,-1.24274386213126E-15));
#38965=DIRECTION('center_axis',(-5.00264601743691E-16,-1.,0.));
#38966=DIRECTION('ref_axis',(0.,0.,-1.));
#38967=DIRECTION('center_axis',(-1.,5.00264601743691E-16,3.82282413363175E-15));
#38968=DIRECTION('ref_axis',(-5.00264601743696E-16,-1.,-1.24274386213125E-15));
#38969=DIRECTION('center_axis',(1.,-5.00264601743691E-16,-3.82282413363175E-15));
#38970=DIRECTION('ref_axis',(-3.82282413363175E-15,1.12027918221652E-15,
-1.));
#38971=DIRECTION('',(-3.82282413363175E-15,1.60101985381241E-15,-1.));
#38972=DIRECTION('',(-2.34465392054002E-15,-0.866025403784438,-0.500000000000001));
#38973=DIRECTION('',(1.47817021309173E-15,-0.866025403784439,0.499999999999999));
#38974=DIRECTION('',(3.82282413363175E-15,-1.2404643501155E-15,1.));
#38975=DIRECTION('',(2.34465392054002E-15,0.866025403784438,0.500000000000001));
#38976=DIRECTION('',(-1.47817021309173E-15,0.866025403784439,-0.499999999999999));
#38977=DIRECTION('center_axis',(-1.,5.00264601743691E-16,3.82282413363175E-15));
#38978=DIRECTION('ref_axis',(5.00264601743695E-16,1.,1.12027918221652E-15));
#38979=DIRECTION('',(1.,-5.00264601743691E-16,-3.82282413363175E-15));
#38980=DIRECTION('center_axis',(3.06053051305348E-15,-0.500000000000001,
0.866025403784438));
#38981=DIRECTION('ref_axis',(1.,-5.00513183386765E-16,-3.82296765231029E-15));
#38982=DIRECTION('',(1.,-5.00264601743691E-16,-3.82282413363175E-15));
#38983=DIRECTION('',(1.,-5.00264601743691E-16,-3.82282413363175E-15));
#38984=DIRECTION('center_axis',(3.56079511479718E-15,0.499999999999999,
0.866025403784439));
#38985=DIRECTION('ref_axis',(1.,-5.00513183386765E-16,-3.8226806149532E-15));
#38986=DIRECTION('',(1.,-5.00264601743691E-16,-3.82282413363175E-15));
#38987=DIRECTION('center_axis',(5.00264601743697E-16,1.,1.60101985381241E-15));
#38988=DIRECTION('ref_axis',(-3.82282413363175E-15,1.60101985381241E-15,
-1.));
#38989=DIRECTION('',(1.,-5.00264601743691E-16,-3.82282413363175E-15));
#38990=DIRECTION('center_axis',(-3.06053051305348E-15,0.500000000000001,
-0.866025403784438));
#38991=DIRECTION('ref_axis',(-1.,5.00513183386765E-16,3.82296765231029E-15));
#38992=DIRECTION('',(-1.,5.00264601743691E-16,3.82282413363175E-15));
#38993=DIRECTION('center_axis',(-5.00264601743696E-16,-1.,-1.24046435011549E-15));
#38994=DIRECTION('ref_axis',(3.82282413363175E-15,-1.2404643501155E-15,
1.));
#38995=DIRECTION('',(1.,-5.00264601743691E-16,-3.82282413363175E-15));
#38996=DIRECTION('center_axis',(-3.56079511479718E-15,-0.499999999999999,
-0.866025403784439));
#38997=DIRECTION('ref_axis',(-1.,5.00513183386765E-16,3.8226806149532E-15));
#38998=DIRECTION('center_axis',(1.,-5.00264601743691E-16,-3.82282413363175E-15));
#38999=DIRECTION('ref_axis',(5.00264601743695E-16,1.,1.12027918221652E-15));
#39000=DIRECTION('',(0.5,-0.866025403784439,-2.98765982181873E-15));
#39001=DIRECTION('axis',(0.,0.,1.));
#39002=DIRECTION('refdir',(1.,0.,0.));
#39003=DIRECTION('center_axis',(1.14962333747911E-15,1.,1.12055937046026E-15));
#39004=DIRECTION('ref_axis',(1.,0.,0.));
#39005=DIRECTION('center_axis',(-1.14962333747911E-15,-1.,-1.12055937046026E-15));
#39006=DIRECTION('ref_axis',(5.33830693859541E-15,-1.12055937046026E-15,
1.));
#39007=DIRECTION('center_axis',(-1.14962333747911E-15,-1.,-1.12055937046026E-15));
#39008=DIRECTION('ref_axis',(5.33830693859541E-15,-1.12055937046026E-15,
1.));
#39009=DIRECTION('center_axis',(0.,1.12055937046026E-15,-1.));
#39010=DIRECTION('ref_axis',(-1.,0.,0.));
#39011=DIRECTION('center_axis',(1.14962333747911E-15,1.,1.12055937046026E-15));
#39012=DIRECTION('ref_axis',(5.33830693859542E-15,-1.12055937046026E-15,
1.));
#39013=DIRECTION('center_axis',(1.14962333747911E-15,1.,1.12055937046026E-15));
#39014=DIRECTION('ref_axis',(-5.46077161851015E-15,1.12055937046026E-15,
-1.));
#39015=DIRECTION('center_axis',(1.14962333747911E-15,1.,1.12055937046026E-15));
#39016=DIRECTION('ref_axis',(5.46077161851015E-15,-1.12055937046026E-15,
1.));
#39017=DIRECTION('center_axis',(1.14962333747911E-15,1.,1.12055937046026E-15));
#39018=DIRECTION('ref_axis',(5.46077161851015E-15,-1.12055937046026E-15,
1.));
#39019=DIRECTION('',(-1.14962333747911E-15,-1.,-1.12055937046026E-15));
#39020=DIRECTION('center_axis',(1.14962333747911E-15,1.,1.12055937046026E-15));
#39021=DIRECTION('ref_axis',(1.,-1.1496233374791E-15,-5.46077161851015E-15));
#39022=DIRECTION('center_axis',(1.14962333747911E-15,1.,1.12055937046026E-15));
#39023=DIRECTION('ref_axis',(-5.46077161851015E-15,1.12055937046026E-15,
-1.));
#39024=DIRECTION('center_axis',(-1.14962333747911E-15,-1.,-1.12055937046026E-15));
#39025=DIRECTION('ref_axis',(5.46077161851015E-15,-1.12055937046026E-15,
1.));
#39026=DIRECTION('',(4.5876594940778E-15,0.707106781186547,0.707106781186548));
#39027=DIRECTION('center_axis',(-1.14962333747911E-15,-1.,-1.12055937046026E-15));
#39028=DIRECTION('ref_axis',(5.46077161851015E-15,-1.12055937046026E-15,
1.));
#39029=DIRECTION('center_axis',(1.14962333747911E-15,1.,1.12055937046026E-15));
#39030=DIRECTION('ref_axis',(1.,-1.1496233374791E-15,-5.46077161851015E-15));
#39031=DIRECTION('center_axis',(1.14962333747911E-15,1.,1.12055937046026E-15));
#39032=DIRECTION('ref_axis',(1.,0.,-7.105427357601E-15));
#39033=DIRECTION('center_axis',(-1.14962333747911E-15,-1.,-1.12055937046026E-15));
#39034=DIRECTION('ref_axis',(5.33830693859541E-15,-1.12055937046026E-15,
1.));
#39035=DIRECTION('center_axis',(-1.14962333747911E-15,-1.,-1.12055937046026E-15));
#39036=DIRECTION('ref_axis',(5.33830693859541E-15,-1.12055937046026E-15,
1.));
#39037=DIRECTION('center_axis',(8.88178419700128E-15,-1.12055937046027E-15,
1.));
#39038=DIRECTION('ref_axis',(-1.,0.,8.88178419700128E-15));
#39039=DIRECTION('center_axis',(1.14962333747911E-15,1.,1.12055937046026E-15));
#39040=DIRECTION('ref_axis',(5.33830693859541E-15,-1.12055937046026E-15,
1.));
#39041=DIRECTION('center_axis',(-1.14962333747911E-15,-1.,-1.12055937046026E-15));
#39042=DIRECTION('ref_axis',(-1.,1.1496233374791E-15,5.46077161851015E-15));
#39043=DIRECTION('',(-1.,1.1496233374791E-15,4.98003094691426E-15));
#39044=DIRECTION('',(-0.499999999999995,-3.95621212527735E-16,0.866025403784441));
#39045=DIRECTION('',(0.500000000000005,-1.54524455000684E-15,0.866025403784436));
#39046=DIRECTION('',(1.,-1.1496233374791E-15,-5.34058645061118E-15));
#39047=DIRECTION('',(0.499999999999995,3.95621212527734E-16,-0.866025403784441));
#39048=DIRECTION('',(-0.500000000000005,1.54524455000684E-15,-0.866025403784436));
#39049=DIRECTION('center_axis',(1.14962333747911E-15,1.,1.12055937046026E-15));
#39050=DIRECTION('ref_axis',(-5.46077161851015E-15,1.12055937046026E-15,
-1.));
#39051=DIRECTION('',(-1.14962333747911E-15,-1.,-1.12055937046026E-15));
#39052=DIRECTION('center_axis',(0.866025403784442,-1.55588270027048E-15,
0.499999999999995));
#39053=DIRECTION('ref_axis',(-1.14974466254757E-15,-1.,-1.12034922927745E-15));
#39054=DIRECTION('',(-1.14962333747911E-15,-1.,-1.12055937046026E-15));
#39055=DIRECTION('',(-1.14962333747911E-15,-1.,-1.12055937046026E-15));
#39056=DIRECTION('center_axis',(0.866025403784436,-4.35323329810222E-16,
-0.500000000000005));
#39057=DIRECTION('ref_axis',(-1.14950201241065E-15,-1.,-1.12034922927745E-15));
#39058=DIRECTION('',(-1.14962333747911E-15,-1.,-1.12055937046026E-15));
#39059=DIRECTION('center_axis',(-4.98003094691426E-15,1.12055937046026E-15,
-1.));
#39060=DIRECTION('ref_axis',(-1.,1.1496233374791E-15,4.98003094691426E-15));
#39061=DIRECTION('',(-1.14962333747911E-15,-1.,-1.12055937046026E-15));
#39062=DIRECTION('center_axis',(-0.866025403784442,1.55588270027048E-15,
-0.499999999999995));
#39063=DIRECTION('ref_axis',(1.14974466254757E-15,1.,1.12034922927745E-15));
#39064=DIRECTION('',(1.14962333747911E-15,1.,1.12055937046026E-15));
#39065=DIRECTION('center_axis',(5.34058645061118E-15,-1.12055937046026E-15,
1.));
#39066=DIRECTION('ref_axis',(1.,-1.1496233374791E-15,-5.34058645061118E-15));
#39067=DIRECTION('',(-1.14962333747911E-15,-1.,-1.12055937046026E-15));
#39068=DIRECTION('center_axis',(-0.866025403784436,4.35323329810222E-16,
0.500000000000005));
#39069=DIRECTION('ref_axis',(1.14950201241065E-15,1.,1.12034922927745E-15));
#39070=DIRECTION('center_axis',(-1.14962333747911E-15,-1.,-1.12055937046026E-15));
#39071=DIRECTION('ref_axis',(-5.46077161851015E-15,1.12055937046026E-15,
-1.));
#39072=DIRECTION('',(4.04829775328281E-15,-0.500000000000001,0.866025403784438));
#39073=DIRECTION('axis',(0.,0.,1.));
#39074=DIRECTION('refdir',(1.,0.,0.));
#39075=DIRECTION('center_axis',(-1.30103752480477E-16,7.77119338241477E-16,
-1.));
#39076=DIRECTION('ref_axis',(0.,-1.,0.));
#39077=DIRECTION('center_axis',(1.30103752480477E-16,-7.77119338241477E-16,
1.));
#39078=DIRECTION('ref_axis',(1.,1.22464679914733E-16,-1.30103752480477E-16));
#39079=DIRECTION('center_axis',(1.30103752480477E-16,-7.77119338241477E-16,
1.));
#39080=DIRECTION('ref_axis',(1.,1.22464679914733E-16,-1.30103752480477E-16));
#39081=DIRECTION('center_axis',(-1.,0.,1.30103752480477E-16));
#39082=DIRECTION('ref_axis',(0.,1.,0.));
#39083=DIRECTION('center_axis',(-1.30103752480477E-16,7.77119338241477E-16,
-1.));
#39084=DIRECTION('ref_axis',(1.,1.22464679914733E-16,-1.30103752480477E-16));
#39085=DIRECTION('center_axis',(-1.30103752480477E-16,7.77119338241477E-16,
-1.));
#39086=DIRECTION('ref_axis',(-1.,2.49761481516283E-30,1.30103752480477E-16));
#39087=DIRECTION('center_axis',(-1.30103752480477E-16,7.77119338241477E-16,
-1.));
#39088=DIRECTION('ref_axis',(1.,-2.49761481516283E-30,-1.30103752480477E-16));
#39089=DIRECTION('center_axis',(-1.30103752480477E-16,7.77119338241477E-16,
-1.));
#39090=DIRECTION('ref_axis',(1.,-2.49761481516283E-30,-1.30103752480477E-16));
#39091=DIRECTION('',(1.30103752480477E-16,-7.77119338241477E-16,1.));
#39092=DIRECTION('center_axis',(-1.30103752480477E-16,7.77119338241477E-16,
-1.));
#39093=DIRECTION('ref_axis',(-2.59872095719319E-30,-1.,-7.77119338241477E-16));
#39094=DIRECTION('center_axis',(-1.30103752480477E-16,7.77119338241477E-16,
-1.));
#39095=DIRECTION('ref_axis',(-1.,2.49761481516283E-30,1.30103752480477E-16));
#39096=DIRECTION('center_axis',(1.30103752480477E-16,-7.77119338241477E-16,
1.));
#39097=DIRECTION('ref_axis',(1.,-2.49761481516283E-30,-1.30103752480477E-16));
#39098=DIRECTION('',(0.707068359822735,6.36127110587822E-16,-0.70714520046281));
#39099=DIRECTION('center_axis',(1.30103752480477E-16,-7.77119338241477E-16,
1.));
#39100=DIRECTION('ref_axis',(1.,-2.49761481516283E-30,-1.30103752480477E-16));
#39101=DIRECTION('center_axis',(-1.30103752480477E-16,7.77119338241477E-16,
-1.));
#39102=DIRECTION('ref_axis',(-2.59872095719319E-30,-1.,-7.77119338241477E-16));
#39103=DIRECTION('center_axis',(1.92452000305188E-48,7.77119338241477E-16,
-1.));
#39104=DIRECTION('ref_axis',(-1.,2.59872095719319E-30,2.01759179052518E-45));
#39105=DIRECTION('center_axis',(1.30110639599212E-16,-7.76859649098367E-16,
1.));
#39106=DIRECTION('ref_axis',(-1.,2.49764325137018E-30,1.30110639599212E-16));
#39107=DIRECTION('center_axis',(1.92452000305188E-48,7.77119338241477E-16,
-1.));
#39108=DIRECTION('ref_axis',(-1.,2.59872095719319E-30,2.01759179052518E-45));
#39109=DIRECTION('center_axis',(1.30110639599212E-16,-7.76859649098367E-16,
1.));
#39110=DIRECTION('ref_axis',(-1.,2.49764325137018E-30,1.30110639599212E-16));
#39111=DIRECTION('center_axis',(1.92452000305188E-48,7.77119338241477E-16,
-1.));
#39112=DIRECTION('ref_axis',(-1.,2.59872095719319E-30,2.01759179052518E-45));
#39113=DIRECTION('center_axis',(1.30110639599212E-16,-7.76859649098367E-16,
1.));
#39114=DIRECTION('ref_axis',(-1.,2.49764325137018E-30,1.30110639599212E-16));
#39115=DIRECTION('center_axis',(1.92452000305188E-48,7.77119338241477E-16,
-1.));
#39116=DIRECTION('ref_axis',(1.,-1.89882151931499E-15,-1.47561092252874E-30));
#39117=DIRECTION('center_axis',(1.30110639599212E-16,-7.76859649098367E-16,
1.));
#39118=DIRECTION('ref_axis',(-1.,2.49764325137018E-30,1.30110639599212E-16));
#39119=DIRECTION('center_axis',(1.92452000305188E-48,7.77119338241477E-16,
-1.));
#39120=DIRECTION('ref_axis',(-1.,2.59872095719319E-30,2.01759179052518E-45));
#39121=DIRECTION('center_axis',(1.30110639599212E-16,-7.76859649098367E-16,
1.));
#39122=DIRECTION('ref_axis',(-1.,2.49764325137018E-30,1.30110639599212E-16));
#39123=DIRECTION('center_axis',(1.92452000305188E-48,7.77119338241477E-16,
-1.));
#39124=DIRECTION('ref_axis',(-1.,2.59872095719319E-30,2.01759179052518E-45));
#39125=DIRECTION('center_axis',(1.30110639599212E-16,-7.76859649098367E-16,
1.));
#39126=DIRECTION('ref_axis',(-1.,2.49764325137018E-30,1.30110639599212E-16));
#39127=DIRECTION('center_axis',(-3.60555503696922E-16,-1.,-7.77119338241477E-16));
#39128=DIRECTION('ref_axis',(2.2010686355983E-47,-7.77119338241477E-16,
1.));
#39129=DIRECTION('',(1.84116587831701E-16,-7.77119338241477E-16,1.));
#39130=DIRECTION('',(-1.,3.60555503696922E-16,1.30103752480477E-16));
#39131=DIRECTION('',(1.84116587831701E-16,-7.77119338241477E-16,1.));
#39132=DIRECTION('center_axis',(-0.866025403784439,-0.5,-2.29110026800376E-16));
#39133=DIRECTION('ref_axis',(-0.5,0.866025403784439,6.73005088689271E-16));
#39134=DIRECTION('',(1.84116587831701E-16,-7.77119338241477E-16,1.));
#39135=DIRECTION('',(-0.5,0.866025403784439,7.3805696492951E-16));
#39136=DIRECTION('center_axis',(-0.866025403784438,0.500000000000001,5.48009311441101E-16));
#39137=DIRECTION('ref_axis',(-1.72563323017096E-31,1.0960186228822E-15,
-1.));
#39138=DIRECTION('',(1.84116587831701E-16,-7.77119338241477E-16,1.));
#39139=DIRECTION('',(0.500000000000001,0.866025403784438,6.07953212449032E-16));
#39140=DIRECTION('center_axis',(-1.29960708002532E-16,7.77119338241477E-16,
-1.));
#39141=DIRECTION('ref_axis',(-2.59872095719319E-30,-1.,-7.77119338241477E-16));
#39142=DIRECTION('',(1.,-8.41296175292812E-16,-1.30103752480478E-16));
#39143=DIRECTION('',(0.499999999999999,-0.866025403784439,-7.3805696492951E-16));
#39144=DIRECTION('',(-0.5,-0.866025403784438,-6.07953212449032E-16));
#39145=DIRECTION('center_axis',(-1.30103752480477E-16,7.77119338241477E-16,
-1.));
#39146=DIRECTION('ref_axis',(-1.,2.49761481516283E-30,1.30103752480477E-16));
#39147=DIRECTION('center_axis',(8.41296175292813E-16,1.,7.77119338241477E-16));
#39148=DIRECTION('ref_axis',(-1.28389381285026E-46,7.77119338241477E-16,
-1.));
#39149=DIRECTION('',(1.84116587831701E-16,-7.77119338241477E-16,1.));
#39150=DIRECTION('center_axis',(0.866025403784439,0.5,2.29110026800376E-16));
#39151=DIRECTION('ref_axis',(0.5,-0.866025403784439,-6.73005088689271E-16));
#39152=DIRECTION('',(1.84116587831701E-16,-7.77119338241477E-16,1.));
#39153=DIRECTION('center_axis',(0.866025403784438,-0.5,-5.48009311441101E-16));
#39154=DIRECTION('ref_axis',(4.19082355898662E-31,-1.0960186228822E-15,
1.));
#39155=DIRECTION('center_axis',(-1.30110639599212E-16,7.76859649098367E-16,
-1.));
#39156=DIRECTION('ref_axis',(-2.59868716887268E-30,-1.,-7.76859649098367E-16));
#39157=DIRECTION('center_axis',(-1.30103752480477E-16,7.77119338241477E-16,
-1.));
#39158=DIRECTION('ref_axis',(-1.,2.49761481516283E-30,1.30103752480477E-16));
#39159=DIRECTION('',(1.30103752480477E-16,-7.77119338241477E-16,1.));
#39160=DIRECTION('axis',(0.,0.,1.));
#39161=DIRECTION('refdir',(1.,0.,0.));
#39162=DIRECTION('center_axis',(4.77727411898588E-16,1.,7.46349589431828E-16));
#39163=DIRECTION('ref_axis',(1.,-4.77727411898586E-16,-3.34404360992194E-15));
#39164=DIRECTION('',(-1.,4.77727411898586E-16,3.34404360992194E-15));
#39165=DIRECTION('',(-3.34404360992194E-15,7.4634958943183E-16,-1.));
#39166=DIRECTION('',(1.,-4.77727411898586E-16,-3.34404360992194E-15));
#39167=DIRECTION('',(-3.34404360992194E-15,7.4634958943183E-16,-1.));
#39168=DIRECTION('center_axis',(-1.,4.77727411898586E-16,3.34404360992194E-15));
#39169=DIRECTION('ref_axis',(4.77727411898588E-16,1.,7.46349589431829E-16));
#39170=DIRECTION('',(-4.77727411898588E-16,-1.,-7.46349589431828E-16));
#39171=DIRECTION('',(4.77727411898588E-16,1.,7.46349589431828E-16));
#39172=DIRECTION('',(-3.34404360992194E-15,7.4634958943183E-16,-1.));
#39173=DIRECTION('center_axis',(-4.77727411898588E-16,-1.,-7.46349589431828E-16));
#39174=DIRECTION('ref_axis',(-1.,4.77727411898586E-16,3.34404360992194E-15));
#39175=DIRECTION('',(1.,-4.77727411898586E-16,-3.34404360992194E-15));
#39176=DIRECTION('',(-1.,4.77727411898586E-16,3.34404360992194E-15));
#39177=DIRECTION('',(-3.34404360992194E-15,7.4634958943183E-16,-1.));
#39178=DIRECTION('center_axis',(1.,-4.77727411898586E-16,-3.34404360992194E-15));
#39179=DIRECTION('ref_axis',(-4.77727411898588E-16,-1.,-7.46349589431829E-16));
#39180=DIRECTION('',(4.77727411898588E-16,1.,7.46349589431828E-16));
#39181=DIRECTION('',(-4.77727411898588E-16,-1.,-7.46349589431828E-16));
#39182=DIRECTION('center_axis',(-3.81963526526752E-16,0.965925826289068,
-0.25881904510252));
#39183=DIRECTION('ref_axis',(-1.,5.00596043934458E-16,3.34404360992194E-15));
#39184=DIRECTION('',(1.,-5.00596043934458E-16,-3.34404360992194E-15));
#39185=DIRECTION('',(-0.250562807085729,0.250562807085731,0.93511312653103));
#39186=DIRECTION('',(1.,-5.00596043934458E-16,-3.34404360992194E-15));
#39187=DIRECTION('',(-0.250562807085735,-0.250562807085731,-0.935113126531028));
#39188=DIRECTION('center_axis',(0.965925826289067,-2.90369159325025E-16,
-0.258819045102524));
#39189=DIRECTION('ref_axis',(5.0059604393446E-16,1.,7.46349589431828E-16));
#39190=DIRECTION('',(-5.0059604393446E-16,-1.,-7.46349589431828E-16));
#39191=DIRECTION('',(-5.0059604393446E-16,-1.,-7.46349589431828E-16));
#39192=DIRECTION('',(-0.250562807085735,0.250562807085733,-0.935113126531028));
#39193=DIRECTION('center_axis',(-1.34904082127562E-15,-0.965925826289068,
-0.258819045102522));
#39194=DIRECTION('ref_axis',(1.,-5.00596043934458E-16,-3.34404360992194E-15));
#39195=DIRECTION('',(-1.,5.00596043934458E-16,3.34404360992194E-15));
#39196=DIRECTION('',(-1.,5.00596043934458E-16,3.34404360992194E-15));
#39197=DIRECTION('',(0.250562807085729,0.250562807085733,-0.93511312653103));
#39198=DIRECTION('center_axis',(-0.965925826289069,6.76708135423834E-16,
-0.258819045102518));
#39199=DIRECTION('ref_axis',(-5.0059604393446E-16,-1.,-7.46349589431828E-16));
#39200=DIRECTION('',(5.0059604393446E-16,1.,7.46349589431828E-16));
#39201=DIRECTION('',(5.0059604393446E-16,1.,7.46349589431828E-16));
#39202=DIRECTION('center_axis',(3.34404360992194E-15,-7.4634958943183E-16,
1.));
#39203=DIRECTION('ref_axis',(-5.0059604393446E-16,-1.,-7.46349589431828E-16));
#39204=DIRECTION('center_axis',(-3.81963526526752E-16,0.965925826289068,
-0.25881904510252));
#39205=DIRECTION('ref_axis',(-1.,5.00596043934458E-16,3.34404360992194E-15));
#39206=DIRECTION('',(1.,-5.00596043934458E-16,-3.34404360992194E-15));
#39207=DIRECTION('',(0.250562807085735,0.250562807085731,0.935113126531028));
#39208=DIRECTION('',(-1.,5.00596043934458E-16,3.34404360992194E-15));
#39209=DIRECTION('',(-0.250562807085729,0.250562807085731,0.93511312653103));
#39210=DIRECTION('center_axis',(0.965925826289067,-2.90369159325025E-16,
-0.258819045102524));
#39211=DIRECTION('ref_axis',(5.0059604393446E-16,1.,7.46349589431828E-16));
#39212=DIRECTION('',(-5.0059604393446E-16,-1.,-7.46349589431828E-16));
#39213=DIRECTION('',(0.250562807085735,-0.250562807085733,0.935113126531028));
#39214=DIRECTION('',(5.0059604393446E-16,1.,7.46349589431828E-16));
#39215=DIRECTION('center_axis',(-1.34904082127562E-15,-0.965925826289068,
-0.258819045102522));
#39216=DIRECTION('ref_axis',(1.,-5.00596043934458E-16,-3.34404360992194E-15));
#39217=DIRECTION('',(-1.,5.00596043934458E-16,3.34404360992194E-15));
#39218=DIRECTION('',(-0.250562807085729,-0.250562807085733,0.93511312653103));
#39219=DIRECTION('',(1.,-5.00596043934458E-16,-3.34404360992194E-15));
#39220=DIRECTION('center_axis',(-0.965925826289069,6.76708135423834E-16,
-0.258819045102518));
#39221=DIRECTION('ref_axis',(-5.0059604393446E-16,-1.,-7.46349589431828E-16));
#39222=DIRECTION('',(5.0059604393446E-16,1.,7.46349589431828E-16));
#39223=DIRECTION('',(-5.0059604393446E-16,-1.,-7.46349589431828E-16));
#39224=DIRECTION('center_axis',(3.34404360992194E-15,-7.4634958943183E-16,
1.));
#39225=DIRECTION('ref_axis',(-5.0059604393446E-16,-1.,-7.46349589431828E-16));
#39226=DIRECTION('center_axis',(3.34404360992194E-15,-7.4634958943183E-16,
1.));
#39227=DIRECTION('ref_axis',(-5.0059604393446E-16,-1.,-7.46349589431828E-16));
#39228=DIRECTION('axis',(0.,0.,1.));
#39229=DIRECTION('refdir',(1.,0.,0.));
#39230=DIRECTION('center_axis',(-3.34404360992166E-15,6.19091607821767E-16,
-1.));
#39231=DIRECTION('ref_axis',(-5.00596043936355E-16,-1.,-6.19091607821765E-16));
#39232=DIRECTION('center_axis',(-3.34404360992166E-15,6.19091607821767E-16,
-1.));
#39233=DIRECTION('ref_axis',(-5.00596043936355E-16,-1.,-6.19091607821765E-16));
#39234=DIRECTION('',(-3.34404360992166E-15,6.19091607821767E-16,-1.));
#39235=DIRECTION('center_axis',(3.34404360992166E-15,-6.19091607821767E-16,
1.));
#39236=DIRECTION('ref_axis',(-5.00596043936355E-16,-1.,-6.19091607821765E-16));
#39237=DIRECTION('center_axis',(-3.34404360992166E-15,6.19091607821767E-16,
-1.));
#39238=DIRECTION('ref_axis',(-5.00596043936355E-16,-1.,-6.19091607821765E-16));
#39239=DIRECTION('center_axis',(-3.34404360992166E-15,6.19091607821767E-16,
-1.));
#39240=DIRECTION('ref_axis',(-5.00596043936355E-16,-1.,-6.19091607821765E-16));
#39241=DIRECTION('',(-3.34404360992166E-15,6.19091607821767E-16,-1.));
#39242=DIRECTION('center_axis',(3.34404360992166E-15,-6.19091607821767E-16,
1.));
#39243=DIRECTION('ref_axis',(-5.00596043936355E-16,-1.,-6.19091607821765E-16));
#39244=DIRECTION('center_axis',(-3.34404360992166E-15,6.19091607821767E-16,
-1.));
#39245=DIRECTION('ref_axis',(-5.00596043936355E-16,-1.,-6.19091607821765E-16));
#39246=DIRECTION('center_axis',(-3.34404360992166E-15,6.19091607821767E-16,
-1.));
#39247=DIRECTION('ref_axis',(-5.00596043936355E-16,-1.,-6.19091607821765E-16));
#39248=DIRECTION('',(-3.34404360992166E-15,6.19091607821767E-16,-1.));
#39249=DIRECTION('center_axis',(3.34404360992166E-15,-6.19091607821767E-16,
1.));
#39250=DIRECTION('ref_axis',(-5.00596043936355E-16,-1.,-6.19091607821765E-16));
#39251=DIRECTION('center_axis',(-3.34404360992166E-15,6.19091607821767E-16,
-1.));
#39252=DIRECTION('ref_axis',(-5.00596043936355E-16,-1.,-6.19091607821765E-16));
#39253=DIRECTION('center_axis',(-3.34404360992166E-15,6.19091607821767E-16,
-1.));
#39254=DIRECTION('ref_axis',(-5.00596043936355E-16,-1.,-6.19091607821765E-16));
#39255=DIRECTION('',(-3.34404360992166E-15,6.19091607821767E-16,-1.));
#39256=DIRECTION('center_axis',(3.34404360992166E-15,-6.19091607821767E-16,
1.));
#39257=DIRECTION('ref_axis',(-5.00596043936355E-16,-1.,-6.19091607821765E-16));
#39258=DIRECTION('center_axis',(-3.34404360992166E-15,6.19091607821767E-16,
-1.));
#39259=DIRECTION('ref_axis',(-5.00596043936355E-16,-1.,-6.19091607821765E-16));
#39260=DIRECTION('center_axis',(-3.34404360992166E-15,6.19091607821767E-16,
-1.));
#39261=DIRECTION('ref_axis',(-5.00596043936355E-16,-1.,-6.19091607821765E-16));
#39262=DIRECTION('',(-3.34404360992166E-15,6.19091607821767E-16,-1.));
#39263=DIRECTION('center_axis',(3.34404360992166E-15,-6.19091607821767E-16,
1.));
#39264=DIRECTION('ref_axis',(-5.00596043936355E-16,-1.,-6.19091607821765E-16));
#39265=DIRECTION('center_axis',(-3.34404360992166E-15,6.19091607821767E-16,
-1.));
#39266=DIRECTION('ref_axis',(-5.00596043936355E-16,-1.,-6.19091607821765E-16));
#39267=DIRECTION('center_axis',(-3.34404360992166E-15,6.19091607821767E-16,
-1.));
#39268=DIRECTION('ref_axis',(-5.00596043936355E-16,-1.,-6.19091607821765E-16));
#39269=DIRECTION('',(-3.34404360992166E-15,6.19091607821767E-16,-1.));
#39270=DIRECTION('center_axis',(3.34404360992166E-15,-6.19091607821767E-16,
1.));
#39271=DIRECTION('ref_axis',(-5.00596043936355E-16,-1.,-6.19091607821765E-16));
#39272=DIRECTION('center_axis',(-3.34404360992166E-15,6.19091607821767E-16,
-1.));
#39273=DIRECTION('ref_axis',(-5.00596043936355E-16,-1.,-6.19091607821765E-16));
#39274=DIRECTION('',(5.00596043936355E-16,1.,6.19091607821765E-16));
#39275=DIRECTION('',(1.,-5.00596043936353E-16,-3.34404360992166E-15));
#39276=DIRECTION('',(-5.00596043936355E-16,-1.,-6.19091607821765E-16));
#39277=DIRECTION('',(-1.,5.00596043936353E-16,3.34404360992166E-15));
#39278=DIRECTION('',(-5.00596043934461E-16,-1.,-6.19091607821765E-16));
#39279=DIRECTION('',(1.,-5.00596043936353E-16,-3.34404360992166E-15));
#39280=DIRECTION('',(5.00596043936355E-16,1.,6.19091607821765E-16));
#39281=DIRECTION('',(-1.,5.00596043936353E-16,3.34404360992166E-15));
#39282=DIRECTION('center_axis',(-5.00596043936355E-16,-1.,-6.19091607821765E-16));
#39283=DIRECTION('ref_axis',(-1.,5.00596043936353E-16,3.34404360992166E-15));
#39284=DIRECTION('',(-1.,5.00596043936353E-16,3.34404360992166E-15));
#39285=DIRECTION('',(-3.34404360992166E-15,6.19091607821767E-16,-1.));
#39286=DIRECTION('',(-3.34404360992166E-15,6.19091607821767E-16,-1.));
#39287=DIRECTION('center_axis',(1.,-5.00596043936353E-16,-3.34404360992166E-15));
#39288=DIRECTION('ref_axis',(-5.00596043936355E-16,-1.,-6.19091607821765E-16));
#39289=DIRECTION('',(-5.00596043936355E-16,-1.,-6.19091607821765E-16));
#39290=DIRECTION('',(-3.34404360992166E-15,6.19091607821767E-16,-1.));
#39291=DIRECTION('center_axis',(5.00596043936355E-16,1.,6.19091607821765E-16));
#39292=DIRECTION('ref_axis',(1.,-5.00596043936353E-16,-3.34404360992166E-15));
#39293=DIRECTION('',(1.,-5.00596043936353E-16,-3.34404360992166E-15));
#39294=DIRECTION('',(-3.34404360992166E-15,6.19091607821767E-16,-1.));
#39295=DIRECTION('center_axis',(-1.,5.00596043936353E-16,3.34404360992166E-15));
#39296=DIRECTION('ref_axis',(5.00596043936355E-16,1.,6.19091607821765E-16));
#39297=DIRECTION('',(5.00596043936355E-16,1.,6.19091607821765E-16));
#39298=DIRECTION('center_axis',(-5.00596043934278E-16,-1.,6.20455933714055E-13));
#39299=DIRECTION('ref_axis',(-3.34404360992197E-15,-6.20455933714055E-13,
-1.));
#39300=DIRECTION('',(-3.34404360992197E-15,-6.20455933714055E-13,-1.));
#39301=DIRECTION('',(1.,-5.00596043936353E-16,-3.34404360992166E-15));
#39302=DIRECTION('',(-3.34404360992226E-15,-6.20455933714055E-13,-1.));
#39303=DIRECTION('center_axis',(-1.,5.00596043936353E-16,3.34404360992166E-15));
#39304=DIRECTION('ref_axis',(-5.00596043936355E-16,-1.,-6.19091607821765E-16));
#39305=DIRECTION('',(2.66598427033833E-15,-0.491594368037543,0.870824309096714));
#39306=DIRECTION('',(8.46232198011949E-16,-0.920455750162943,0.390846788386413));
#39307=DIRECTION('',(3.34404360992196E-15,5.89417440552492E-13,1.));
#39308=DIRECTION('',(-1.18154003924372E-15,0.874903192709269,-0.484297845738681));
#39309=DIRECTION('center_axis',(5.00596043936355E-16,1.,6.19091607821765E-16));
#39310=DIRECTION('ref_axis',(1.,-5.00596043936353E-16,-3.34404360992166E-15));
#39311=DIRECTION('',(-1.,5.00596043936353E-16,3.34404360992166E-15));
#39312=DIRECTION('',(-3.34404360992166E-15,6.19091607821767E-16,-1.));
#39313=DIRECTION('',(1.,-5.00596043936353E-16,-3.34404360992166E-15));
#39314=DIRECTION('',(-3.34404360992166E-15,6.19091607821767E-16,-1.));
#39315=DIRECTION('center_axis',(3.34404360992166E-15,-6.19091607821767E-16,
1.));
#39316=DIRECTION('ref_axis',(-5.00596043936355E-16,-1.,-6.19091607821765E-16));
#39317=DIRECTION('',(-5.00596043936355E-16,-1.,-6.19091607821765E-16));
#39318=DIRECTION('',(-1.,5.00596043936353E-16,3.34404360992166E-15));
#39319=DIRECTION('',(-5.00596043934461E-16,-1.,-6.19091607821765E-16));
#39320=DIRECTION('center_axis',(-5.00596043934278E-16,-1.,6.20455933714055E-13));
#39321=DIRECTION('ref_axis',(-3.34404360992197E-15,-6.20455933714055E-13,
-1.));
#39322=DIRECTION('',(-3.34404360992226E-15,-6.20455933714055E-13,-1.));
#39323=DIRECTION('',(1.,-5.00596043936353E-16,-3.34404360992166E-15));
#39324=DIRECTION('',(-3.34404360992197E-15,-6.20455933714055E-13,-1.));
#39325=DIRECTION('',(-1.,5.00596043936353E-16,3.34404360992166E-15));
#39326=DIRECTION('center_axis',(2.07984420920684E-15,0.870824309096714,
0.491594368037543));
#39327=DIRECTION('ref_axis',(2.66598427033833E-15,-0.491594368037543,0.870824309096714));
#39328=DIRECTION('',(2.66598427033951E-15,-0.491594368037543,0.870824309096714));
#39329=DIRECTION('',(2.66598427033833E-15,-0.491594368037543,0.870824309096714));
#39330=DIRECTION('',(1.,-5.00596043936353E-16,-3.34404360992166E-15));
#39331=DIRECTION('center_axis',(3.27370052559951E-15,0.390846788386413,
0.920455750162943));
#39332=DIRECTION('ref_axis',(8.46232198011949E-16,-0.920455750162943,0.390846788386413));
#39333=DIRECTION('',(8.46232198013806E-16,-0.920455750162943,0.390846788386413));
#39334=DIRECTION('',(8.46232198011949E-16,-0.920455750162943,0.390846788386413));
#39335=DIRECTION('',(-1.,5.00596043936353E-16,3.34404360992166E-15));
#39336=DIRECTION('center_axis',(-3.16815201654317E-15,-0.484297845738681,
-0.874903192709269));
#39337=DIRECTION('ref_axis',(-1.18154003924372E-15,0.874903192709269,-0.484297845738681));
#39338=DIRECTION('',(-1.18154003924552E-15,0.874903192709269,-0.484297845738681));
#39339=DIRECTION('',(1.,-5.00596043936353E-16,-3.34404360992166E-15));
#39340=DIRECTION('',(-1.18154003924372E-15,0.874903192709269,-0.484297845738681));
#39341=DIRECTION('center_axis',(-1.,5.00596043936353E-16,3.34404360992166E-15));
#39342=DIRECTION('ref_axis',(-5.00596043936355E-16,-1.,-6.19091607821765E-16));
#39343=DIRECTION('',(-3.34404360992196E-15,-5.89417440552492E-13,-1.));
#39344=DIRECTION('',(5.00596043936355E-16,1.,6.19091607821765E-16));
#39345=DIRECTION('center_axis',(-1.,5.00596043934459E-16,3.34404360992195E-15));
#39346=DIRECTION('ref_axis',(-5.00596043934461E-16,-1.,-6.19091607821765E-16));
#39347=DIRECTION('',(3.34404360992225E-15,5.89417440552492E-13,1.));
#39348=DIRECTION('',(-5.00596043936355E-16,-1.,-6.19091607821765E-16));
#39349=DIRECTION('center_axis',(3.34404360992166E-15,-6.19091607821767E-16,
1.));
#39350=DIRECTION('ref_axis',(-5.00596043936355E-16,-1.,-6.19091607821765E-16));
#39351=DIRECTION('center_axis',(2.07984420920684E-15,0.870824309096714,
0.491594368037543));
#39352=DIRECTION('ref_axis',(2.66598427033833E-15,-0.491594368037543,0.870824309096714));
#39353=DIRECTION('',(2.66598427033951E-15,-0.491594368037543,0.870824309096714));
#39354=DIRECTION('',(1.,-5.00596043936353E-16,-3.34404360992166E-15));
#39355=DIRECTION('center_axis',(3.27370052559951E-15,0.390846788386413,
0.920455750162943));
#39356=DIRECTION('ref_axis',(8.46232198011949E-16,-0.920455750162943,0.390846788386413));
#39357=DIRECTION('',(8.46232198013806E-16,-0.920455750162943,0.390846788386413));
#39358=DIRECTION('',(1.,-5.00596043936353E-16,-3.34404360992166E-15));
#39359=DIRECTION('center_axis',(5.00596043934382E-16,1.,-5.89417440552492E-13));
#39360=DIRECTION('ref_axis',(3.34404360992196E-15,5.89417440552492E-13,
1.));
#39361=DIRECTION('',(3.34404360992225E-15,5.89417440552492E-13,1.));
#39362=DIRECTION('',(1.,-5.00596043936353E-16,-3.34404360992166E-15));
#39363=DIRECTION('center_axis',(-3.16815201654317E-15,-0.484297845738681,
-0.874903192709269));
#39364=DIRECTION('ref_axis',(-1.18154003924372E-15,0.874903192709269,-0.484297845738681));
#39365=DIRECTION('',(-1.18154003924552E-15,0.874903192709269,-0.484297845738681));
#39366=DIRECTION('center_axis',(-1.,5.00596043934459E-16,3.34404360992195E-15));
#39367=DIRECTION('ref_axis',(-5.00596043934461E-16,-1.,-6.19091607821765E-16));
#39368=DIRECTION('axis',(0.,0.,1.));
#39369=DIRECTION('refdir',(1.,0.,0.));
#39370=DIRECTION('center_axis',(-0.857167300702049,-0.515038074910159,2.44576428750191E-14));
#39371=DIRECTION('ref_axis',(-0.515038074910159,0.857167300702049,-3.63131968870903E-14));
#39372=DIRECTION('center_axis',(-0.857167300702049,-0.515038074910159,2.44576428750191E-14));
#39373=DIRECTION('ref_axis',(-0.515038074910159,0.857167300702049,-3.63131968870903E-14));
#39374=DIRECTION('center_axis',(2.77102527463854E-15,8.5557679050281E-15,
1.));
#39375=DIRECTION('ref_axis',(-6.7618653731838E-14,1.,-8.55576790502791E-15));
#39376=DIRECTION('',(0.857167300702075,0.515038074910116,-6.78177848602257E-15));
#39377=DIRECTION('',(-0.515038074910087,0.857167300702093,-5.90654095760951E-15));
#39378=DIRECTION('',(0.8571673007021,0.515038074910075,-6.78177848602229E-15));
#39379=DIRECTION('center_axis',(-0.515038074910103,0.857167300702083,-5.90654095760938E-15));
#39380=DIRECTION('ref_axis',(-2.77102527463854E-15,-8.5557679050281E-15,
-1.));
#39381=DIRECTION('',(-2.77102527463854E-15,-8.5557679050281E-15,-1.));
#39382=DIRECTION('',(0.85716730070209,0.515038074910091,-6.7817784860224E-15));
#39383=DIRECTION('center_axis',(-2.77102527463854E-15,-8.5557679050281E-15,
-1.));
#39384=DIRECTION('ref_axis',(6.7618653731838E-14,-1.,8.55576790502791E-15));
#39385=DIRECTION('',(0.51503807491012,-0.857167300702073,5.90654095760924E-15));
#39386=DIRECTION('',(0.857167300702092,0.515038074910088,-6.78177848602238E-15));
#39387=DIRECTION('center_axis',(-0.857167300702051,-0.515038074910156,6.78177848602285E-15));
#39388=DIRECTION('ref_axis',(2.77102527463854E-15,8.5557679050281E-15,1.));
#39389=DIRECTION('center_axis',(-0.857167300702059,-0.515038074910142,1.20908994046383E-14));
#39390=DIRECTION('ref_axis',(0.515038074910142,-0.857167300702059,1.31876972665472E-13));
#39391=DIRECTION('',(-2.77102527463854E-15,-8.5557679050281E-15,-1.));
#39392=DIRECTION('center_axis',(0.857167300702053,0.515038074910153,-7.55127991844926E-15));
#39393=DIRECTION('ref_axis',(0.515038074910153,-0.857167300702053,5.90654095760898E-15));
#39394=DIRECTION('',(-0.857167300702053,-0.515038074910153,7.55127991844926E-15));
#39395=DIRECTION('center_axis',(-5.19067754597624E-15,-4.44287817572889E-15,
-1.));
#39396=DIRECTION('ref_axis',(0.861906247151903,0.507067669172983,-6.72671728481439E-15));
#39397=DIRECTION('center_axis',(-2.77102527463854E-15,-8.5557679050281E-15,
-1.));
#39398=DIRECTION('ref_axis',(0.91847083292034,0.395488721804576,-5.92881560485675E-15));
#39399=DIRECTION('',(2.77102527463854E-15,8.5557679050281E-15,1.));
#39400=DIRECTION('center_axis',(3.22934968323309E-13,1.72787305786163E-13,
-1.));
#39401=DIRECTION('ref_axis',(0.885014263114158,0.465563909774484,3.66245586665653E-13));
#39402=DIRECTION('center_axis',(2.77102527463854E-15,8.5557679050281E-15,
1.));
#39403=DIRECTION('ref_axis',(0.861906247151891,0.507067669173004,-6.72671728481454E-15));
#39404=DIRECTION('',(2.77102527463854E-15,8.5557679050281E-15,1.));
#39405=DIRECTION('center_axis',(-4.25208859581478E-13,-2.05700297011475E-13,
-1.));
#39406=DIRECTION('ref_axis',(0.918470832920341,0.395488721804574,-4.71894082964798E-13));
#39407=DIRECTION('',(2.77102527463854E-15,8.5557679050281E-15,1.));
#39408=DIRECTION('',(-2.77102527463854E-15,-8.5557679050281E-15,-1.));
#39409=DIRECTION('center_axis',(-1.,-6.7618653731838E-14,2.77102527463912E-15));
#39410=DIRECTION('ref_axis',(-2.77102527463854E-15,-8.5557679050281E-15,
-1.));
#39411=DIRECTION('',(1.,6.7618653731838E-14,-2.77102527463912E-15));
#39412=DIRECTION('',(1.,6.7618653731838E-14,-2.77102527463912E-15));
#39413=DIRECTION('center_axis',(-1.,-6.7618653731838E-14,2.77102527463912E-15));
#39414=DIRECTION('ref_axis',(2.77102527463841E-15,1.04984153671894E-14,
1.));
#39415=DIRECTION('',(1.,6.7618653731838E-14,-2.77102527463912E-15));
#39416=DIRECTION('',(1.,6.7618653731838E-14,-2.77102527463912E-15));
#39417=DIRECTION('center_axis',(-1.,-6.7618653731838E-14,2.77102527463912E-15));
#39418=DIRECTION('ref_axis',(6.7618653731838E-14,-1.,8.55576790502791E-15));
#39419=DIRECTION('',(-1.,-6.7618653731838E-14,2.77102527463912E-15));
#39420=DIRECTION('',(1.,6.7618653731838E-14,-2.77102527463912E-15));
#39421=DIRECTION('center_axis',(6.7618653731838E-14,-1.,8.55576790502791E-15));
#39422=DIRECTION('ref_axis',(2.77102527463854E-15,8.5557679050281E-15,1.));
#39423=DIRECTION('',(2.77102527463854E-15,8.5557679050281E-15,1.));
#39424=DIRECTION('',(1.,6.7618653731838E-14,-2.77102527463912E-15));
#39425=DIRECTION('',(-2.77102527463854E-15,-8.5557679050281E-15,-1.));
#39426=DIRECTION('center_axis',(-6.7618653731838E-14,1.,-8.55576790502791E-15));
#39427=DIRECTION('ref_axis',(-2.77102527463854E-15,-8.5557679050281E-15,
-1.));
#39428=DIRECTION('',(1.,6.7618653731838E-14,-2.77102527463912E-15));
#39429=DIRECTION('',(1.,6.7618653731838E-14,-2.77102527463912E-15));
#39430=DIRECTION('',(-2.77102527463854E-15,-8.5557679050281E-15,-1.));
#39431=DIRECTION('center_axis',(-0.85716730070211,0.515038074910058,-2.11149495005192E-14));
#39432=DIRECTION('ref_axis',(0.515038074910058,0.85716730070211,-8.76090800356362E-15));
#39433=DIRECTION('center_axis',(0.857167300702118,-0.515038074910045,-9.73848807776743E-16));
#39434=DIRECTION('ref_axis',(0.515038074910045,0.857167300702118,-1.31047159934894E-14));
#39435=DIRECTION('',(0.85716730070211,-0.515038074910058,2.11149495005192E-14));
#39436=DIRECTION('center_axis',(0.85716730070212,-0.515038074910041,-1.95197940709233E-15));
#39437=DIRECTION('ref_axis',(0.515038074910041,0.85716730070212,2.09861197125113E-15));
#39438=DIRECTION('center_axis',(1.64678176605324E-15,8.08403097159972E-16,
-1.));
#39439=DIRECTION('ref_axis',(0.918470832920391,-0.395488721804457,1.19280671270647E-15));
#39440=DIRECTION('center_axis',(4.19666809032036E-13,-2.05700297011328E-13,
-1.));
#39441=DIRECTION('ref_axis',(0.893066438469014,-0.449924812030044,4.67340009953242E-13));
#39442=DIRECTION('center_axis',(2.77102527463854E-15,8.5557679050281E-15,
1.));
#39443=DIRECTION('ref_axis',(0.885014263114177,-0.465563909774447,1.53085986548262E-15));
#39444=DIRECTION('center_axis',(3.22934968323738E-13,-1.898988415964E-13,
-1.));
#39445=DIRECTION('ref_axis',(0.861906247151989,-0.507067669172838,3.74631229608968E-13));
#39446=DIRECTION('',(-2.77102527463854E-15,-8.5557679050281E-15,-1.));
#39447=DIRECTION('center_axis',(5.00337040136837E-14,-3.31988340433105E-14,
-1.));
#39448=DIRECTION('ref_axis',(0.893066438469019,-0.449924812030035,5.96204010134664E-14));
#39449=DIRECTION('',(2.77102527463854E-15,8.5557679050281E-15,1.));
#39450=DIRECTION('',(2.77102527463854E-15,8.5557679050281E-15,1.));
#39451=DIRECTION('',(2.77102527463854E-15,8.5557679050281E-15,1.));
#39452=DIRECTION('center_axis',(-0.85716730070212,0.515038074910041,-2.03131397634351E-15));
#39453=DIRECTION('ref_axis',(-2.77102527463854E-15,-8.5557679050281E-15,
-1.));
#39454=DIRECTION('center_axis',(-7.09168149328433E-14,1.,0.));
#39455=DIRECTION('ref_axis',(0.,-8.86460186660541E-15,-1.));
#39456=DIRECTION('center_axis',(-0.515038074912743,-0.857167300700497,6.99406836105656E-14));
#39457=DIRECTION('ref_axis',(0.857167300700497,-0.515038074912743,-7.69635029986347E-14));
#39458=DIRECTION('center_axis',(5.4143828599301E-14,-4.58060313724235E-14,
1.));
#39459=DIRECTION('ref_axis',(0.813525514741032,-0.581529222709692,-7.06849318507178E-14));
#39460=DIRECTION('center_axis',(-0.515038074910113,-0.857167300702077,-4.75968469660724E-14));
#39461=DIRECTION('ref_axis',(0.765900867954103,-0.460199669632744,0.449012387955015));
#39462=DIRECTION('center_axis',(2.77102527463854E-15,8.5557679050281E-15,
1.));
#39463=DIRECTION('ref_axis',(0.89942493888384,-0.43707525589285,1.24718520816265E-15));
#39464=DIRECTION('center_axis',(0.515038074910163,0.857167300702047,7.80464133895757E-14));
#39465=DIRECTION('ref_axis',(0.854456218440598,-0.513409092344321,0.0794712191071334));
#39466=DIRECTION('center_axis',(2.77102527463854E-15,8.5557679050281E-15,
1.));
#39467=DIRECTION('ref_axis',(0.997159343857271,-0.0753209330673478,-2.1187253229561E-15));
#39468=DIRECTION('center_axis',(0.515038074910056,0.857167300702111,-8.76090800356364E-15));
#39469=DIRECTION('ref_axis',(0.853796957819509,-0.513012968599281,-0.0885914717515463));
#39470=DIRECTION('center_axis',(-2.77102527463854E-15,-8.5557679050281E-15,
-1.));
#39471=DIRECTION('ref_axis',(0.895386922140334,-0.44528896197869,1.32864921752887E-15));
#39472=DIRECTION('center_axis',(0.515038074910152,0.857167300702054,-9.20691349666037E-14));
#39473=DIRECTION('ref_axis',(0.765900867954062,-0.460199669632791,-0.449012387955036));
#39474=DIRECTION('center_axis',(3.34893569077092E-13,-2.11445125090906E-13,
-1.));
#39475=DIRECTION('ref_axis',(0.808168976755185,-0.588950681305725,3.95181343523989E-13));
#39476=DIRECTION('center_axis',(-0.515038074910049,-0.857167300702115,4.43474428456801E-14));
#39477=DIRECTION('ref_axis',(0.854456218440674,-0.513409092344209,-0.0794712191070315));
#39478=DIRECTION('center_axis',(-5.41438285993037E-14,4.58060313724264E-14,
-1.));
#39479=DIRECTION('ref_axis',(0.534642392051038,-0.845078406197877,-6.76572740235932E-14));
#39480=DIRECTION('center_axis',(-2.77102527463854E-15,-8.5557679050281E-15,
-1.));
#39481=DIRECTION('ref_axis',(6.7618653731838E-14,-1.,8.55576790502791E-15));
#39482=DIRECTION('center_axis',(2.77102527463854E-15,8.5557679050281E-15,
1.));
#39483=DIRECTION('ref_axis',(0.895386922140312,0.445288961978735,-6.29092880119255E-15));
#39484=DIRECTION('',(0.857167300702098,0.515038074910078,-6.78177848602231E-15));
#39485=DIRECTION('',(0.51503807491012,-0.857167300702073,5.90654095760924E-15));
#39486=DIRECTION('',(0.857167300702087,0.515038074910096,-6.78177848602243E-15));
#39487=DIRECTION('center_axis',(-0.515038074910065,0.857167300702106,-5.90654095760967E-15));
#39488=DIRECTION('ref_axis',(-2.77102527463854E-15,-8.5557679050281E-15,
-1.));
#39489=DIRECTION('center_axis',(0.515038074910833,-0.857167300701645,3.31402177757022E-14));
#39490=DIRECTION('ref_axis',(0.857167300701645,0.515038074910833,1.33541552527618E-14));
#39491=DIRECTION('',(0.857167300702098,0.515038074910078,-6.78177848602231E-15));
#39492=DIRECTION('',(-2.77102527463854E-15,-8.5557679050281E-15,-1.));
#39493=DIRECTION('center_axis',(-0.857167300702058,-0.515038074910145,3.72458084698414E-15));
#39494=DIRECTION('ref_axis',(2.65998341932259E-15,2.80470534102394E-15,
1.));
#39495=DIRECTION('center_axis',(-0.857167300702053,-0.515038074910153,-1.03164475269556E-15));
#39496=DIRECTION('ref_axis',(0.515038074910153,-0.857167300702053,2.11098689223494E-14));
#39497=DIRECTION('center_axis',(0.85716730070204,0.515038074910174,1.1501575548429E-14));
#39498=DIRECTION('ref_axis',(0.515038074910174,-0.85716730070204,5.90654095760881E-15));
#39499=DIRECTION('center_axis',(-0.85716730070205,-0.515038074910157,9.93521908124291E-15));
#39500=DIRECTION('ref_axis',(0.515038074910157,-0.85716730070205,1.67660609324238E-14));
#39501=DIRECTION('',(-0.85716730070204,-0.515038074910174,-1.1501575548429E-14));
#39502=DIRECTION('center_axis',(-0.857167300702099,0.515038074910076,-2.54241575221074E-14));
#39503=DIRECTION('ref_axis',(0.515038074910076,0.857167300702099,-8.7609080035636E-15));
#39504=DIRECTION('center_axis',(0.85716730070211,-0.515038074910058,1.38516209272139E-14));
#39505=DIRECTION('ref_axis',(0.515038074910058,0.85716730070211,1.64991411593497E-13));
#39506=DIRECTION('',(0.857167300702099,-0.515038074910076,2.54241575221073E-14));
#39507=DIRECTION('center_axis',(0.85716730070212,-0.515038074910041,-1.95197940709221E-15));
#39508=DIRECTION('ref_axis',(0.515038074910041,0.85716730070212,3.03333639057696E-14));
#39509=DIRECTION('center_axis',(2.77102527463854E-15,8.5557679050281E-15,
1.));
#39510=DIRECTION('ref_axis',(-6.7618653731838E-14,1.,-8.55576790502791E-15));
#39511=DIRECTION('center_axis',(1.41462354879372E-13,-4.82321162475789E-14,
-1.));
#39512=DIRECTION('ref_axis',(0.895386922140315,-0.445288961978728,1.48140771512084E-13));
#39513=DIRECTION('',(0.857167300702158,-0.515038074909978,2.03131397634287E-15));
#39514=DIRECTION('',(0.515038074909971,0.857167300702162,-8.76090800356383E-15));
#39515=DIRECTION('',(0.857167300702148,-0.515038074909994,2.03131397634304E-15));
#39516=DIRECTION('center_axis',(-0.515038074909966,-0.857167300702166,8.76090800356385E-15));
#39517=DIRECTION('ref_axis',(2.77102527463854E-15,8.5557679050281E-15,1.));
#39518=DIRECTION('center_axis',(0.515038074910056,0.857167300702111,-8.76090800356364E-15));
#39519=DIRECTION('ref_axis',(0.853796957819509,-0.513012968599281,-0.0885914717515493));
#39520=DIRECTION('',(0.857167300702158,-0.515038074909978,2.03131397634287E-15));
#39521=DIRECTION('',(2.77102527463854E-15,8.5557679050281E-15,1.));
#39522=DIRECTION('center_axis',(-2.77102527463854E-15,-8.5557679050281E-15,
-1.));
#39523=DIRECTION('ref_axis',(6.7618653731838E-14,-1.,8.55576790502791E-15));
#39524=DIRECTION('center_axis',(2.77102527463854E-15,8.5557679050281E-15,
1.));
#39525=DIRECTION('ref_axis',(0.997159343857267,-0.0753209330674082,-2.11872532295557E-15));
#39526=DIRECTION('',(0.857167300702159,-0.515038074909977,2.03131397634286E-15));
#39527=DIRECTION('',(-0.515038074909971,-0.857167300702162,8.76090800356383E-15));
#39528=DIRECTION('center_axis',(-0.515038074910013,-0.857167300702137,8.76090800356374E-15));
#39529=DIRECTION('ref_axis',(2.77102527463854E-15,8.5557679050281E-15,1.));
#39530=DIRECTION('center_axis',(0.515038074910268,0.857167300701984,9.11494052980619E-14));
#39531=DIRECTION('ref_axis',(0.854456218440525,-0.513409092344421,0.079471219107265));
#39532=DIRECTION('',(0.857167300702156,-0.515038074909982,2.03131397634291E-15));
#39533=DIRECTION('',(2.77102527463854E-15,8.5557679050281E-15,1.));
#39534=DIRECTION('center_axis',(-2.77102527463854E-15,-8.5557679050281E-15,
-1.));
#39535=DIRECTION('ref_axis',(6.7618653731838E-14,-1.,8.55576790502791E-15));
#39536=DIRECTION('center_axis',(6.78100213977318E-13,-3.9722294646622E-13,
1.));
#39537=DIRECTION('ref_axis',(0.899424938883905,-0.437075255892716,-7.83516564486894E-13));
#39538=DIRECTION('',(0.857167300702151,-0.515038074909989,2.03131397634299E-15));
#39539=DIRECTION('',(-0.515038074909941,-0.85716730070218,8.76090800356391E-15));
#39540=DIRECTION('center_axis',(0.515038074909992,0.85716730070215,-8.76090800356379E-15));
#39541=DIRECTION('ref_axis',(-2.77102527463854E-15,-8.5557679050281E-15,
-1.));
#39542=DIRECTION('center_axis',(-0.515038074910134,-0.857167300702064,-5.44461381909585E-14));
#39543=DIRECTION('ref_axis',(0.765900867954141,-0.460199669632797,0.449012387954897));
#39544=DIRECTION('',(0.857167300702159,-0.515038074909977,2.03131397634286E-15));
#39545=DIRECTION('',(-2.77102527463854E-15,-8.5557679050281E-15,-1.));
#39546=DIRECTION('center_axis',(-2.77102527463854E-15,-8.5557679050281E-15,
-1.));
#39547=DIRECTION('ref_axis',(6.7618653731838E-14,-1.,8.55576790502791E-15));
#39548=DIRECTION('center_axis',(2.77102527463854E-15,8.5557679050281E-15,
1.));
#39549=DIRECTION('ref_axis',(0.813525514741016,-0.581529222709715,2.72112929658504E-15));
#39550=DIRECTION('',(0.857167300702151,-0.51503807490999,2.031313976343E-15));
#39551=DIRECTION('',(-0.515038074910003,-0.857167300702143,8.76090800356376E-15));
#39552=DIRECTION('center_axis',(0.51503807490998,0.857167300702157,-8.76090800356381E-15));
#39553=DIRECTION('ref_axis',(-2.77102527463854E-15,-8.5557679050281E-15,
-1.));
#39554=DIRECTION('center_axis',(-0.515038074909266,-0.857167300702586,-2.04247301180779E-15));
#39555=DIRECTION('ref_axis',(0.857167300702586,-0.515038074909266,7.947721297203E-14));
#39556=DIRECTION('',(0.857167300702151,-0.51503807490999,2.031313976343E-15));
#39557=DIRECTION('',(-2.77102527463854E-15,-8.5557679050281E-15,-1.));
#39558=DIRECTION('center_axis',(2.77102527463854E-15,8.5557679050281E-15,
1.));
#39559=DIRECTION('ref_axis',(-6.7618653731838E-14,1.,-8.55576790502791E-15));
#39560=DIRECTION('center_axis',(-2.77102527463854E-15,-8.5557679050281E-15,
-1.));
#39561=DIRECTION('ref_axis',(0.534642392051038,-0.845078406197877,5.74878712371346E-15));
#39562=DIRECTION('',(0.857167300702159,-0.515038074909977,2.03131397634286E-15));
#39563=DIRECTION('',(0.515038074909973,0.857167300702161,-8.76090800356383E-15));
#39564=DIRECTION('center_axis',(0.515038074909992,0.85716730070215,-1.83469634573233E-15));
#39565=DIRECTION('ref_axis',(-2.65430854586528E-15,-5.45548554721672E-16,
-1.));
#39566=DIRECTION('center_axis',(-0.515038074910081,-0.857167300702096,5.46958285005906E-14));
#39567=DIRECTION('ref_axis',(0.854456218440659,-0.513409092344244,-0.0794712191069747));
#39568=DIRECTION('',(0.857167300702151,-0.515038074909989,2.03131397634299E-15));
#39569=DIRECTION('',(-2.77102527463854E-15,-8.5557679050281E-15,-1.));
#39570=DIRECTION('center_axis',(2.77102527463854E-15,8.5557679050281E-15,
1.));
#39571=DIRECTION('ref_axis',(-6.7618653731838E-14,1.,-8.55576790502791E-15));
#39572=DIRECTION('center_axis',(-2.77102527463854E-15,-8.5557679050281E-15,
-1.));
#39573=DIRECTION('ref_axis',(0.808168976755134,-0.588950681305795,2.79946867599331E-15));
#39574=DIRECTION('',(0.857167300702156,-0.515038074909982,2.03131397634291E-15));
#39575=DIRECTION('',(0.515038074909941,0.85716730070218,-8.76090800356391E-15));
#39576=DIRECTION('center_axis',(-0.515038074909963,-0.857167300702167,8.76090800356385E-15));
#39577=DIRECTION('ref_axis',(2.77102527463854E-15,8.5557679050281E-15,1.));
#39578=DIRECTION('center_axis',(0.515038074910184,0.857167300702034,-1.02454745030335E-13));
#39579=DIRECTION('ref_axis',(0.765900867954022,-0.460199669632811,-0.449012387955084));
#39580=DIRECTION('',(2.77102527463854E-15,8.5557679050281E-15,1.));
#39581=DIRECTION('center_axis',(0.857167300702158,-0.515038074909979,2.03131397634288E-15));
#39582=DIRECTION('ref_axis',(2.77102527463854E-15,8.5557679050281E-15,1.));
#39583=DIRECTION('center_axis',(-7.09168149328348E-14,1.,0.));
#39584=DIRECTION('ref_axis',(0.,-8.86460186660431E-15,-1.));
#39585=DIRECTION('center_axis',(-0.85716730070212,0.515038074910041,-2.03131397634351E-15));
#39586=DIRECTION('ref_axis',(-2.77102527463854E-15,-8.5557679050281E-15,
-1.));
#39587=DIRECTION('center_axis',(-1.,-6.7618653731838E-14,2.77102527463912E-15));
#39588=DIRECTION('ref_axis',(-6.7618653731838E-14,1.,-9.47596933447271E-15));
#39589=DIRECTION('',(-1.,-6.7618653731838E-14,2.77102527463912E-15));
#39590=DIRECTION('center_axis',(1.,6.7618653731838E-14,-2.77102527463912E-15));
#39591=DIRECTION('ref_axis',(-2.77102527463854E-15,-8.5557679050281E-15,
-1.));
#39592=DIRECTION('center_axis',(-1.,-6.7618653731838E-14,2.77102527463912E-15));
#39593=DIRECTION('ref_axis',(-2.77102527463873E-15,-5.7951636166937E-15,
-1.));
#39594=DIRECTION('',(-1.,-6.7618653731838E-14,2.77102527463912E-15));
#39595=DIRECTION('center_axis',(-1.,-6.7618653731838E-14,2.77102527463912E-15));
#39596=DIRECTION('ref_axis',(-2.77102527463873E-15,-5.7951636166937E-15,
-1.));
#39597=DIRECTION('',(-1.,-6.7618653731838E-14,2.77102527463912E-15));
#39598=DIRECTION('center_axis',(-2.77102527463854E-15,-8.5557679050281E-15,
-1.));
#39599=DIRECTION('ref_axis',(6.7618653731838E-14,-1.,8.55576790502791E-15));
#39600=DIRECTION('',(6.7618653731838E-14,-1.,8.55576790502791E-15));
#39601=DIRECTION('',(6.7618653731838E-14,-1.,8.55576790502791E-15));
#39602=DIRECTION('',(-1.,-6.7618653731838E-14,2.77102527463912E-15));
#39603=DIRECTION('center_axis',(1.,6.7618653731838E-14,-2.77102527463912E-15));
#39604=DIRECTION('ref_axis',(6.7618653731838E-14,-1.,9.01586861975031E-15));
#39605=DIRECTION('center_axis',(-1.,-7.65049048161611E-14,-6.11522580968364E-15));
#39606=DIRECTION('ref_axis',(7.6504904816161E-14,-1.,1.91380843436431E-14));
#39607=DIRECTION('center_axis',(-1.,-7.6504904816161E-14,-6.11522580968382E-15));
#39608=DIRECTION('ref_axis',(7.6504904816161E-14,-1.,9.47596933447271E-15));
#39609=DIRECTION('',(-1.,-6.7618653731838E-14,2.77102527463912E-15));
#39610=DIRECTION('center_axis',(6.7618653731838E-14,-1.,8.55576790502791E-15));
#39611=DIRECTION('ref_axis',(2.77102527463854E-15,8.5557679050281E-15,1.));
#39612=DIRECTION('',(2.77102527463854E-15,8.5557679050281E-15,1.));
#39613=DIRECTION('',(2.77102527463854E-15,8.5557679050281E-15,1.));
#39614=DIRECTION('',(-1.,-6.7618653731838E-14,2.77102527463912E-15));
#39615=DIRECTION('center_axis',(1.,6.7618653731838E-14,-2.77102527463912E-15));
#39616=DIRECTION('ref_axis',(2.77102426704276E-15,1.49011597348792E-8,1.));
#39617=DIRECTION('center_axis',(-1.,-6.7618653731838E-14,2.77102527463912E-15));
#39618=DIRECTION('ref_axis',(2.7710242670427E-15,1.49011606550806E-8,1.));
#39619=DIRECTION('center_axis',(-1.,-5.87324028735622E-14,-6.11522571605215E-15));
#39620=DIRECTION('ref_axis',(-6.11522659123301E-15,1.49011588146778E-8,
1.));
#39621=DIRECTION('',(-1.,-6.7618653731838E-14,2.77102527463912E-15));
#39622=DIRECTION('center_axis',(2.77102527463854E-15,8.5557679050281E-15,
1.));
#39623=DIRECTION('ref_axis',(-6.7618653731838E-14,1.,-8.55576790502791E-15));
#39624=DIRECTION('',(-6.7618653731838E-14,1.,-8.55576790502791E-15));
#39625=DIRECTION('',(-6.7618653731838E-14,1.,-8.55576790502791E-15));
#39626=DIRECTION('',(-1.,-6.7618653731838E-14,2.77102527463912E-15));
#39627=DIRECTION('center_axis',(1.,6.7618653731838E-14,-2.77102527463912E-15));
#39628=DIRECTION('ref_axis',(-6.7618653731838E-14,1.,-8.55576790502791E-15));
#39629=DIRECTION('center_axis',(-1.,-6.7618653731838E-14,2.77102527463912E-15));
#39630=DIRECTION('ref_axis',(-6.7618653731838E-14,1.,-8.55576790502791E-15));
#39631=DIRECTION('center_axis',(-1.,-6.7618653731838E-14,2.77102527463912E-15));
#39632=DIRECTION('ref_axis',(-6.7618653731838E-14,1.,-1.95981850583656E-14));
#39633=DIRECTION('',(-1.,-6.7618653731838E-14,2.77102527463912E-15));
#39634=DIRECTION('center_axis',(-6.7618653731838E-14,1.,-8.55576790502791E-15));
#39635=DIRECTION('ref_axis',(-2.77102527463854E-15,-8.5557679050281E-15,
-1.));
#39636=DIRECTION('',(-2.77102527463854E-15,-8.5557679050281E-15,-1.));
#39637=DIRECTION('',(-2.77102527463854E-15,-8.5557679050281E-15,-1.));
#39638=DIRECTION('center_axis',(-1.,-6.7618653731838E-14,2.77102527463912E-15));
#39639=DIRECTION('ref_axis',(-6.7618653731838E-14,1.,-8.55576790502791E-15));
#39640=DIRECTION('',(2.77102527463854E-15,8.5557679050281E-15,1.));
#39641=DIRECTION('',(6.7618653731838E-14,-1.,8.55576790502791E-15));
#39642=DIRECTION('',(2.77102527463854E-15,8.5557679050281E-15,1.));
#39643=DIRECTION('',(6.7618653731838E-14,-1.,8.55576790502791E-15));
#39644=DIRECTION('center_axis',(1.,6.7618653731838E-14,-2.77102527463912E-15));
#39645=DIRECTION('ref_axis',(6.7618653731838E-14,-1.,8.55576790502791E-15));
#39646=DIRECTION('center_axis',(1.,6.7618653731838E-14,-2.77102527463912E-15));
#39647=DIRECTION('ref_axis',(-2.77102527463861E-15,-7.46981590754665E-15,
-1.));
#39648=DIRECTION('center_axis',(1.,6.7618653731838E-14,-2.77102527463912E-15));
#39649=DIRECTION('ref_axis',(-2.77102527463832E-15,-1.18136238974724E-14,
-1.));
#39650=DIRECTION('',(-2.77102527463854E-15,-8.5557679050281E-15,-1.));
#39651=DIRECTION('center_axis',(-1.,-6.7618653731838E-14,2.77102527463912E-15));
#39652=DIRECTION('ref_axis',(-2.77102527463854E-15,-8.5557679050281E-15,
-1.));
#39653=DIRECTION('',(6.7618653731838E-14,-1.,8.55576790502791E-15));
#39654=DIRECTION('center_axis',(-1.,-6.7618653731838E-14,2.77102527463912E-15));
#39655=DIRECTION('ref_axis',(6.7618653731838E-14,-1.,5.64179671178602E-15));
#39656=DIRECTION('',(2.77102527463854E-15,8.5557679050281E-15,1.));
#39657=DIRECTION('center_axis',(-1.,-5.35487561816597E-14,-1.12988722755394E-14));
#39658=DIRECTION('ref_axis',(-1.12988722755392E-14,-4.55710246456112E-15,
1.));
#39659=DIRECTION('',(-6.7618653731838E-14,1.,-8.55576790502791E-15));
#39660=DIRECTION('center_axis',(-1.,-8.16885512820165E-14,-1.12988722755392E-14));
#39661=DIRECTION('ref_axis',(-8.16885512820165E-14,1.,3.1001168679395E-15));
#39662=DIRECTION('center_axis',(1.,6.7618653731838E-14,-2.77102527463912E-15));
#39663=DIRECTION('ref_axis',(-2.77102527463627E-15,-4.20664366273117E-14,
-1.));
#39664=DIRECTION('',(-1.,-6.7618653731838E-14,2.77102527463912E-15));
#39665=DIRECTION('center_axis',(-1.,-5.354875618166E-14,-1.12988722755392E-14));
#39666=DIRECTION('ref_axis',(1.12988722755397E-14,-8.55576790502718E-15,
-1.));
#39667=DIRECTION('',(-1.,-6.7618653731838E-14,2.77102527463912E-15));
#39668=DIRECTION('center_axis',(-2.77102527463854E-15,-8.5557679050281E-15,
-1.));
#39669=DIRECTION('ref_axis',(6.7618653731838E-14,-1.,8.55576790502791E-15));
#39670=DIRECTION('',(6.7618653731838E-14,-1.,8.55576790502791E-15));
#39671=DIRECTION('',(-1.,-6.7618653731838E-14,2.77102527463912E-15));
#39672=DIRECTION('center_axis',(1.,6.7618653731838E-14,-2.77102527463912E-15));
#39673=DIRECTION('ref_axis',(6.76186537318381E-14,-1.,4.06094510306894E-14));
#39674=DIRECTION('center_axis',(-1.,-8.16885512820162E-14,-1.12988722755389E-14));
#39675=DIRECTION('ref_axis',(8.16885512820161E-14,-1.,5.64179671178601E-15));
#39676=DIRECTION('',(-1.,-6.7618653731838E-14,2.77102527463912E-15));
#39677=DIRECTION('center_axis',(6.7618653731838E-14,-1.,8.55576790502791E-15));
#39678=DIRECTION('ref_axis',(2.77102527463854E-15,8.5557679050281E-15,1.));
#39679=DIRECTION('',(2.77102527463854E-15,8.5557679050281E-15,1.));
#39680=DIRECTION('',(-1.,-6.7618653731838E-14,2.77102527463912E-15));
#39681=DIRECTION('center_axis',(1.,6.7618653731838E-14,-2.77102527463912E-15));
#39682=DIRECTION('ref_axis',(2.77102527463864E-15,7.09878230840716E-15,
1.));
#39683=DIRECTION('center_axis',(-1.,-6.7618653731838E-14,2.77102527463912E-15));
#39684=DIRECTION('ref_axis',(2.77102527463943E-15,-4.5571024645602E-15,
1.));
#39685=DIRECTION('',(-1.,-6.7618653731838E-14,2.77102527463912E-15));
#39686=DIRECTION('center_axis',(2.77102527463854E-15,8.5557679050281E-15,
1.));
#39687=DIRECTION('ref_axis',(-6.7618653731838E-14,1.,-8.55576790502791E-15));
#39688=DIRECTION('',(-6.7618653731838E-14,1.,-8.55576790502791E-15));
#39689=DIRECTION('',(-1.,-6.7618653731838E-14,2.77102527463912E-15));
#39690=DIRECTION('center_axis',(1.,6.7618653731838E-14,-2.77102527463912E-15));
#39691=DIRECTION('ref_axis',(-6.7618653731838E-14,1.,-8.55576790502791E-15));
#39692=DIRECTION('center_axis',(-1.,-6.7618653731838E-14,2.77102527463912E-15));
#39693=DIRECTION('ref_axis',(-6.7618653731838E-14,1.,3.10011686793949E-15));
#39694=DIRECTION('',(-1.,-6.7618653731838E-14,2.77102527463912E-15));
#39695=DIRECTION('center_axis',(-6.7618653731838E-14,1.,-8.55576790502791E-15));
#39696=DIRECTION('ref_axis',(-2.77102527463854E-15,-8.5557679050281E-15,
-1.));
#39697=DIRECTION('',(-2.77102527463854E-15,-8.5557679050281E-15,-1.));
#39698=DIRECTION('center_axis',(1.,6.7618653731838E-14,-2.77102527463912E-15));
#39699=DIRECTION('ref_axis',(6.7618653731838E-14,-1.,8.55576790502791E-15));
#39700=DIRECTION('center_axis',(-6.99688737499255E-14,1.,0.));
#39701=DIRECTION('ref_axis',(0.,-8.7461092187406E-15,-1.));
#39702=DIRECTION('center_axis',(-1.,-6.7618653731838E-14,2.77102527463912E-15));
#39703=DIRECTION('ref_axis',(-2.77102527463869E-15,-6.38386391006521E-15,
-1.));
#39704=DIRECTION('center_axis',(6.51793608929021E-13,0.707106781186447,
-0.707106781186648));
#39705=DIRECTION('ref_axis',(0.896534794971466,-0.313229437797635,-0.313229437796719));
#39706=DIRECTION('center_axis',(4.00117890718912E-13,-0.707106781186849,
-0.707106781186247));
#39707=DIRECTION('ref_axis',(0.996198003956249,-0.0616016919958765,0.0616016919964927));
#39708=DIRECTION('center_axis',(-3.6704722266697E-13,-0.707106781186503,
0.707106781186592));
#39709=DIRECTION('ref_axis',(0.996921797515119,-0.0554388385488158,-0.0554388385482913));
#39710=DIRECTION('center_axis',(-5.26061948198612E-13,-0.707106781186484,
-0.707106781186611));
#39711=DIRECTION('ref_axis',(0.896534794971479,-0.31322943779752,0.313229437796797));
#39712=DIRECTION('center_axis',(9.18554053444912E-12,-0.707106781186299,
0.707106781186796));
#39713=DIRECTION('ref_axis',(0.996198003956234,0.0616016920027945,0.0616016919898103));
#39714=DIRECTION('center_axis',(4.75776948071443E-13,0.707106781186498,
0.707106781186597));
#39715=DIRECTION('ref_axis',(0.996921797515123,-0.0554388385488504,0.0554388385481719));
#39716=DIRECTION('center_axis',(7.70726635632004E-13,-0.707106781186425,
0.70710678118667));
#39717=DIRECTION('ref_axis',(0.896534794971449,0.313229437797744,0.313229437796658));
#39718=DIRECTION('center_axis',(9.23046358674266E-12,0.707106781186311,
0.707106781186784));
#39719=DIRECTION('ref_axis',(0.996198003956241,0.061601691989768,-0.061601692002731));
#39720=DIRECTION('center_axis',(-6.34411876251122E-13,0.707106781186469,
-0.707106781186626));
#39721=DIRECTION('ref_axis',(0.996921797515115,0.0554388385490345,0.0554388385481277));
#39722=DIRECTION('center_axis',(-6.56544319852163E-13,0.707106781186476,
0.707106781186619));
#39723=DIRECTION('ref_axis',(0.896534794971433,0.313229437797672,-0.313229437796776));
#39724=DIRECTION('center_axis',(2.14647884590057E-14,0.707106781186789,
-0.707106781186307));
#39725=DIRECTION('ref_axis',(0.996198003956254,-0.0616016919961379,-0.0616016919961496));
#39726=DIRECTION('center_axis',(5.78996367848738E-13,-0.707106781186491,
-0.707106781186604));
#39727=DIRECTION('ref_axis',(0.996921797515118,0.0554388385489725,-0.0554388385481474));
#39728=DIRECTION('center_axis',(1.,6.7618653731838E-14,-2.77102527463912E-15));
#39729=DIRECTION('ref_axis',(-2.77102527463847E-15,-9.64171990250954E-15,
-1.));
#39730=DIRECTION('',(-1.,-6.7618653731838E-14,2.77102527463912E-15));
#39731=DIRECTION('center_axis',(-6.99688737499273E-14,1.,0.));
#39732=DIRECTION('ref_axis',(0.,-8.74610921874091E-15,-1.));
#39733=DIRECTION('center_axis',(-1.,-6.32748457419122E-14,2.77102527463908E-15));
#39734=DIRECTION('ref_axis',(-2.77102527463847E-15,-9.64171990250955E-15,
-1.));
#39735=DIRECTION('center_axis',(2.22250656035605E-13,0.707106781186488,
-0.707106781186608));
#39736=DIRECTION('ref_axis',(0.896534794971443,-0.313229437797377,-0.313229437797042));
#39737=DIRECTION('center_axis',(1.17092005636022E-13,-0.707106781186556,
-0.707106781186539));
#39738=DIRECTION('ref_axis',(0.996198003956251,-0.0616016919960817,0.0616016919962482));
#39739=DIRECTION('center_axis',(3.08468140487006E-13,-0.707106781186592,
0.707106781186503));
#39740=DIRECTION('ref_axis',(0.99692179751513,-0.0554388385482297,-0.0554388385486716));
#39741=DIRECTION('center_axis',(2.19731246458362E-13,-0.707106781186608,
-0.707106781186487));
#39742=DIRECTION('ref_axis',(0.896534794971441,-0.313229437797046,0.313229437797379));
#39743=DIRECTION('center_axis',(6.15824789516204E-13,-0.707106781186494,
0.707106781186602));
#39744=DIRECTION('ref_axis',(0.996198003956225,0.0616016919968157,0.0616016919959387));
#39745=DIRECTION('center_axis',(-1.98029326998358E-14,0.707106781186549,
0.707106781186547));
#39746=DIRECTION('ref_axis',(0.996921797515125,-0.0554388385484832,0.0554388385485112));
#39747=DIRECTION('center_axis',(6.31015736015947E-14,-0.70710678118654,
0.707106781186555));
#39748=DIRECTION('ref_axis',(0.896534794971412,0.313229437797297,0.313229437797211));
#39749=DIRECTION('center_axis',(1.51175084320796E-12,0.707106781186554,
0.707106781186542));
#39750=DIRECTION('ref_axis',(0.996198003956232,0.061601691995254,-0.0616016919973848));
#39751=DIRECTION('center_axis',(8.47242099047219E-14,0.70710678118659,-0.707106781186506));
#39752=DIRECTION('ref_axis',(0.996921797515118,0.0554388385484938,0.0554388385486198));
#39753=DIRECTION('center_axis',(8.8643031429794E-14,0.707106781186602,0.707106781186494));
#39754=DIRECTION('ref_axis',(0.896534794971411,0.313229437797176,-0.313229437797336));
#39755=DIRECTION('center_axis',(1.95394423019618E-14,0.707106781186544,
-0.707106781186551));
#39756=DIRECTION('ref_axis',(0.996198003956246,-0.0616016919962189,-0.0616016919961908));
#39757=DIRECTION('center_axis',(2.04087760748626E-14,-0.707106781186559,
-0.707106781186536));
#39758=DIRECTION('ref_axis',(0.996921797515118,0.0554388385485753,-0.0554388385485483));
#39759=DIRECTION('center_axis',(1.,6.7618653731838E-14,-2.77102527463912E-15));
#39760=DIRECTION('ref_axis',(-2.77102527463854E-15,-8.5557679050281E-15,
-1.));
#39761=DIRECTION('',(-1.,-6.7618653731838E-14,2.77102527463912E-15));
#39762=DIRECTION('center_axis',(4.9773019351027E-14,-0.707106781186589,
0.707106781186506));
#39763=DIRECTION('ref_axis',(-4.58541978259481E-14,0.707106781186506,0.707106781186589));
#39764=DIRECTION('',(1.,6.7618653731838E-14,-2.77102527463912E-15));
#39765=DIRECTION('',(4.58541978259513E-14,-0.707106781186551,-0.707106781186544));
#39766=DIRECTION('',(1.,6.7618653731838E-14,-2.77102527463912E-15));
#39767=DIRECTION('center_axis',(-4.58541978259514E-14,0.707106781186553,
0.707106781186542));
#39768=DIRECTION('ref_axis',(-4.9773019351024E-14,0.707106781186542,-0.707106781186553));
#39769=DIRECTION('',(4.97730193510239E-14,-0.707106781186541,0.707106781186554));
#39770=DIRECTION('',(1.,6.7618653731838E-14,-2.77102527463912E-15));
#39771=DIRECTION('center_axis',(4.97730193510239E-14,-0.707106781186541,
0.707106781186554));
#39772=DIRECTION('ref_axis',(-4.58541978259515E-14,0.707106781186554,0.707106781186541));
#39773=DIRECTION('',(4.58541978259515E-14,-0.707106781186554,-0.707106781186541));
#39774=DIRECTION('',(1.,6.7618653731838E-14,-2.77102527463912E-15));
#39775=DIRECTION('center_axis',(-4.58541978259512E-14,0.707106781186549,
0.707106781186546));
#39776=DIRECTION('ref_axis',(-4.97730193510242E-14,0.707106781186546,-0.707106781186549));
#39777=DIRECTION('',(4.97730193510238E-14,-0.707106781186539,0.707106781186556));
#39778=DIRECTION('',(1.,6.7618653731838E-14,-2.77102527463912E-15));
#39779=DIRECTION('center_axis',(-4.97730193510225E-14,0.707106781186519,
-0.707106781186576));
#39780=DIRECTION('ref_axis',(4.58541978259531E-14,-0.707106781186576,-0.707106781186519));
#39781=DIRECTION('',(-4.585419782595E-14,0.707106781186533,0.707106781186562));
#39782=DIRECTION('',(1.,6.7618653731838E-14,-2.77102527463912E-15));
#39783=DIRECTION('center_axis',(-4.58541978259529E-14,0.707106781186574,
0.707106781186521));
#39784=DIRECTION('ref_axis',(-4.97730193510226E-14,0.707106781186521,-0.707106781186574));
#39785=DIRECTION('',(4.97730193510239E-14,-0.707106781186541,0.707106781186554));
#39786=DIRECTION('',(1.,6.7618653731838E-14,-2.77102527463912E-15));
#39787=DIRECTION('center_axis',(-4.97730193510239E-14,0.707106781186542,
-0.707106781186554));
#39788=DIRECTION('ref_axis',(4.58541978259515E-14,-0.707106781186554,-0.707106781186541));
#39789=DIRECTION('',(-4.58541978259481E-14,0.707106781186505,0.70710678118659));
#39790=DIRECTION('',(1.,6.7618653731838E-14,-2.77102527463912E-15));
#39791=DIRECTION('center_axis',(4.58541978259531E-14,-0.707106781186576,
-0.707106781186519));
#39792=DIRECTION('ref_axis',(4.97730193510225E-14,-0.707106781186519,0.707106781186576));
#39793=DIRECTION('',(-4.9773019351024E-14,0.707106781186542,-0.707106781186553));
#39794=DIRECTION('',(1.,6.7618653731838E-14,-2.77102527463912E-15));
#39795=DIRECTION('center_axis',(-4.97730193510253E-14,0.707106781186563,
-0.707106781186532));
#39796=DIRECTION('ref_axis',(4.585419782595E-14,-0.707106781186532,-0.707106781186563));
#39797=DIRECTION('',(-4.58541978259528E-14,0.707106781186573,0.707106781186522));
#39798=DIRECTION('',(1.,6.7618653731838E-14,-2.77102527463912E-15));
#39799=DIRECTION('center_axis',(4.58541978259515E-14,-0.707106781186554,
-0.707106781186542));
#39800=DIRECTION('ref_axis',(4.97730193510239E-14,-0.707106781186541,0.707106781186554));
#39801=DIRECTION('',(-4.97730193510206E-14,0.707106781186491,-0.707106781186604));
#39802=DIRECTION('',(1.,6.7618653731838E-14,-2.77102527463912E-15));
#39803=DIRECTION('center_axis',(4.97730193510253E-14,-0.707106781186562,
0.707106781186533));
#39804=DIRECTION('ref_axis',(-4.585419782595E-14,0.707106781186533,0.707106781186562));
#39805=DIRECTION('',(4.58541978259514E-14,-0.707106781186553,-0.707106781186542));
#39806=DIRECTION('',(1.,6.7618653731838E-14,-2.77102527463912E-15));
#39807=DIRECTION('center_axis',(4.58541978259515E-14,-0.707106781186554,
-0.707106781186542));
#39808=DIRECTION('ref_axis',(4.97730193510239E-14,-0.707106781186541,0.707106781186554));
#39809=DIRECTION('',(-4.97730193510239E-14,0.707106781186541,-0.707106781186554));
#39810=DIRECTION('center_axis',(1.,6.7618653731838E-14,-2.77102527463912E-15));
#39811=DIRECTION('ref_axis',(6.7618653731838E-14,-1.,8.55576790502791E-15));
#39812=DIRECTION('center_axis',(4.97730193510297E-14,-0.707106781186631,
0.707106781186464));
#39813=DIRECTION('ref_axis',(-4.58541978259452E-14,0.707106781186464,0.707106781186631));
#39814=DIRECTION('',(1.,6.7618653731838E-14,-2.77102527463912E-15));
#39815=DIRECTION('',(4.58541978259341E-14,-0.707106781186307,-0.707106781186788));
#39816=DIRECTION('',(1.,6.7618653731838E-14,-2.77102527463912E-15));
#39817=DIRECTION('center_axis',(-4.58541978259499E-14,0.707106781186531,
0.707106781186564));
#39818=DIRECTION('ref_axis',(-4.97730193510254E-14,0.707106781186564,-0.707106781186531));
#39819=DIRECTION('',(4.97730193510227E-14,-0.707106781186522,0.707106781186573));
#39820=DIRECTION('',(1.,6.7618653731838E-14,-2.77102527463912E-15));
#39821=DIRECTION('center_axis',(4.97730193510225E-14,-0.707106781186519,
0.707106781186576));
#39822=DIRECTION('ref_axis',(-4.58541978259531E-14,0.707106781186576,0.707106781186519));
#39823=DIRECTION('',(4.585419782595E-14,-0.707106781186532,-0.707106781186563));
#39824=DIRECTION('',(1.,6.7618653731838E-14,-2.77102527463912E-15));
#39825=DIRECTION('center_axis',(-4.58541978259578E-14,0.707106781186643,
0.707106781186452));
#39826=DIRECTION('ref_axis',(-4.97730193510181E-14,0.707106781186452,-0.707106781186643));
#39827=DIRECTION('',(4.97730193510079E-14,-0.707106781186295,0.7071067811868));
#39828=DIRECTION('',(1.,6.7618653731838E-14,-2.77102527463912E-15));
#39829=DIRECTION('center_axis',(-4.97730193510214E-14,0.707106781186502,
-0.707106781186593));
#39830=DIRECTION('ref_axis',(4.58541978259543E-14,-0.707106781186593,-0.707106781186502));
#39831=DIRECTION('',(-4.585419782595E-14,0.707106781186532,0.707106781186563));
#39832=DIRECTION('',(1.,6.7618653731838E-14,-2.77102527463912E-15));
#39833=DIRECTION('center_axis',(-4.58541978259487E-14,0.707106781186514,
0.707106781186581));
#39834=DIRECTION('ref_axis',(-4.97730193510265E-14,0.707106781186581,-0.707106781186514));
#39835=DIRECTION('',(4.97730193510225E-14,-0.70710678118652,0.707106781186575));
#39836=DIRECTION('',(1.,6.7618653731838E-14,-2.77102527463912E-15));
#39837=DIRECTION('center_axis',(-4.97730193510303E-14,0.707106781186639,
-0.707106781186456));
#39838=DIRECTION('ref_axis',(4.58541978259446E-14,-0.707106781186456,-0.707106781186639));
#39839=DIRECTION('',(-4.58541978259685E-14,0.707106781186796,0.707106781186299));
#39840=DIRECTION('',(1.,6.7618653731838E-14,-2.77102527463912E-15));
#39841=DIRECTION('center_axis',(4.58541978259488E-14,-0.707106781186515,
-0.70710678118658));
#39842=DIRECTION('ref_axis',(4.97730193510264E-14,-0.70710678118658,0.707106781186515));
#39843=DIRECTION('',(-4.97730193510223E-14,0.707106781186516,-0.707106781186579));
#39844=DIRECTION('',(1.,6.7618653731838E-14,-2.77102527463912E-15));
#39845=DIRECTION('center_axis',(-4.97730193510214E-14,0.707106781186502,
-0.707106781186593));
#39846=DIRECTION('ref_axis',(4.58541978259543E-14,-0.707106781186593,-0.707106781186502));
#39847=DIRECTION('',(-4.58541978259498E-14,0.70710678118653,0.707106781186565));
#39848=DIRECTION('',(1.,6.7618653731838E-14,-2.77102527463912E-15));
#39849=DIRECTION('center_axis',(4.58541978259616E-14,-0.707106781186697,
-0.707106781186398));
#39850=DIRECTION('ref_axis',(4.97730193510146E-14,-0.707106781186398,0.707106781186697));
#39851=DIRECTION('',(-4.97730193510397E-14,0.707106781186784,-0.707106781186311));
#39852=DIRECTION('',(1.,6.7618653731838E-14,-2.77102527463912E-15));
#39853=DIRECTION('center_axis',(4.97730193510213E-14,-0.707106781186501,
0.707106781186594));
#39854=DIRECTION('ref_axis',(-4.58541978259543E-14,0.707106781186594,0.707106781186501));
#39855=DIRECTION('',(4.585419782595E-14,-0.707106781186533,-0.707106781186562));
#39856=DIRECTION('',(1.,6.7618653731838E-14,-2.77102527463912E-15));
#39857=DIRECTION('center_axis',(3.16979723399869E-14,-0.707106781186513,
-0.707106781186582));
#39858=DIRECTION('ref_axis',(4.97730193510266E-14,-0.707106781186582,0.707106781186513));
#39859=DIRECTION('',(-4.97730193510212E-14,0.7071067811865,-0.707106781186595));
#39860=DIRECTION('center_axis',(1.,6.7618653731838E-14,-2.77102527463912E-15));
#39861=DIRECTION('ref_axis',(6.7618653731838E-14,-1.,8.55576790502791E-15));
#39862=DIRECTION('center_axis',(0.857167300702084,0.515038074910101,-6.78177848602247E-15));
#39863=DIRECTION('ref_axis',(-2.77102527463854E-15,-8.5557679050281E-15,
-1.));
#39864=DIRECTION('',(-2.77102527463854E-15,-8.5557679050281E-15,-1.));
#39865=DIRECTION('',(-0.515038074910099,0.857167300702085,-5.90654095760941E-15));
#39866=DIRECTION('',(2.77102527463854E-15,8.5557679050281E-15,1.));
#39867=DIRECTION('',(-0.515038074910089,0.857167300702092,-5.90654095760949E-15));
#39868=DIRECTION('',(2.77102527463854E-15,8.5557679050281E-15,1.));
#39869=DIRECTION('',(0.515038074910119,-0.857167300702073,5.90654095760925E-15));
#39870=DIRECTION('',(2.77102527463854E-15,8.5557679050281E-15,1.));
#39871=DIRECTION('',(0.515038074910127,-0.857167300702068,5.90654095760919E-15));
#39872=DIRECTION('',(-2.77102527463854E-15,-8.5557679050281E-15,-1.));
#39873=DIRECTION('center_axis',(-0.515038074910076,0.857167300702099,-5.90654095760959E-15));
#39874=DIRECTION('ref_axis',(-2.77102527463854E-15,-8.5557679050281E-15,
-1.));
#39875=DIRECTION('',(0.857167300702085,0.515038074910099,-6.78177848602246E-15));
#39876=DIRECTION('center_axis',(-2.77102527463854E-15,-8.5557679050281E-15,
-1.));
#39877=DIRECTION('ref_axis',(6.7618653731838E-14,-1.,8.55576790502791E-15));
#39878=DIRECTION('',(0.8571673007021,0.515038074910075,-6.78177848602229E-15));
#39879=DIRECTION('center_axis',(0.515038074910084,-0.857167300702094,5.90654095760953E-15));
#39880=DIRECTION('ref_axis',(2.77102527463854E-15,8.5557679050281E-15,1.));
#39881=DIRECTION('',(0.857167300702077,0.515038074910113,-6.78177848602255E-15));
#39882=DIRECTION('center_axis',(-2.77102527463854E-15,-8.5557679050281E-15,
-1.));
#39883=DIRECTION('ref_axis',(6.7618653731838E-14,-1.,8.55576790502791E-15));
#39884=DIRECTION('',(0.85716730070208,0.515038074910108,-6.78177848602252E-15));
#39885=DIRECTION('center_axis',(0.51503807491009,-0.857167300702091,5.90654095760948E-15));
#39886=DIRECTION('ref_axis',(2.77102527463854E-15,8.5557679050281E-15,1.));
#39887=DIRECTION('',(0.857167300702075,0.515038074910117,-6.78177848602258E-15));
#39888=DIRECTION('center_axis',(2.77102527463854E-15,8.5557679050281E-15,
1.));
#39889=DIRECTION('ref_axis',(-6.7618653731838E-14,1.,-8.55576790502791E-15));
#39890=DIRECTION('',(0.857167300702077,0.515038074910113,-6.78177848602255E-15));
#39891=DIRECTION('center_axis',(0.515038074910101,-0.857167300702084,5.90654095760939E-15));
#39892=DIRECTION('ref_axis',(2.77102527463854E-15,8.5557679050281E-15,1.));
#39893=DIRECTION('',(0.857167300702087,0.515038074910097,-6.78177848602244E-15));
#39894=DIRECTION('center_axis',(2.77102527463854E-15,8.5557679050281E-15,
1.));
#39895=DIRECTION('ref_axis',(-6.7618653731838E-14,1.,-8.55576790502791E-15));
#39896=DIRECTION('',(0.857167300702085,0.515038074910099,-6.78177848602246E-15));
#39897=DIRECTION('center_axis',(-0.515038074910086,0.857167300702093,-5.90654095760951E-15));
#39898=DIRECTION('ref_axis',(-2.77102527463854E-15,-8.5557679050281E-15,
-1.));
#39899=DIRECTION('center_axis',(-1.,-6.7618653731838E-14,2.77102527463912E-15));
#39900=DIRECTION('ref_axis',(2.7710252746386E-15,7.63556647558329E-15,1.));
#39901=DIRECTION('',(-1.,-6.7618653731838E-14,2.77102527463912E-15));
#39902=DIRECTION('',(1.,6.7618653731838E-14,-2.77102527463912E-15));
#39903=DIRECTION('center_axis',(-6.7618653731838E-14,1.,-8.55576790502791E-15));
#39904=DIRECTION('ref_axis',(-2.77102527463854E-15,-8.5557679050281E-15,
-1.));
#39905=DIRECTION('',(1.,6.7618653731838E-14,-2.77102527463912E-15));
#39906=DIRECTION('',(-2.77102527463854E-15,-8.5557679050281E-15,-1.));
#39907=DIRECTION('center_axis',(-2.77102527463854E-15,-8.5557679050281E-15,
-1.));
#39908=DIRECTION('ref_axis',(6.7618653731838E-14,-1.,8.55576790502791E-15));
#39909=DIRECTION('center_axis',(-3.95128286645425E-13,-2.33583808290282E-13,
-1.));
#39910=DIRECTION('ref_axis',(0.880460531975146,0.474119448698367,-4.58641487869712E-13));
#39911=DIRECTION('center_axis',(2.77102527463854E-15,8.5557679050281E-15,
1.));
#39912=DIRECTION('ref_axis',(-6.7618653731838E-14,1.,-8.55576790502791E-15));
#39913=DIRECTION('center_axis',(-4.70892792007641E-13,-2.56506629572123E-13,
1.));
#39914=DIRECTION('ref_axis',(0.856355995328812,0.516385911179227,5.3570827522798E-13));
#39915=DIRECTION('center_axis',(-1.,-6.7618653731838E-14,2.77102527463912E-15));
#39916=DIRECTION('ref_axis',(-2.77102527463854E-15,-8.5557679050281E-15,
-1.));
#39917=DIRECTION('',(1.,6.7618653731838E-14,-2.77102527463912E-15));
#39918=DIRECTION('',(-1.,-6.7618653731838E-14,2.77102527463912E-15));
#39919=DIRECTION('center_axis',(-2.77102527463854E-15,-8.5557679050281E-15,
-1.));
#39920=DIRECTION('ref_axis',(6.7618653731838E-14,-1.,8.55576790502791E-15));
#39921=DIRECTION('',(1.,6.7618653731838E-14,-2.77102527463912E-15));
#39922=DIRECTION('',(-1.,-6.7618653731838E-14,2.77102527463912E-15));
#39923=DIRECTION('center_axis',(2.59167743232149E-16,-1.01673529621644E-14,
-1.));
#39924=DIRECTION('ref_axis',(0.88885275239948,-0.458192955589529,4.88897146616111E-15));
#39925=DIRECTION('center_axis',(2.77102527463854E-15,8.5557679050281E-15,
1.));
#39926=DIRECTION('ref_axis',(-6.7618653731838E-14,1.,-8.55576790502791E-15));
#39927=DIRECTION('center_axis',(-1.02909387888083E-15,8.10142695923282E-15,
1.));
#39928=DIRECTION('ref_axis',(0.88885275239942,0.458192955589646,-2.7973038362239E-15));
#39929=DIRECTION('',(-1.,-6.7618653731838E-14,2.77102527463912E-15));
#39930=DIRECTION('',(1.,6.7618653731838E-14,-2.77102527463912E-15));
#39931=DIRECTION('center_axis',(-2.77102527463854E-15,-8.5557679050281E-15,
-1.));
#39932=DIRECTION('ref_axis',(6.7618653731838E-14,-1.,8.55576790502791E-15));
#39933=DIRECTION('center_axis',(5.00248153014182E-16,-2.81970907598089E-15,
-1.));
#39934=DIRECTION('ref_axis',(0.856355995328885,-0.516385911179105,1.88444854544628E-15));
#39935=DIRECTION('center_axis',(2.77102527463854E-15,8.5557679050281E-15,
1.));
#39936=DIRECTION('ref_axis',(-6.7618653731838E-14,1.,-8.55576790502791E-15));
#39937=DIRECTION('center_axis',(5.53379700565215E-13,-3.04189065102847E-13,
1.));
#39938=DIRECTION('ref_axis',(0.880460531975183,-0.474119448698298,-6.31450937390529E-13));
#39939=DIRECTION('',(1.,6.7618653731838E-14,-2.77102527463912E-15));
#39940=DIRECTION('center_axis',(6.7618653731838E-14,-1.,8.55576790502791E-15));
#39941=DIRECTION('ref_axis',(2.77102527463854E-15,8.5557679050281E-15,1.));
#39942=DIRECTION('',(2.77102527463854E-15,8.5557679050281E-15,1.));
#39943=DIRECTION('center_axis',(6.7618653731838E-14,-1.,8.55576790502791E-15));
#39944=DIRECTION('ref_axis',(2.77102527463854E-15,8.5557679050281E-15,1.));
#39945=DIRECTION('center_axis',(-6.74540619515736E-14,1.,-8.39117612476355E-15));
#39946=DIRECTION('ref_axis',(1.47128018848125E-14,-8.39117612476256E-15,
-1.));
#39947=DIRECTION('center_axis',(-6.7618653731838E-14,1.,-8.55576790502791E-15));
#39948=DIRECTION('ref_axis',(-2.77102527463854E-15,-8.5557679050281E-15,
-1.));
#39949=DIRECTION('center_axis',(0.515038074909993,0.857167300702149,-1.91875610040794E-14));
#39950=DIRECTION('ref_axis',(-2.80848657939479E-15,-2.06973404938391E-14,
-1.));
#39951=DIRECTION('',(0.857167300702153,-0.515038074909987,2.03131397634296E-15));
#39952=DIRECTION('',(-2.77102527463854E-15,-8.5557679050281E-15,-1.));
#39953=DIRECTION('',(0.857167300702159,-0.515038074909977,2.03131397634286E-15));
#39954=DIRECTION('center_axis',(2.77102527463854E-15,8.5557679050281E-15,
1.));
#39955=DIRECTION('ref_axis',(-6.7618653731838E-14,1.,-8.55576790502791E-15));
#39956=DIRECTION('',(0.515038074909973,0.857167300702161,-8.76090800356383E-15));
#39957=DIRECTION('',(0.857167300702151,-0.51503807490999,2.031313976343E-15));
#39958=DIRECTION('center_axis',(2.77102527463854E-15,8.5557679050281E-15,
1.));
#39959=DIRECTION('ref_axis',(-6.7618653731838E-14,1.,-8.55576790502791E-15));
#39960=DIRECTION('',(0.857167300702156,-0.515038074909982,2.03131397634291E-15));
#39961=DIRECTION('',(0.515038074909941,0.857167300702181,-8.76090800356391E-15));
#39962=DIRECTION('center_axis',(0.515038074909987,0.857167300702153,-8.7609080035638E-15));
#39963=DIRECTION('ref_axis',(-2.77102527463854E-15,-8.5557679050281E-15,
-1.));
#39964=DIRECTION('',(-2.77102527463854E-15,-8.5557679050281E-15,-1.));
#39965=DIRECTION('',(0.857167300702151,-0.51503807490999,2.031313976343E-15));
#39966=DIRECTION('center_axis',(-2.77102527463854E-15,-8.5557679050281E-15,
-1.));
#39967=DIRECTION('ref_axis',(6.7618653731838E-14,-1.,8.55576790502791E-15));
#39968=DIRECTION('',(-0.515038074909973,-0.857167300702161,8.76090800356383E-15));
#39969=DIRECTION('',(0.857167300702159,-0.515038074909977,2.03131397634286E-15));
#39970=DIRECTION('center_axis',(0.515038074909993,0.857167300702149,-8.76090800356378E-15));
#39971=DIRECTION('ref_axis',(-2.77102527463854E-15,-8.5557679050281E-15,
-1.));
#39972=DIRECTION('',(-2.77102527463854E-15,-8.5557679050281E-15,-1.));
#39973=DIRECTION('',(0.857167300702153,-0.515038074909987,2.03131397634296E-15));
#39974=DIRECTION('center_axis',(-2.77102527463854E-15,-8.5557679050281E-15,
-1.));
#39975=DIRECTION('ref_axis',(6.7618653731838E-14,-1.,8.55576790502791E-15));
#39976=DIRECTION('',(-0.515038074909941,-0.857167300702181,8.76090800356391E-15));
#39977=DIRECTION('',(0.857167300702156,-0.515038074909982,2.03131397634291E-15));
#39978=DIRECTION('center_axis',(-0.515038074910012,-0.857167300702138,8.76090800356374E-15));
#39979=DIRECTION('ref_axis',(2.77102527463854E-15,8.5557679050281E-15,1.));
#39980=DIRECTION('',(2.77102527463854E-15,8.5557679050281E-15,1.));
#39981=DIRECTION('',(0.857167300702159,-0.515038074909977,2.03131397634286E-15));
#39982=DIRECTION('center_axis',(-2.77102527463854E-15,-8.5557679050281E-15,
-1.));
#39983=DIRECTION('ref_axis',(6.7618653731838E-14,-1.,8.55576790502791E-15));
#39984=DIRECTION('',(-0.515038074909971,-0.857167300702162,8.76090800356383E-15));
#39985=DIRECTION('',(0.857167300702144,-0.515038074910001,2.03131397634311E-15));
#39986=DIRECTION('center_axis',(-0.51503807491001,-0.857167300702139,8.76090800356374E-15));
#39987=DIRECTION('ref_axis',(2.77102527463854E-15,8.5557679050281E-15,1.));
#39988=DIRECTION('',(2.77102527463854E-15,8.5557679050281E-15,1.));
#39989=DIRECTION('',(0.857167300702144,-0.515038074910001,2.03131397634311E-15));
#39990=DIRECTION('center_axis',(2.77102527463854E-15,8.5557679050281E-15,
1.));
#39991=DIRECTION('ref_axis',(-6.7618653731838E-14,1.,-8.55576790502791E-15));
#39992=DIRECTION('',(0.515038074909971,0.857167300702162,-8.76090800356383E-15));
#39993=DIRECTION('',(0.857167300702159,-0.515038074909977,2.03131397634286E-15));
#39994=DIRECTION('center_axis',(-6.7618653731838E-14,1.,-8.55576790502791E-15));
#39995=DIRECTION('ref_axis',(-2.77102527463854E-15,-8.5557679050281E-15,
-1.));
#39996=DIRECTION('',(-6.7618653731838E-14,1.,-8.55576790502791E-15));
#39997=DIRECTION('center_axis',(-6.6659342535235E-14,1.,-7.59645670842486E-15));
#39998=DIRECTION('ref_axis',(-1.,-6.6659342535235E-14,-2.79201063973172E-15));
#39999=DIRECTION('center_axis',(6.7618653731838E-14,-1.,8.55576790502791E-15));
#40000=DIRECTION('ref_axis',(2.77102527463854E-15,8.5557679050281E-15,1.));
#40001=DIRECTION('center_axis',(0.857167300702162,-0.515038074909972,2.03131397634281E-15));
#40002=DIRECTION('ref_axis',(2.77102527463854E-15,8.5557679050281E-15,1.));
#40003=DIRECTION('',(2.77102527463854E-15,8.5557679050281E-15,1.));
#40004=DIRECTION('center_axis',(-0.515038074910012,-0.857167300702138,8.76090800356374E-15));
#40005=DIRECTION('ref_axis',(2.77102527463854E-15,8.5557679050281E-15,1.));
#40006=DIRECTION('center_axis',(-7.09168149328414E-14,1.,0.));
#40007=DIRECTION('ref_axis',(0.,-8.86460186660509E-15,-1.));
#40008=DIRECTION('center_axis',(0.515038074910022,-0.857167300702132,-5.09723557356589E-14));
#40009=DIRECTION('ref_axis',(0.765900867954176,0.460199669632626,0.449012387955011));
#40010=DIRECTION('center_axis',(-3.34893569076932E-13,-1.94333589280781E-13,
1.));
#40011=DIRECTION('ref_axis',(0.808168976755105,0.588950681305834,3.85103492850293E-13));
#40012=DIRECTION('center_axis',(-0.515038074910272,0.857167300701981,-9.75530354987259E-14));
#40013=DIRECTION('ref_axis',(0.854456218440534,0.513409092344432,0.079471219107103));
#40014=DIRECTION('center_axis',(5.41438285992961E-14,6.29175671824922E-14,
1.));
#40015=DIRECTION('ref_axis',(0.534642392050907,0.84507840619796,-8.21178634335555E-14));
#40016=DIRECTION('center_axis',(-0.515038074910461,0.857167300701868,-5.90654095760654E-15));
#40017=DIRECTION('ref_axis',(0.853796957819265,0.513012968599682,-0.0885914717515699));
#40018=DIRECTION('center_axis',(4.86017780500163E-14,4.58060313724332E-14,
-1.));
#40019=DIRECTION('ref_axis',(0.813525514740932,0.581529222709832,6.61763323248973E-14));
#40020=DIRECTION('center_axis',(-0.515038074909955,0.857167300702172,-1.78183517834286E-14));
#40021=DIRECTION('ref_axis',(0.765900867954212,0.460199669632583,-0.449012387954995));
#40022=DIRECTION('center_axis',(-3.40435619625912E-13,-2.11445125090658E-13,
-1.));
#40023=DIRECTION('ref_axis',(0.899424938883873,0.437075255892783,-3.9861371853221E-13));
#40024=DIRECTION('center_axis',(0.515038074910064,-0.857167300702106,4.90124063835157E-14));
#40025=DIRECTION('ref_axis',(0.854456218440668,0.513409092344217,-0.0794712191070439));
#40026=DIRECTION('center_axis',(-2.77102527463854E-15,-8.5557679050281E-15,
-1.));
#40027=DIRECTION('ref_axis',(0.997159343857257,0.0753209330675436,-3.4075821663865E-15));
#40028=DIRECTION('center_axis',(0.857167300702092,0.515038074910088,-6.78177848602238E-15));
#40029=DIRECTION('ref_axis',(-2.77102527463854E-15,-8.5557679050281E-15,
-1.));
#40030=DIRECTION('',(-0.515038074910087,0.857167300702093,-5.90654095760951E-15));
#40031=DIRECTION('',(-2.77102527463854E-15,-8.5557679050281E-15,-1.));
#40032=DIRECTION('',(-0.515038074910099,0.857167300702085,-5.90654095760941E-15));
#40033=DIRECTION('',(2.77102527463854E-15,8.5557679050281E-15,1.));
#40034=DIRECTION('',(-0.515038074910089,0.857167300702092,-5.90654095760949E-15));
#40035=DIRECTION('',(2.77102527463854E-15,8.5557679050281E-15,1.));
#40036=DIRECTION('',(0.515038074910089,-0.857167300702092,5.90654095760949E-15));
#40037=DIRECTION('',(2.77102527463854E-15,8.5557679050281E-15,1.));
#40038=DIRECTION('',(0.515038074910057,-0.857167300702111,5.90654095760974E-15));
#40039=DIRECTION('',(-2.77102527463854E-15,-8.5557679050281E-15,-1.));
#40040=DIRECTION('center_axis',(-0.515038074910083,0.857167300702095,-5.90654095760954E-15));
#40041=DIRECTION('ref_axis',(-2.77102527463854E-15,-8.5557679050281E-15,
-1.));
#40042=DIRECTION('',(0.857167300702109,0.515038074910059,-6.78177848602218E-15));
#40043=DIRECTION('center_axis',(-2.77102527463854E-15,-8.5557679050281E-15,
-1.));
#40044=DIRECTION('ref_axis',(6.7618653731838E-14,-1.,8.55576790502791E-15));
#40045=DIRECTION('',(0.857167300702093,0.515038074910086,-6.78177848602236E-15));
#40046=DIRECTION('center_axis',(0.515038074910109,-0.85716730070208,5.90654095760933E-15));
#40047=DIRECTION('ref_axis',(2.77102527463854E-15,8.5557679050281E-15,1.));
#40048=DIRECTION('',(0.857167300702082,0.515038074910104,-6.78177848602249E-15));
#40049=DIRECTION('center_axis',(-2.77102527463854E-15,-8.5557679050281E-15,
-1.));
#40050=DIRECTION('ref_axis',(6.7618653731838E-14,-1.,8.55576790502791E-15));
#40051=DIRECTION('',(0.857167300702081,0.515038074910106,-6.7817784860225E-15));
#40052=DIRECTION('center_axis',(0.515038074910096,-0.857167300702087,5.90654095760943E-15));
#40053=DIRECTION('ref_axis',(2.77102527463854E-15,8.5557679050281E-15,1.));
#40054=DIRECTION('',(0.857167300702081,0.515038074910106,-6.7817784860225E-15));
#40055=DIRECTION('center_axis',(2.77102527463854E-15,8.5557679050281E-15,
1.));
#40056=DIRECTION('ref_axis',(-6.7618653731838E-14,1.,-8.55576790502791E-15));
#40057=DIRECTION('',(0.857167300702082,0.515038074910104,-6.78177848602249E-15));
#40058=DIRECTION('center_axis',(0.51503807491008,-0.857167300702097,5.90654095760956E-15));
#40059=DIRECTION('ref_axis',(2.77102527463854E-15,8.5557679050281E-15,1.));
#40060=DIRECTION('',(0.857167300702093,0.515038074910086,-6.78177848602236E-15));
#40061=DIRECTION('center_axis',(2.77102527463854E-15,8.5557679050281E-15,
1.));
#40062=DIRECTION('ref_axis',(-6.7618653731838E-14,1.,-8.55576790502791E-15));
#40063=DIRECTION('',(0.857167300702109,0.515038074910059,-6.78177848602218E-15));
#40064=DIRECTION('center_axis',(-0.515038074910084,0.857167300702095,-5.90654095760953E-15));
#40065=DIRECTION('ref_axis',(-2.77102527463854E-15,-8.5557679050281E-15,
-1.));
#40066=DIRECTION('',(0.857167300702087,0.515038074910096,-6.78177848602243E-15));
#40067=DIRECTION('center_axis',(2.77102527463854E-15,8.5557679050281E-15,
1.));
#40068=DIRECTION('ref_axis',(-6.7618653731838E-14,1.,-8.55576790502791E-15));
#40069=DIRECTION('center_axis',(-2.77102527463854E-15,-8.5557679050281E-15,
-1.));
#40070=DIRECTION('ref_axis',(6.7618653731838E-14,-1.,8.55576790502791E-15));
#40071=DIRECTION('center_axis',(-2.77102527463854E-15,-8.5557679050281E-15,
-1.));
#40072=DIRECTION('ref_axis',(-1.,-6.6598517921482E-14,2.77102527463911E-15));
#40073=DIRECTION('center_axis',(-2.77102527463854E-15,-8.5557679050281E-15,
-1.));
#40074=DIRECTION('ref_axis',(1.,6.78710947856367E-14,-2.77102527463912E-15));
#40075=DIRECTION('center_axis',(0.809016994374993,-0.58778525229241,1.31600269666953E-14));
#40076=DIRECTION('ref_axis',(-0.58778525229241,-0.809016994374993,8.55052942525792E-15));
#40077=DIRECTION('',(-0.809016994374993,0.587785252292411,-1.31600269666953E-14));
#40078=DIRECTION('center_axis',(-0.809016994375011,0.587785252292386,-4.7527885634039E-14));
#40079=DIRECTION('ref_axis',(-0.587785252292386,-0.809016994375011,-1.03345964395218E-13));
#40080=DIRECTION('center_axis',(-0.809016994375011,0.587785252292386,-4.7527885634039E-14));
#40081=DIRECTION('ref_axis',(-0.587785252292386,-0.809016994375011,-1.03345964395218E-13));
#40082=DIRECTION('center_axis',(6.7618653731838E-14,-1.,8.55576790502791E-15));
#40083=DIRECTION('ref_axis',(2.77102527463854E-15,8.5557679050281E-15,1.));
#40084=DIRECTION('center_axis',(-6.7618653731838E-14,1.,-8.55576790502791E-15));
#40085=DIRECTION('ref_axis',(-0.999999999999964,-6.76186560146574E-14,-2.66816709635331E-7));
#40086=DIRECTION('center_axis',(-6.7618653731838E-14,1.,-8.55576790502791E-15));
#40087=DIRECTION('ref_axis',(-0.999999999999964,-6.76186560146574E-14,-2.66816709635331E-7));
#40088=DIRECTION('center_axis',(-6.7618653731838E-14,1.,-8.55576790502791E-15));
#40089=DIRECTION('ref_axis',(1.,6.7618653731838E-14,-2.77102527463912E-15));
#40090=DIRECTION('',(6.7618653731838E-14,-1.,8.55576790502791E-15));
#40091=DIRECTION('center_axis',(6.76186537327884E-14,-1.,4.25205660328949E-15));
#40092=DIRECTION('ref_axis',(1.,6.76186537327884E-14,-2.77102527463912E-15));
#40093=DIRECTION('center_axis',(6.76186537327884E-14,-1.,4.25205660328949E-15));
#40094=DIRECTION('ref_axis',(1.,6.76186537327884E-14,-2.77102527463912E-15));
#40095=DIRECTION('center_axis',(0.8660254037839,0.500000000000933,-6.67766223488626E-15));
#40096=DIRECTION('ref_axis',(-2.77102527463854E-15,-8.5557679050281E-15,
-1.));
#40097=DIRECTION('center_axis',(-0.866025403783983,-0.500000000000789,1.25096941532722E-12));
#40098=DIRECTION('ref_axis',(5.94980265416061E-7,-1.03053354726044E-6,0.999999999999292));
#40099=DIRECTION('center_axis',(-0.866025403783983,-0.500000000000789,1.25096941532722E-12));
#40100=DIRECTION('ref_axis',(5.94980265416061E-7,-1.03053354726044E-6,0.999999999999292));
#40101=DIRECTION('center_axis',(-0.866025403784387,-0.500000000000089,4.3675291105943E-14));
#40102=DIRECTION('ref_axis',(-0.500000000000089,0.866025403784387,-6.02399971731799E-15));
#40103=DIRECTION('',(0.866025403784387,0.500000000000089,-4.3675291105943E-14));
#40104=DIRECTION('center_axis',(0.8660254037844,0.500000000000067,-1.42864757407154E-14));
#40105=DIRECTION('ref_axis',(-0.500000000000067,0.8660254037844,6.88713418504579E-15));
#40106=DIRECTION('center_axis',(1.36653725312799E-8,7.88970643311003E-9,
-1.));
#40107=DIRECTION('ref_axis',(0.49999999636864,-0.866025405881005,0.));
#40108=DIRECTION('center_axis',(-0.809016994376835,0.587785252289875,-2.78714765756024E-15));
#40109=DIRECTION('ref_axis',(-2.77102527463854E-15,-8.5557679050281E-15,
-1.));
#40110=DIRECTION('center_axis',(0.809016982702078,-0.587785268358799,-1.07442107896218E-9));
#40111=DIRECTION('ref_axis',(-2.68991140209819E-13,-1.82828450322239E-9,
1.));
#40112=DIRECTION('center_axis',(0.809016982702078,-0.587785268358799,-1.07442107896218E-9));
#40113=DIRECTION('ref_axis',(-2.68991140209819E-13,-1.82828450322239E-9,
1.));
#40114=DIRECTION('center_axis',(-0.587785268327129,-0.809016982725088,-1.31521403548603E-9));
#40115=DIRECTION('ref_axis',(-4.97129381068598E-15,1.6256975880891E-9,-1.));
#40116=DIRECTION('center_axis',(-1.,-2.90861433570666E-10,4.9713238625083E-15));
#40117=DIRECTION('ref_axis',(4.97129381117057E-15,1.03318399277558E-10,
1.));
#40118=DIRECTION('center_axis',(-2.94928246063151E-15,-8.30841608127262E-15,
-1.));
#40119=DIRECTION('ref_axis',(6.8138088415828E-14,-1.,7.50144092651318E-15));
#40120=DIRECTION('center_axis',(-2.77102527463857E-15,-8.1650678567722E-15,
-1.));
#40121=DIRECTION('ref_axis',(-1.,-6.65985179156601E-14,2.77102527463911E-15));
#40122=DIRECTION('center_axis',(-2.77102527463857E-15,-8.1650678567722E-15,
-1.));
#40123=DIRECTION('ref_axis',(-1.,-6.65985179156601E-14,2.77102527463911E-15));
#40124=DIRECTION('center_axis',(1.,6.75911083482698E-14,-2.94928246063208E-15));
#40125=DIRECTION('ref_axis',(-6.75911083482698E-14,1.,-7.81400096511789E-15));
#40126=DIRECTION('center_axis',(-2.77102527463854E-15,-8.5557679050281E-15,
-1.));
#40127=DIRECTION('ref_axis',(1.,6.89554556095436E-14,-2.77102527463913E-15));
#40128=DIRECTION('center_axis',(2.77102527463854E-15,8.56804070208913E-15,
1.));
#40129=DIRECTION('ref_axis',(-1.,-6.75495870696371E-14,2.77102527463912E-15));
#40130=DIRECTION('',(-2.77102527463854E-15,-8.56804070208913E-15,-1.));
#40131=DIRECTION('center_axis',(2.77102527463854E-15,8.5557679050281E-15,
1.));
#40132=DIRECTION('ref_axis',(-6.7618653731838E-14,1.,-8.55576790502791E-15));
#40133=DIRECTION('center_axis',(-2.77102527463854E-15,-8.5557679050281E-15,
-1.));
#40134=DIRECTION('ref_axis',(6.7618653731838E-14,-1.,8.55576790502791E-15));
#40135=DIRECTION('center_axis',(-2.77102527463854E-15,-8.5557679050281E-15,
-1.));
#40136=DIRECTION('ref_axis',(-1.,-6.55943646399812E-14,2.7710252746391E-15));
#40137=DIRECTION('center_axis',(2.77102527463854E-15,8.5680407190582E-15,
1.));
#40138=DIRECTION('ref_axis',(1.,6.75429236703742E-14,-2.77102527463912E-15));
#40139=DIRECTION('',(-2.77102527463854E-15,-8.5680407190582E-15,-1.));
#40140=DIRECTION('center_axis',(-2.77102527463854E-15,-8.5557679050281E-15,
-1.));
#40141=DIRECTION('ref_axis',(0.813826036051037,0.581108581114973,-7.22696266269622E-15));
#40142=DIRECTION('center_axis',(-2.77102527463854E-15,-8.5557679050281E-15,
-1.));
#40143=DIRECTION('ref_axis',(0.813826036051037,0.581108581114973,-7.22696266269622E-15));
#40144=DIRECTION('center_axis',(-6.7618653731838E-14,1.,-8.55576790502791E-15));
#40145=DIRECTION('ref_axis',(-2.77102527463854E-15,-8.5557679050281E-15,
-1.));
#40146=DIRECTION('center_axis',(-6.54569677098685E-14,1.,-5.02820377450251E-15));
#40147=DIRECTION('ref_axis',(-0.504155551068663,-3.73429150937775E-14,-0.8636128648455));
#40148=DIRECTION('',(-2.77102527463854E-15,-8.5557679050281E-15,-1.));
#40149=DIRECTION('',(-1.,-6.7618653731838E-14,2.77102527463912E-15));
#40150=DIRECTION('',(-2.77102527463854E-15,-8.5557679050281E-15,-1.));
#40151=DIRECTION('center_axis',(-2.77102527463854E-15,-8.5557679050281E-15,
-1.));
#40152=DIRECTION('ref_axis',(6.7618653731838E-14,-1.,8.55576790502791E-15));
#40153=DIRECTION('',(-6.7618653731838E-14,1.,-8.55576790502791E-15));
#40154=DIRECTION('',(1.,6.7618653731838E-14,-2.77102527463912E-15));
#40155=DIRECTION('',(0.707106781186496,0.707106781186599,-8.00925226644011E-15));
#40156=DIRECTION('',(-6.7618653731838E-14,1.,-8.55576790502791E-15));
#40157=DIRECTION('',(1.,6.7618653731838E-14,-2.77102527463912E-15));
#40158=DIRECTION('',(6.7618653731838E-14,-1.,8.55576790502791E-15));
#40159=DIRECTION('',(0.707106781186597,-0.707106781186498,4.0904307413668E-15));
#40160=DIRECTION('',(1.,6.90094127104307E-14,-2.77102527463913E-15));
#40161=DIRECTION('',(6.7618653731838E-14,-1.,8.55576790502791E-15));
#40162=DIRECTION('',(-1.,-6.7618653731838E-14,2.77102527463912E-15));
#40163=DIRECTION('',(-0.707106781186496,-0.707106781186599,8.00925226644011E-15));
#40164=DIRECTION('',(6.7618653731838E-14,-1.,8.55576790502791E-15));
#40165=DIRECTION('',(-1.,-6.7618653731838E-14,2.77102527463912E-15));
#40166=DIRECTION('',(-6.7618653731838E-14,1.,-8.55576790502791E-15));
#40167=DIRECTION('',(-0.707106781186595,0.7071067811865,-4.09043074136683E-15));
#40168=DIRECTION('center_axis',(0.707106781186496,0.707106781186599,-8.19011459861798E-15));
#40169=DIRECTION('ref_axis',(-2.76568749322768E-15,-8.8168836495273E-15,
-1.));
#40170=DIRECTION('center_axis',(0.70710678118651,0.707106781186585,2.01699480869601E-13));
#40171=DIRECTION('ref_axis',(-0.0672249759424576,0.0672249759427345,-0.995470544626527));
#40172=DIRECTION('',(-2.77102527463816E-15,-1.41116436776427E-14,-1.));
#40173=DIRECTION('center_axis',(-6.7618653731838E-14,1.,-8.55576790502791E-15));
#40174=DIRECTION('ref_axis',(-2.77102527463854E-15,-8.5557679050281E-15,
-1.));
#40175=DIRECTION('',(2.77102527463854E-15,8.5557679050281E-15,1.));
#40176=DIRECTION('',(-1.,-6.7618653731838E-14,2.77102527463912E-15));
#40177=DIRECTION('',(-2.77102527463854E-15,-8.5557679050281E-15,-1.));
#40178=DIRECTION('',(1.,6.7618653731838E-14,-2.77102527463912E-15));
#40179=DIRECTION('',(2.77102527463854E-15,8.5557679050281E-15,1.));
#40180=DIRECTION('',(-1.,-6.7618653731838E-14,2.77102527463912E-15));
#40181=DIRECTION('center_axis',(6.7618653731838E-14,-1.,8.55576790502791E-15));
#40182=DIRECTION('ref_axis',(2.77102527463854E-15,8.5557679050281E-15,1.));
#40183=DIRECTION('',(2.77102527463854E-15,8.5557679050281E-15,1.));
#40184=DIRECTION('',(1.,6.7618653731838E-14,-2.77102527463912E-15));
#40185=DIRECTION('',(2.77102527463854E-15,8.5557679050281E-15,1.));
#40186=DIRECTION('',(1.,6.7618653731838E-14,-2.77102527463912E-15));
#40187=DIRECTION('',(2.77102527463854E-15,8.5557679050281E-15,1.));
#40188=DIRECTION('',(-1.,-6.7618653731838E-14,2.77102527463912E-15));
#40189=DIRECTION('center_axis',(-2.77102527463854E-15,-8.5557679050281E-15,
-1.));
#40190=DIRECTION('ref_axis',(6.7618653731838E-14,-1.,8.55576790502791E-15));
#40191=DIRECTION('',(-1.,-6.7618653731838E-14,2.77102527463912E-15));
#40192=DIRECTION('center_axis',(7.2574015725158E-16,-8.55576790502786E-15,
-1.));
#40193=DIRECTION('ref_axis',(-5.97509315100852E-14,1.,-8.5557679050279E-15));
#40194=DIRECTION('',(1.,6.7618653731838E-14,-2.77102527463912E-15));
#40195=DIRECTION('center_axis',(4.22250558914198E-15,-8.55576790502776E-15,
-1.));
#40196=DIRECTION('ref_axis',(7.8983141385481E-14,-1.,8.5557679050281E-15));
#40197=DIRECTION('center_axis',(-6.91127211940769E-15,-8.55576790502838E-15,
-1.));
#40198=DIRECTION('ref_axis',(0.811429434660002,0.584450402144912,-1.06084316213848E-14));
#40199=DIRECTION('',(1.,6.7618653731838E-14,-2.77102527463912E-15));
#40200=DIRECTION('center_axis',(9.18710863590449E-15,8.55576790502796E-15,
1.));
#40201=DIRECTION('ref_axis',(9.5991471980432E-14,1.,-8.55576790502884E-15));
#40202=DIRECTION('',(-1.,-6.7618653731838E-14,2.77102527463912E-15));
#40203=DIRECTION('center_axis',(-2.8074595126898E-15,-8.5557679050281E-15,
-1.));
#40204=DIRECTION('ref_axis',(-5.53799747202225E-14,1.,-8.55576790502794E-15));
#40205=DIRECTION('center_axis',(2.77102527463854E-15,8.5557679050281E-15,
1.));
#40206=DIRECTION('ref_axis',(-1.86639376853759E-14,1.,-8.55576790502804E-15));
#40207=DIRECTION('',(2.77102527463854E-15,8.5557679050281E-15,1.));
#40208=DIRECTION('',(2.77102527463854E-15,8.5557679050281E-15,1.));
#40209=DIRECTION('center_axis',(-6.7618653731838E-14,1.,-8.55576790502791E-15));
#40210=DIRECTION('ref_axis',(-2.77102527463854E-15,-8.5557679050281E-15,
-1.));
#40211=DIRECTION('',(-1.,-6.7618653731838E-14,2.77102527463912E-15));
#40212=DIRECTION('',(2.77102527463854E-15,8.5557679050281E-15,1.));
#40213=DIRECTION('center_axis',(-2.8074595126898E-15,-8.5557679050281E-15,
-1.));
#40214=DIRECTION('ref_axis',(6.58702710158929E-14,-1.,8.55576790502791E-15));
#40215=DIRECTION('center_axis',(6.26779070652866E-15,8.55576790502833E-15,
1.));
#40216=DIRECTION('ref_axis',(7.72347586695359E-14,-1.,8.55576790502785E-15));
#40217=DIRECTION('',(2.77102527463854E-15,8.5557679050281E-15,1.));
#40218=DIRECTION('center_axis',(6.7618653731838E-14,-1.,8.55576790502791E-15));
#40219=DIRECTION('ref_axis',(2.77102527463854E-15,8.5557679050281E-15,1.));
#40220=DIRECTION('',(1.,6.7618653731838E-14,-2.77102527463912E-15));
#40221=DIRECTION('center_axis',(-2.77102527463854E-15,-8.5557679050281E-15,
-1.));
#40222=DIRECTION('ref_axis',(6.7618653731838E-14,-1.,8.55576790502791E-15));
#40223=DIRECTION('',(-1.,-6.7618653731838E-14,2.77102527463912E-15));
#40224=DIRECTION('center_axis',(7.257401572517E-16,-8.55576790502786E-15,
-1.));
#40225=DIRECTION('ref_axis',(-6.41218882999477E-14,1.,-8.55576790502791E-15));
#40226=DIRECTION('',(1.,6.7618653731838E-14,-2.77102527463912E-15));
#40227=DIRECTION('center_axis',(-2.77102527463854E-15,-8.5557679050281E-15,
-1.));
#40228=DIRECTION('ref_axis',(6.84928450898106E-14,-1.,8.55576790502791E-15));
#40229=DIRECTION('center_axis',(-5.4767989042709E-15,-1.05258846015543E-14,
-1.));
#40230=DIRECTION('ref_axis',(1.,6.07633997852702E-14,-5.47679890427154E-15));
#40231=DIRECTION('center_axis',(9.18710863590508E-15,8.55576790502853E-15,
1.));
#40232=DIRECTION('ref_axis',(6.44106120512047E-14,-1.,8.55576790502794E-15));
#40233=DIRECTION('center_axis',(-2.80745343291974E-15,-8.5557679050281E-15,
-1.));
#40234=DIRECTION('ref_axis',(-6.7618653731838E-14,1.,-8.55576790502791E-15));
#40235=DIRECTION('center_axis',(2.77102527463854E-15,8.5557679050281E-15,
1.));
#40236=DIRECTION('ref_axis',(-6.67444623738654E-14,1.,-8.55576790502791E-15));
#40237=DIRECTION('',(2.77102527463854E-15,8.5557679050281E-15,1.));
#40238=DIRECTION('',(2.77102527463854E-15,8.5557679050281E-15,1.));
#40239=DIRECTION('center_axis',(-6.7618653731838E-14,1.,-8.55576790502791E-15));
#40240=DIRECTION('ref_axis',(-2.77102527463854E-15,-8.5557679050281E-15,
-1.));
#40241=DIRECTION('',(-1.,-6.7618653731838E-14,2.77102527463912E-15));
#40242=DIRECTION('',(2.77102527463854E-15,8.5557679050281E-15,1.));
#40243=DIRECTION('center_axis',(-2.8074592087013E-15,-8.5557679050281E-15,
-1.));
#40244=DIRECTION('ref_axis',(6.7618653731838E-14,-1.,8.55576790502791E-15));
#40245=DIRECTION('center_axis',(6.2677907065288E-15,8.55576790502833E-15,
1.));
#40246=DIRECTION('ref_axis',(6.7618653731838E-14,-1.,8.55576790502791E-15));
#40247=DIRECTION('',(2.77102527463854E-15,8.5557679050281E-15,1.));
#40248=DIRECTION('center_axis',(6.7618653731838E-14,-1.,8.55576790502791E-15));
#40249=DIRECTION('ref_axis',(2.77102527463854E-15,8.5557679050281E-15,1.));
#40250=DIRECTION('',(1.,6.7618653731838E-14,-2.77102527463912E-15));
#40251=DIRECTION('center_axis',(-2.77102527463854E-15,-8.5557679050281E-15,
-1.));
#40252=DIRECTION('ref_axis',(6.7618653731838E-14,-1.,8.55576790502791E-15));
#40253=DIRECTION('center_axis',(2.77102527463839E-15,1.08315670797044E-14,
1.));
#40254=DIRECTION('ref_axis',(1.,9.26524446532782E-14,-2.77102527463939E-15));
#40255=DIRECTION('center_axis',(-2.77102527463854E-15,-8.5557679050281E-15,
-1.));
#40256=DIRECTION('ref_axis',(1.,6.7618653731838E-14,-2.77102527463912E-15));
#40257=DIRECTION('',(-2.77102527463854E-15,-8.5557679050281E-15,-1.));
#40258=DIRECTION('center_axis',(2.77102527463885E-15,4.00416955567546E-15,
1.));
#40259=DIRECTION('ref_axis',(1.,9.26524446532782E-14,-2.77102527463922E-15));
#40260=DIRECTION('center_axis',(2.77102527463885E-15,4.00416955567546E-15,
1.));
#40261=DIRECTION('ref_axis',(1.,9.26524446532782E-14,-2.77102527463922E-15));
#40262=DIRECTION('center_axis',(1.53398371455475E-14,1.40986148553614E-14,
-1.));
#40263=DIRECTION('ref_axis',(-0.813826036051091,0.581108581114896,-4.29113278354576E-15));
#40264=DIRECTION('',(0.575461908797923,-0.410905818312039,-0.707106781186522));
#40265=DIRECTION('center_axis',(2.77102527463854E-15,8.5557679050281E-15,
1.));
#40266=DIRECTION('ref_axis',(-0.813826036051116,0.581108581114861,-2.71669763258241E-15));
#40267=DIRECTION('center_axis',(-2.77102527463854E-15,-8.5557679050281E-15,
-1.));
#40268=DIRECTION('ref_axis',(6.7618653731838E-14,-1.,8.55576790502791E-15));
#40269=DIRECTION('center_axis',(2.77102527463839E-15,1.08315670797045E-14,
1.));
#40270=DIRECTION('ref_axis',(1.,6.7618653731838E-14,-2.77102527463912E-15));
#40271=DIRECTION('center_axis',(-2.77102527463854E-15,-8.5557679050281E-15,
-1.));
#40272=DIRECTION('ref_axis',(1.,6.7618653731838E-14,-2.77102527463912E-15));
#40273=DIRECTION('',(-2.77102527463854E-15,-8.5557679050281E-15,-1.));
#40274=DIRECTION('center_axis',(2.77102527463885E-15,4.00416955567534E-15,
1.));
#40275=DIRECTION('ref_axis',(1.,6.7618653731838E-14,-2.77102527463912E-15));
#40276=DIRECTION('center_axis',(2.77102527463885E-15,4.00416955567534E-15,
1.));
#40277=DIRECTION('ref_axis',(1.,6.7618653731838E-14,-2.77102527463912E-15));
#40278=DIRECTION('center_axis',(-4.42416735431458E-15,-5.558773389224E-15,
-1.));
#40279=DIRECTION('ref_axis',(-0.813826036051113,0.581108581114866,3.7025166383754E-16));
#40280=DIRECTION('',(0.575461908797911,-0.410905818312022,-0.707106781186542));
#40281=DIRECTION('center_axis',(2.77102527463854E-15,8.5557679050281E-15,
1.));
#40282=DIRECTION('ref_axis',(-0.813826036051116,0.581108581114862,-2.71669763258241E-15));
#40283=DIRECTION('center_axis',(-2.77102527463854E-15,-8.5557679050281E-15,
-1.));
#40284=DIRECTION('ref_axis',(6.7618653731838E-14,-1.,8.55576790502791E-15));
#40285=DIRECTION('center_axis',(2.77102527463839E-15,1.08315670797045E-14,
1.));
#40286=DIRECTION('ref_axis',(1.,5.39638586837799E-14,-2.77102527463897E-15));
#40287=DIRECTION('center_axis',(-2.77102527463854E-15,-8.5557679050281E-15,
-1.));
#40288=DIRECTION('ref_axis',(1.,6.7618653731838E-14,-2.77102527463912E-15));
#40289=DIRECTION('',(-2.77102527463854E-15,-8.5557679050281E-15,-1.));
#40290=DIRECTION('center_axis',(2.77102527463885E-15,4.00416955567533E-15,
1.));
#40291=DIRECTION('ref_axis',(1.,5.39638586837799E-14,-2.77102527463906E-15));
#40292=DIRECTION('center_axis',(2.77102527463885E-15,4.00416955567533E-15,
1.));
#40293=DIRECTION('ref_axis',(1.,5.39638586837799E-14,-2.77102527463906E-15));
#40294=DIRECTION('center_axis',(-3.54887986328151E-14,-8.22998747375855E-15,
-1.));
#40295=DIRECTION('ref_axis',(-0.813826036051127,0.581108581114846,2.40991919720918E-14));
#40296=DIRECTION('',(0.575461908797904,-0.410905818312013,-0.707106781186553));
#40297=DIRECTION('center_axis',(2.77102527463854E-15,8.5557679050281E-15,
1.));
#40298=DIRECTION('ref_axis',(-0.813826036051116,0.581108581114862,-2.71669763258241E-15));
#40299=DIRECTION('center_axis',(-2.77102527463854E-15,-8.5557679050281E-15,
-1.));
#40300=DIRECTION('ref_axis',(6.7618653731838E-14,-1.,8.55576790502791E-15));
#40301=DIRECTION('center_axis',(2.77102527463839E-15,1.08315670797045E-14,
1.));
#40302=DIRECTION('ref_axis',(1.,6.7618653731838E-14,-2.77102527463912E-15));
#40303=DIRECTION('center_axis',(-2.77102527463854E-15,-8.5557679050281E-15,
-1.));
#40304=DIRECTION('ref_axis',(1.,6.7618653731838E-14,-2.77102527463912E-15));
#40305=DIRECTION('',(-2.77102527463854E-15,-8.5557679050281E-15,-1.));
#40306=DIRECTION('center_axis',(2.77102527463885E-15,4.00416955567534E-15,
1.));
#40307=DIRECTION('ref_axis',(1.,6.7618653731838E-14,-2.77102527463912E-15));
#40308=DIRECTION('center_axis',(2.77102527463885E-15,4.00416955567534E-15,
1.));
#40309=DIRECTION('ref_axis',(1.,6.7618653731838E-14,-2.77102527463912E-15));
#40310=DIRECTION('center_axis',(-1.05735999988311E-15,-6.40139923879278E-15,
-1.));
#40311=DIRECTION('ref_axis',(-0.813826036051111,0.581108581114868,-2.8594009314208E-15));
#40312=DIRECTION('',(0.575461908797912,-0.410905818312024,-0.70710678118654));
#40313=DIRECTION('center_axis',(2.77102527463854E-15,8.5557679050281E-15,
1.));
#40314=DIRECTION('ref_axis',(-0.813826036051116,0.581108581114861,-2.71669763258241E-15));
#40315=DIRECTION('center_axis',(3.09929612963862E-15,8.6194655394995E-15,
1.));
#40316=DIRECTION('ref_axis',(0.813826036051036,0.581108581114974,-7.53113327336009E-15));
#40317=DIRECTION('',(0.0142032227504033,0.0101417431418033,-0.999847695156391));
#40318=DIRECTION('center_axis',(-2.87643042720314E-15,-8.58953731699573E-15,
-1.));
#40319=DIRECTION('ref_axis',(0.813826036051037,0.581108581114972,-7.33236781526082E-15));
#40320=DIRECTION('center_axis',(-2.77102527463854E-15,-8.5557679050281E-15,
-1.));
#40321=DIRECTION('ref_axis',(6.7618653731838E-14,-1.,8.55576790502791E-15));
#40322=DIRECTION('center_axis',(2.77102527463854E-15,8.5557679050281E-15,
1.));
#40323=DIRECTION('ref_axis',(-1.,-5.54559913600458E-14,2.77102527463901E-15));
#40324=DIRECTION('center_axis',(2.7710252746384E-15,1.05828783003268E-14,
1.));
#40325=DIRECTION('ref_axis',(1.,6.64679041229712E-14,-2.77102527463911E-15));
#40326=DIRECTION('center_axis',(-2.7710252746384E-15,-1.05828783003268E-14,
-1.));
#40327=DIRECTION('ref_axis',(-1.,-6.80361564334454E-14,2.77102527463912E-15));
#40328=DIRECTION('center_axis',(2.7710252746384E-15,1.05828783003268E-14,
1.));
#40329=DIRECTION('ref_axis',(1.,7.16728745224354E-14,-2.77102527463916E-15));
#40330=DIRECTION('center_axis',(-2.77102527463852E-15,-8.8665914989739E-15,
-1.));
#40331=DIRECTION('ref_axis',(-1.,-6.68051934319591E-14,2.77102527463911E-15));
#40332=DIRECTION('center_axis',(2.77102527463854E-15,8.56804086924424E-15,
1.));
#40333=DIRECTION('ref_axis',(-1.,-6.76736001032872E-14,2.77102527463912E-15));
#40334=DIRECTION('',(-2.77102527463854E-15,-8.56804086924424E-15,-1.));
#40335=DIRECTION('center_axis',(-2.77102527463852E-15,-8.8665914989739E-15,
-1.));
#40336=DIRECTION('ref_axis',(-1.,-6.68051935153285E-14,2.77102527463911E-15));
#40337=DIRECTION('center_axis',(-2.77102527463854E-15,-8.5557679050281E-15,
-1.));
#40338=DIRECTION('ref_axis',(6.7618653731838E-14,-1.,8.55576790502791E-15));
#40339=DIRECTION('center_axis',(-2.77102527463852E-15,-8.89443768051384E-15,
-1.));
#40340=DIRECTION('ref_axis',(-1.,-6.69412911079351E-14,2.77102527463911E-15));
#40341=DIRECTION('center_axis',(2.77102527463854E-15,8.56804054497893E-15,
1.));
#40342=DIRECTION('ref_axis',(-1.,-6.75587848041088E-14,2.77102527463912E-15));
#40343=DIRECTION('',(2.77102527463854E-15,8.56804054497893E-15,1.));
#40344=DIRECTION('center_axis',(-2.77102527463852E-15,-8.89443768051384E-15,
-1.));
#40345=DIRECTION('ref_axis',(-1.,-6.69412911079351E-14,2.77102527463911E-15));
#40346=DIRECTION('center_axis',(-2.77102527463854E-15,-8.5557679050281E-15,
-1.));
#40347=DIRECTION('ref_axis',(6.7618653731838E-14,-1.,8.55576790502791E-15));
#40348=DIRECTION('center_axis',(-2.77102527463845E-15,-9.91373506304373E-15,
-1.));
#40349=DIRECTION('ref_axis',(-1.,-6.57708935439301E-14,2.7710252746391E-15));
#40350=DIRECTION('center_axis',(2.77102527463854E-15,8.56804088631084E-15,
1.));
#40351=DIRECTION('ref_axis',(-1.,-6.74986252505169E-14,2.77102527463912E-15));
#40352=DIRECTION('',(-2.77102527463854E-15,-8.56804088631084E-15,-1.));
#40353=DIRECTION('center_axis',(-2.77102527463845E-15,-9.91373506304373E-15,
-1.));
#40354=DIRECTION('ref_axis',(-1.,-6.60304235712797E-14,2.7710252746391E-15));
#40355=DIRECTION('center_axis',(-2.77102527463854E-15,-8.5557679050281E-15,
-1.));
#40356=DIRECTION('ref_axis',(6.7618653731838E-14,-1.,8.55576790502791E-15));
#40357=DIRECTION('center_axis',(-2.77102527463844E-15,-9.983019101718E-15,
-1.));
#40358=DIRECTION('ref_axis',(-1.,-6.60243977496101E-14,2.7710252746391E-15));
#40359=DIRECTION('center_axis',(2.77102527463854E-15,8.55745189714029E-15,
1.));
#40360=DIRECTION('ref_axis',(-1.,-6.74925013484086E-14,2.77102527463912E-15));
#40361=DIRECTION('',(2.77102527463854E-15,8.55745189714029E-15,1.));
#40362=DIRECTION('center_axis',(-2.77102527463854E-15,-8.5557679050281E-15,
-1.));
#40363=DIRECTION('ref_axis',(6.7618653731838E-14,-1.,8.55576790502791E-15));
#40364=DIRECTION('center_axis',(-2.77102527463854E-15,-8.5557679050281E-15,
-1.));
#40365=DIRECTION('ref_axis',(-1.,-6.35644329412406E-14,2.77102527463908E-15));
#40366=DIRECTION('center_axis',(-2.77102527463854E-15,-8.5557679050281E-15,
-1.));
#40367=DIRECTION('ref_axis',(-1.,-7.07975313971927E-14,2.77102527463915E-15));
#40368=DIRECTION('center_axis',(2.77102527463857E-15,8.11729798613651E-15,
1.));
#40369=DIRECTION('ref_axis',(-1.,-6.7618653731838E-14,2.77102527463912E-15));
#40370=DIRECTION('',(2.77102527463857E-15,8.11729798613651E-15,1.));
#40371=DIRECTION('center_axis',(2.77102527463854E-15,8.5557679050281E-15,
1.));
#40372=DIRECTION('ref_axis',(-1.,-6.7618653731838E-14,2.77102527463912E-15));
#40373=DIRECTION('',(2.77102527463854E-15,8.5557679050281E-15,1.));
#40374=DIRECTION('center_axis',(-2.77102527463833E-15,-1.17346455703829E-14,
-1.));
#40375=DIRECTION('ref_axis',(-1.,-7.07975313971927E-14,2.77102527463916E-15));
#40376=DIRECTION('center_axis',(-2.77102527463854E-15,-8.5557679050281E-15,
-1.));
#40377=DIRECTION('ref_axis',(6.7618653731838E-14,-1.,8.55576790502791E-15));
#40378=DIRECTION('center_axis',(-2.77102527463854E-15,-8.5557679050281E-15,
-1.));
#40379=DIRECTION('ref_axis',(1.,6.66050985341886E-14,-2.77102527463911E-15));
#40380=DIRECTION('center_axis',(2.77102527463854E-15,8.5557679050281E-15,
1.));
#40381=DIRECTION('ref_axis',(1.,7.16728745224354E-14,-2.77102527463915E-15));
#40382=DIRECTION('',(-2.77102527463854E-15,-8.5557679050281E-15,-1.));
#40383=DIRECTION('center_axis',(-2.77102527463854E-15,-8.5557679050281E-15,
-1.));
#40384=DIRECTION('ref_axis',(6.7618653731838E-14,-1.,8.55576790502791E-15));
#40385=DIRECTION('center_axis',(2.77102527463854E-15,8.5557679050281E-15,
1.));
#40386=DIRECTION('ref_axis',(1.,6.7618653731838E-14,-2.77102527463912E-15));
#40387=DIRECTION('center_axis',(-2.77102527463854E-15,-8.5557679050281E-15,
-1.));
#40388=DIRECTION('ref_axis',(1.,6.7618653731838E-14,-2.77102527463912E-15));
#40389=DIRECTION('center_axis',(2.77102527463833E-15,1.17346455703829E-14,
1.));
#40390=DIRECTION('ref_axis',(1.,6.7618653731838E-14,-2.77102527463912E-15));
#40391=DIRECTION('',(-2.77102527463854E-15,-8.5557679050281E-15,-1.));
#40392=DIRECTION('center_axis',(-2.77102527463854E-15,-8.5557679050281E-15,
-1.));
#40393=DIRECTION('ref_axis',(6.7618653731838E-14,-1.,8.55576790502791E-15));
#40394=DIRECTION('center_axis',(-2.77102527463854E-15,-8.5557679050281E-15,
-1.));
#40395=DIRECTION('ref_axis',(6.7618653731838E-14,-1.,8.55576790502791E-15));
#40396=DIRECTION('center_axis',(-2.77102527463833E-15,-1.17346455703829E-14,
-1.));
#40397=DIRECTION('ref_axis',(-1.,-6.90135324843597E-14,2.77102527463914E-15));
#40398=DIRECTION('center_axis',(2.77102527463854E-15,8.56804061665863E-15,
1.));
#40399=DIRECTION('ref_axis',(-1.,-6.64947506794674E-14,2.77102527463911E-15));
#40400=DIRECTION('center_axis',(-2.77102527463854E-15,-8.5557679050281E-15,
-1.));
#40401=DIRECTION('ref_axis',(-1.,-6.94133515893739E-14,2.77102527463913E-15));
#40402=DIRECTION('',(2.77102527463854E-15,8.56804061665863E-15,1.));
#40403=DIRECTION('center_axis',(-2.77102527463854E-15,-8.5557679050281E-15,
-1.));
#40404=DIRECTION('ref_axis',(6.7618653731838E-14,-1.,8.55576790502791E-15));
#40405=DIRECTION('center_axis',(-2.77102527463854E-15,-8.5557679050281E-15,
-1.));
#40406=DIRECTION('ref_axis',(-1.,-6.80361569771588E-14,2.77102527463912E-15));
#40407=DIRECTION('center_axis',(2.77102527463854E-15,8.56804073271148E-15,
1.));
#40408=DIRECTION('ref_axis',(-1.,-6.7618653731838E-14,2.77102527463912E-15));
#40409=DIRECTION('',(2.77102527463854E-15,8.56804073271148E-15,1.));
#40410=DIRECTION('center_axis',(-2.77102527463854E-15,-8.56804074636475E-15,
-1.));
#40411=DIRECTION('ref_axis',(1.,6.8335345472937E-14,-2.77102527463912E-15));
#40412=DIRECTION('center_axis',(2.77102527463854E-15,8.5557679050281E-15,
1.));
#40413=DIRECTION('ref_axis',(1.,6.66124823430948E-14,-2.77102527463911E-15));
#40414=DIRECTION('',(-2.77102527463854E-15,-8.56804074636475E-15,-1.));
#40415=DIRECTION('center_axis',(-2.77102527463854E-15,-8.5557679050281E-15,
-1.));
#40416=DIRECTION('ref_axis',(6.7618653731838E-14,-1.,8.55576790502791E-15));
#40417=DIRECTION('center_axis',(2.77102527463854E-15,8.5557679050281E-15,
1.));
#40418=DIRECTION('ref_axis',(1.,6.85355210440792E-14,-2.77102527463913E-15));
#40419=DIRECTION('center_axis',(-2.77102527463854E-15,-8.56804073953811E-15,
-1.));
#40420=DIRECTION('ref_axis',(1.,6.53708478165727E-14,-2.7710252746391E-15));
#40421=DIRECTION('center_axis',(2.77102527463833E-15,1.17346455703829E-14,
1.));
#40422=DIRECTION('ref_axis',(1.,6.89353399596176E-14,-2.77102527463913E-15));
#40423=DIRECTION('',(-2.77102527463854E-15,-8.56804073953811E-15,-1.));
#40424=DIRECTION('center_axis',(-2.77102527463854E-15,-8.5557679050281E-15,
-1.));
#40425=DIRECTION('ref_axis',(6.7618653731838E-14,-1.,8.55576790502791E-15));
#40426=DIRECTION('center_axis',(6.7618653731838E-14,-1.,8.55576790502791E-15));
#40427=DIRECTION('ref_axis',(2.77102527463854E-15,8.5557679050281E-15,1.));
#40428=DIRECTION('',(9.05427566006634E-15,8.55576790502852E-15,1.));
#40429=DIRECTION('',(1.,6.7618653731838E-14,-2.77102527463912E-15));
#40430=DIRECTION('',(-2.77102527463854E-15,-8.5557679050281E-15,-1.));
#40431=DIRECTION('',(2.77102527463854E-15,8.5557679050281E-15,1.));
#40432=DIRECTION('',(1.,6.7618653731838E-14,-2.77102527463912E-15));
#40433=DIRECTION('center_axis',(-3.71186709412393E-15,-8.55576790502816E-15,
-1.));
#40434=DIRECTION('ref_axis',(6.7618653731838E-14,-1.,8.55576790502791E-15));
#40435=DIRECTION('',(9.05427566006634E-15,8.55576790502852E-15,1.));
#40436=DIRECTION('center_axis',(3.64505808662706E-15,-8.55576790502766E-15,
-1.));
#40437=DIRECTION('ref_axis',(-8.68669038156344E-14,1.,-8.55576790502798E-15));
#40438=DIRECTION('center_axis',(-5.97906695527122E-15,-8.55576790502831E-15,
-1.));
#40439=DIRECTION('ref_axis',(-4.99744244883579E-14,1.,-8.55576790502801E-15));
#40440=DIRECTION('center_axis',(-6.7618653731838E-14,1.,-8.55576790502791E-15));
#40441=DIRECTION('ref_axis',(-2.77102527463854E-15,-8.5557679050281E-15,
-1.));
#40442=DIRECTION('',(2.77102527463854E-15,8.5557679050281E-15,1.));
#40443=DIRECTION('',(-1.,-6.7618653731838E-14,2.77102527463912E-15));
#40444=DIRECTION('',(-1.,-6.7618653731838E-14,2.77102527463912E-15));
#40445=DIRECTION('',(2.77102527463854E-15,8.5557679050281E-15,1.));
#40446=DIRECTION('center_axis',(-2.77102527463854E-15,-8.5557679050281E-15,
-1.));
#40447=DIRECTION('ref_axis',(6.7618653731838E-14,-1.,8.55576790502791E-15));
#40448=DIRECTION('center_axis',(-5.97906695527179E-15,-8.55576790502831E-15,
-1.));
#40449=DIRECTION('ref_axis',(-6.44106120512047E-14,1.,-8.55576790502793E-15));
#40450=DIRECTION('center_axis',(-2.77102527463854E-15,-8.5557679050281E-15,
-1.));
#40451=DIRECTION('ref_axis',(6.92226745721546E-14,-1.,8.5557679050279E-15));
#40452=DIRECTION('center_axis',(2.77102527463854E-15,8.5557679050281E-15,
1.));
#40453=DIRECTION('ref_axis',(-1.,-4.55530009807148E-14,2.77102527463893E-15));
#40454=DIRECTION('center_axis',(-2.63111778409163E-15,-9.17043370360255E-15,
-1.));
#40455=DIRECTION('ref_axis',(-6.7618653731838E-14,1.,-9.17043370360237E-15));
#40456=DIRECTION('center_axis',(-2.77102527463854E-15,-8.5557679050281E-15,
-1.));
#40457=DIRECTION('ref_axis',(6.92226745721546E-14,-1.,8.5557679050279E-15));
#40458=DIRECTION('center_axis',(-2.80745897018724E-15,-8.5557679050281E-15,
-1.));
#40459=DIRECTION('ref_axis',(6.7618653731838E-14,-1.,8.55576790502791E-15));
#40460=DIRECTION('center_axis',(-2.80745897018724E-15,-8.5557679050281E-15,
-1.));
#40461=DIRECTION('ref_axis',(-2.43100910432985E-14,1.,-8.55576790502803E-15));
#40462=DIRECTION('center_axis',(4.3701640599445E-16,-8.55576790502817E-15,
-1.));
#40463=DIRECTION('ref_axis',(5.63905078496234E-14,-1.,8.55576790502819E-15));
#40464=DIRECTION('center_axis',(-2.77102527463854E-15,-8.5557679050281E-15,
-1.));
#40465=DIRECTION('ref_axis',(6.7618653731838E-14,-1.,8.55576790502791E-15));
#40466=DIRECTION('center_axis',(2.77102527463854E-15,8.5557679050281E-15,
1.));
#40467=DIRECTION('ref_axis',(-1.,-6.92565555623126E-14,2.77102527463913E-15));
#40468=DIRECTION('center_axis',(2.75460319106607E-15,8.53296808841364E-15,
1.));
#40469=DIRECTION('ref_axis',(0.811429434660075,-0.58445040214481,2.7519305207226E-15));
#40470=DIRECTION('center_axis',(-7.66431182155099E-14,1.52787649784829E-14,
-1.));
#40471=DIRECTION('ref_axis',(0.811429434660079,-0.584450402144805,-7.11201624201471E-14));
#40472=DIRECTION('center_axis',(1.71148062915242E-14,-8.55576790502675E-15,
-1.));
#40473=DIRECTION('ref_axis',(0.811429434660073,-0.584450402144813,1.88878795861987E-14));
#40474=DIRECTION('center_axis',(2.77102527463854E-15,8.56804068897833E-15,
1.));
#40475=DIRECTION('ref_axis',(-1.,-6.7618653731838E-14,2.77102527463912E-15));
#40476=DIRECTION('',(-2.77102527463854E-15,-8.56804068897833E-15,-1.));
#40477=DIRECTION('center_axis',(-2.77102527463799E-15,-1.6687780537331E-14,
-1.));
#40478=DIRECTION('ref_axis',(-1.,-6.52077354570261E-14,2.77102527463908E-15));
#40479=DIRECTION('center_axis',(2.77102527463854E-15,8.5557679050281E-15,
1.));
#40480=DIRECTION('ref_axis',(-6.7618653731838E-14,1.,-8.55576790502791E-15));
#40481=DIRECTION('center_axis',(-6.99630283644434E-14,1.,0.));
#40482=DIRECTION('ref_axis',(0.,-9.99471833777773E-15,-1.));
#40483=DIRECTION('center_axis',(-1.,-6.7618653731838E-14,2.77102527463912E-15));
#40484=DIRECTION('ref_axis',(7.02309329852463E-15,-0.144413862398959,-0.989517375464936));
#40485=DIRECTION('center_axis',(7.15738251412779E-14,-1.,4.29833232732464E-15));
#40486=DIRECTION('ref_axis',(0.504155551068649,3.23722461609332E-14,-0.863612864845509));
#40487=DIRECTION('center_axis',(-0.707106781186504,-0.707106781186591,-2.23509189115751E-13));
#40488=DIRECTION('ref_axis',(0.067224975942765,-0.0672249759424421,-0.995470544626526));
#40489=DIRECTION('center_axis',(-1.,-6.7618653731838E-14,2.77102527463912E-15));
#40490=DIRECTION('ref_axis',(-2.00277979389365E-14,0.256579164383079,-0.966523218761185));
#40491=DIRECTION('center_axis',(6.7618653731838E-14,-1.,8.55576790502791E-15));
#40492=DIRECTION('ref_axis',(0.144413862399064,1.29898995316941E-15,-0.98951737546492));
#40493=DIRECTION('center_axis',(1.,6.7618653731838E-14,-2.77102527463912E-15));
#40494=DIRECTION('ref_axis',(-3.64834127106881E-14,0.504155551068691,-0.863612864845484));
#40495=DIRECTION('center_axis',(0.707106781186603,-0.707106781186492,-9.33092817933997E-15));
#40496=DIRECTION('ref_axis',(0.0672249759425836,0.0672249759426073,-0.995470544626527));
#40497=DIRECTION('center_axis',(6.86644901853775E-14,-1.,1.10717869485878E-14));
#40498=DIRECTION('ref_axis',(-0.256579164383157,-2.83190166735466E-14,-0.966523218761164));
#40499=DIRECTION('center_axis',(1.,6.76186537318372E-14,-8.87945683687985E-14));
#40500=DIRECTION('ref_axis',(-9.76288392034752E-14,0.144413862399098,-0.989517375464915));
#40501=DIRECTION('center_axis',(1.,1.01085420245098E-13,7.77415841192694E-14));
#40502=DIRECTION('ref_axis',(1.01075458772354E-13,-0.256579164383133,-0.96652321876117));
#40503=DIRECTION('center_axis',(-6.7618653731838E-14,1.,-8.55576790502791E-15));
#40504=DIRECTION('ref_axis',(-0.14441386239907,-1.82311519581102E-14,-0.989517375464919));
#40505=DIRECTION('center_axis',(-1.,-6.7618653731838E-14,2.77102527463912E-15));
#40506=DIRECTION('ref_axis',(3.16972265587057E-14,-0.504155551068665,-0.863612864845499));
#40507=DIRECTION('center_axis',(-0.7071067811866,0.707106781186495,-2.2386518306794E-13));
#40508=DIRECTION('ref_axis',(-0.0672249759424351,-0.0672249759427602,-0.995470544626527));
#40509=DIRECTION('center_axis',(-6.7618653731838E-14,1.,-8.55576790502791E-15));
#40510=DIRECTION('ref_axis',(0.256579164383152,9.08018933668768E-15,-0.966523218761165));
#40511=DIRECTION('center_axis',(2.77102527463854E-15,8.5557679050281E-15,
1.));
#40512=DIRECTION('ref_axis',(-6.7618653731838E-14,1.,-8.55576790502791E-15));
#40513=DIRECTION('center_axis',(1.71148062915315E-14,-8.55576790502675E-15,
-1.));
#40514=DIRECTION('ref_axis',(-0.811429434660146,0.584450402144712,-1.8887879586205E-14));
#40515=DIRECTION('center_axis',(-2.77102527463799E-15,-1.6687780537331E-14,
-1.));
#40516=DIRECTION('ref_axis',(-1.,-6.84069885735319E-14,2.77102527463913E-15));
#40517=DIRECTION('center_axis',(2.77102527463863E-15,7.29513229243521E-15,
1.));
#40518=DIRECTION('ref_axis',(-1.,-6.90562041476608E-14,2.77102527463913E-15));
#40519=DIRECTION('',(-2.77102527463863E-15,-7.29513229243521E-15,-1.));
#40520=DIRECTION('center_axis',(2.75459778662046E-15,8.53296058508019E-15,
1.));
#40521=DIRECTION('ref_axis',(-0.811429434660145,0.584450402144713,-2.75193052072158E-15));
#40522=DIRECTION('center_axis',(-1.27139410577239E-14,-5.34772622439547E-15,
-1.));
#40523=DIRECTION('ref_axis',(-0.81142943466015,0.584450402144707,7.19098526236367E-15));
#40524=DIRECTION('center_axis',(-6.99630283644434E-14,1.,0.));
#40525=DIRECTION('ref_axis',(0.,-9.99471833777773E-15,-1.));
#40526=DIRECTION('center_axis',(-1.,-4.27399845701664E-14,3.45511976547096E-13));
#40527=DIRECTION('ref_axis',(-3.35717857973925E-13,-0.144413862399068,-0.98951737546492));
#40528=DIRECTION('center_axis',(6.77586799616196E-14,-1.,1.15647158182159E-14));
#40529=DIRECTION('ref_axis',(0.504155551068638,2.41734772768401E-14,-0.863612864845515));
#40530=DIRECTION('center_axis',(-0.707106781186505,-0.70710678118659,-2.46996567226803E-13));
#40531=DIRECTION('ref_axis',(0.0672249759428265,-0.0672249759424707,-0.99547054462652));
#40532=DIRECTION('center_axis',(-1.,-3.41518872186049E-14,-7.77415841192225E-14));
#40533=DIRECTION('ref_axis',(6.63763834298554E-14,0.256579164382971,-0.966523218761213));
#40534=DIRECTION('center_axis',(6.7618653731838E-14,-1.,8.55576790502791E-15));
#40535=DIRECTION('ref_axis',(0.144413862399062,1.29898995316927E-15,-0.989517375464921));
#40536=DIRECTION('center_axis',(1.,1.01085420245101E-13,-8.32836346685738E-14));
#40537=DIRECTION('ref_axis',(-1.22887594079545E-13,0.504155551068567,-0.863612864845557));
#40538=DIRECTION('center_axis',(0.707106781186596,-0.707106781186499,6.38249639743397E-13));
#40539=DIRECTION('ref_axis',(0.0672249759431773,0.0672249759422879,-0.995470544626509));
#40540=DIRECTION('center_axis',(6.58951814592576E-14,-1.,6.32142250125411E-15));
#40541=DIRECTION('ref_axis',(-0.256579164383186,-2.3017132218756E-14,-0.966523218761156));
#40542=DIRECTION('center_axis',(1.,6.7618653731838E-14,-2.77102527463912E-15));
#40543=DIRECTION('ref_axis',(-1.25070486127466E-14,0.144413862399052,-0.989517375464922));
#40544=DIRECTION('center_axis',(-6.7618653731838E-14,1.,-8.55576790502791E-15));
#40545=DIRECTION('ref_axis',(-0.504155551068567,-4.14791908661042E-14,-0.863612864845557));
#40546=DIRECTION('center_axis',(0.707106781186503,0.707106781186592,7.20099469180332E-13));
#40547=DIRECTION('ref_axis',(-0.0672249759422375,0.0672249759432429,-0.995470544626508));
#40548=DIRECTION('center_axis',(1.,3.41518872185722E-14,-8.32836346685755E-14));
#40549=DIRECTION('ref_axis',(-7.17329039653535E-14,-0.256579164383119,-0.966523218761174));
#40550=DIRECTION('center_axis',(-6.7618653731838E-14,1.,2.19717498174569E-15));
#40551=DIRECTION('ref_axis',(-0.144413862399068,-7.59092813426568E-15,-0.98951737546492));
#40552=DIRECTION('center_axis',(-1.,-1.01085420245114E-13,-7.77415841193218E-14));
#40553=DIRECTION('ref_axis',(1.18101407927591E-13,-0.504155551068541,-0.863612864845571));
#40554=DIRECTION('center_axis',(-0.707106781186599,0.707106781186496,-9.97176130514017E-14));
#40555=DIRECTION('ref_axis',(-0.0672249759425231,-0.0672249759426732,-0.995470544626527));
#40556=DIRECTION('center_axis',(-6.65728172782997E-14,1.,-1.10717869485855E-14));
#40557=DIRECTION('ref_axis',(0.256579164382955,6.38005866889998E-15,-0.966523218761218));
#40558=DIRECTION('center_axis',(-6.69476735228678E-14,1.,-8.81842604587865E-15));
#40559=DIRECTION('ref_axis',(-2.77102527463852E-15,-8.81842604587884E-15,
-1.));
#40560=DIRECTION('',(-2.77102527463854E-15,-8.5557679050281E-15,-1.));
#40561=DIRECTION('',(-1.,-6.69232742425416E-14,2.77102527463911E-15));
#40562=DIRECTION('',(-2.77102527463854E-15,-8.5557679050281E-15,-1.));
#40563=DIRECTION('center_axis',(1.,6.7618653731838E-14,-2.77102527463912E-15));
#40564=DIRECTION('ref_axis',(6.7618653731838E-14,-1.,8.55576790502791E-15));
#40565=DIRECTION('',(-2.77102527463854E-15,-8.5557679050281E-15,-1.));
#40566=DIRECTION('',(-6.7618653731838E-14,1.,-8.55576790502791E-15));
#40567=DIRECTION('center_axis',(6.68518192073007E-14,-1.,8.85594863742873E-15));
#40568=DIRECTION('ref_axis',(2.77102527463852E-15,8.85594863742892E-15,
1.));
#40569=DIRECTION('',(-2.7710252746385E-15,-9.17308743531861E-15,-1.));
#40570=DIRECTION('',(1.,6.68239343154993E-14,-2.77102527463911E-15));
#40571=DIRECTION('center_axis',(0.707106781186592,-0.707106781186503,4.09043074136686E-15));
#40572=DIRECTION('ref_axis',(2.77102527463854E-15,8.5557679050281E-15,1.));
#40573=DIRECTION('',(-2.77102527463854E-15,-8.5557679050281E-15,-1.));
#40574=DIRECTION('',(0.707106781186499,0.707106781186596,-8.00925226644009E-15));
#40575=DIRECTION('center_axis',(1.,6.7618653731838E-14,-2.77102527463912E-15));
#40576=DIRECTION('ref_axis',(6.7618653731838E-14,-1.,8.55576790502791E-15));
#40577=DIRECTION('',(-2.77102527463854E-15,-8.5557679050281E-15,-1.));
#40578=DIRECTION('',(-6.7618653731838E-14,1.,-8.55576790502791E-15));
#40579=DIRECTION('center_axis',(6.7618653731838E-14,-1.,8.55576790502791E-15));
#40580=DIRECTION('ref_axis',(2.77102527463854E-15,8.5557679050281E-15,1.));
#40581=DIRECTION('',(-2.77102527463854E-15,-8.5557679050281E-15,-1.));
#40582=DIRECTION('',(1.,6.7618653731838E-14,-2.77102527463912E-15));
#40583=DIRECTION('center_axis',(-1.,-6.7618653731838E-14,2.77102527463912E-15));
#40584=DIRECTION('ref_axis',(-6.7618653731838E-14,1.,-8.55576790502791E-15));
#40585=DIRECTION('',(-2.77102527463854E-15,-8.5557679050281E-15,-1.));
#40586=DIRECTION('',(6.7618653731838E-14,-1.,8.55576790502791E-15));
#40587=DIRECTION('center_axis',(-0.7071067811865,-0.707106781186595,8.19011459861795E-15));
#40588=DIRECTION('ref_axis',(2.76568749322768E-15,8.8168836495273E-15,1.));
#40589=DIRECTION('',(-2.77102527463854E-15,-8.5557679050281E-15,-1.));
#40590=DIRECTION('',(0.707106781186594,-0.707106781186501,4.09043074136684E-15));
#40591=DIRECTION('center_axis',(6.96315943587485E-14,-1.,8.5557679050279E-15));
#40592=DIRECTION('ref_axis',(2.77102527463854E-15,8.5557679050281E-15,1.));
#40593=DIRECTION('',(-2.77102527463849E-15,-9.3534957749956E-15,-1.));
#40594=DIRECTION('',(1.,6.97047921997271E-14,-2.77102527463914E-15));
#40595=DIRECTION('center_axis',(-1.,-6.7618653731838E-14,2.77102527463912E-15));
#40596=DIRECTION('ref_axis',(-6.7618653731838E-14,1.,-8.55576790502791E-15));
#40597=DIRECTION('',(-2.77102527463854E-15,-8.5557679050281E-15,-1.));
#40598=DIRECTION('',(6.7618653731838E-14,-1.,8.55576790502791E-15));
#40599=DIRECTION('center_axis',(-6.7618653731838E-14,1.,-8.55576790502791E-15));
#40600=DIRECTION('ref_axis',(-2.77102527463854E-15,-8.5557679050281E-15,
-1.));
#40601=DIRECTION('',(-2.77102527463854E-15,-8.5557679050281E-15,-1.));
#40602=DIRECTION('',(-1.,-6.7618653731838E-14,2.77102527463912E-15));
#40603=DIRECTION('center_axis',(-0.707106781186592,0.707106781186503,-4.09043074136686E-15));
#40604=DIRECTION('ref_axis',(-2.77102527463854E-15,-8.5557679050281E-15,
-1.));
#40605=DIRECTION('',(-2.77102527463854E-15,-8.5557679050281E-15,-1.));
#40606=DIRECTION('',(-0.707106781186497,-0.707106781186598,8.00925226644011E-15));
#40607=DIRECTION('center_axis',(-1.,-6.7618653731838E-14,2.77102527463912E-15));
#40608=DIRECTION('ref_axis',(-6.7618653731838E-14,1.,-8.55576790502791E-15));
#40609=DIRECTION('',(-2.77102527463854E-15,-8.5557679050281E-15,-1.));
#40610=DIRECTION('',(6.7618653731838E-14,-1.,8.55576790502791E-15));
#40611=DIRECTION('center_axis',(-6.7618653731838E-14,1.,-8.55576790502791E-15));
#40612=DIRECTION('ref_axis',(-2.77102527463854E-15,-8.5557679050281E-15,
-1.));
#40613=DIRECTION('',(-2.77102527463854E-15,-8.5557679050281E-15,-1.));
#40614=DIRECTION('',(-1.,-6.7618653731838E-14,2.77102527463912E-15));
#40615=DIRECTION('center_axis',(1.,6.7618653731838E-14,-2.77102527463912E-15));
#40616=DIRECTION('ref_axis',(6.7618653731838E-14,-1.,8.55576790502791E-15));
#40617=DIRECTION('',(-2.77102527463854E-15,-8.5557679050281E-15,-1.));
#40618=DIRECTION('',(-6.7618653731838E-14,1.,-8.55576790502791E-15));
#40619=DIRECTION('center_axis',(0.707106781186493,0.707106781186602,-8.00925226644013E-15));
#40620=DIRECTION('ref_axis',(-2.77102527463854E-15,-8.5557679050281E-15,
-1.));
#40621=DIRECTION('',(-0.707106781186595,0.7071067811865,-4.09043074136683E-15));
#40622=DIRECTION('center_axis',(-2.77102527463854E-15,-8.5557679050281E-15,
-1.));
#40623=DIRECTION('ref_axis',(6.7618653731838E-14,-1.,8.55576790502791E-15));
#40624=DIRECTION('center_axis',(1.,6.7618653731838E-14,-2.77102527463912E-15));
#40625=DIRECTION('ref_axis',(6.7618653731838E-14,-1.,8.55576790502791E-15));
#40626=DIRECTION('',(-2.77102527463854E-15,-8.5557679050281E-15,-1.));
#40627=DIRECTION('center_axis',(6.7618653731838E-14,-1.,8.81842604587865E-15));
#40628=DIRECTION('ref_axis',(2.77102527463852E-15,8.81842604587884E-15,
1.));
#40629=DIRECTION('',(-2.77102527463854E-15,-8.5557679050281E-15,-1.));
#40630=DIRECTION('center_axis',(0.707106781186593,-0.707106781186502,4.29713054957012E-15));
#40631=DIRECTION('ref_axis',(2.7691954317893E-15,8.84625573427986E-15,1.));
#40632=DIRECTION('',(-2.77102527463854E-15,-8.5557679050281E-15,-1.));
#40633=DIRECTION('center_axis',(1.,6.7618653731838E-14,-2.77102527463912E-15));
#40634=DIRECTION('ref_axis',(6.7618653731838E-14,-1.,8.55576790502791E-15));
#40635=DIRECTION('',(-2.77102527463854E-15,-8.5557679050281E-15,-1.));
#40636=DIRECTION('center_axis',(6.7618653731838E-14,-1.,8.55576790502791E-15));
#40637=DIRECTION('ref_axis',(2.77102527463854E-15,8.5557679050281E-15,1.));
#40638=DIRECTION('',(-2.77102527463854E-15,-8.5557679050281E-15,-1.));
#40639=DIRECTION('center_axis',(-1.,-6.7618653731838E-14,2.77102527463912E-15));
#40640=DIRECTION('ref_axis',(-6.7618653731838E-14,1.,-8.55576790502791E-15));
#40641=DIRECTION('',(-2.77102527463854E-15,-8.5557679050281E-15,-1.));
#40642=DIRECTION('center_axis',(-0.707106781186495,-0.7071067811866,8.00925226644012E-15));
#40643=DIRECTION('ref_axis',(2.77102527463854E-15,8.5557679050281E-15,1.));
#40644=DIRECTION('',(-2.77102527463854E-15,-8.5557679050281E-15,-1.));
#40645=DIRECTION('center_axis',(6.89606141497783E-14,-1.,8.55576790502791E-15));
#40646=DIRECTION('ref_axis',(2.77102527463854E-15,8.5557679050281E-15,1.));
#40647=DIRECTION('',(-2.77102527463854E-15,-8.5557679050281E-15,-1.));
#40648=DIRECTION('center_axis',(-1.,-6.7618653731838E-14,2.77102527463912E-15));
#40649=DIRECTION('ref_axis',(-6.7618653731838E-14,1.,-8.55576790502791E-15));
#40650=DIRECTION('',(-2.77102527463854E-15,-8.5557679050281E-15,-1.));
#40651=DIRECTION('center_axis',(-6.7618653731838E-14,1.,-8.81842604587865E-15));
#40652=DIRECTION('ref_axis',(-2.77102527463852E-15,-8.81842604587884E-15,
-1.));
#40653=DIRECTION('',(-2.7710252746385E-15,-9.0959224940323E-15,-1.));
#40654=DIRECTION('center_axis',(-0.70710678118659,0.707106781186505,-4.09043074136688E-15));
#40655=DIRECTION('ref_axis',(-2.77102527463854E-15,-8.5557679050281E-15,
-1.));
#40656=DIRECTION('',(-2.77102527463854E-15,-8.5557679050281E-15,-1.));
#40657=DIRECTION('center_axis',(-1.,-6.7618653731838E-14,2.77102527463912E-15));
#40658=DIRECTION('ref_axis',(-6.7618653731838E-14,1.,-8.55576790502791E-15));
#40659=DIRECTION('',(-2.77102527463854E-15,-8.5557679050281E-15,-1.));
#40660=DIRECTION('center_axis',(-6.7618653731838E-14,1.,-8.55576790502791E-15));
#40661=DIRECTION('ref_axis',(-2.77102527463854E-15,-8.5557679050281E-15,
-1.));
#40662=DIRECTION('',(-2.77102527463854E-15,-8.5557679050281E-15,-1.));
#40663=DIRECTION('center_axis',(1.,6.7618653731838E-14,-2.77102527463912E-15));
#40664=DIRECTION('ref_axis',(6.7618653731838E-14,-1.,8.55576790502791E-15));
#40665=DIRECTION('axis',(0.,0.,1.));
#40666=DIRECTION('refdir',(1.,0.,0.));
#40667=DIRECTION('center_axis',(1.,-5.00596043936353E-16,-3.34404360992166E-15));
#40668=DIRECTION('ref_axis',(-2.71857077046111E-15,-0.707106781186757,-0.707106781186338));
#40669=DIRECTION('center_axis',(-1.,5.00596043936353E-16,3.34404360992166E-15));
#40670=DIRECTION('ref_axis',(-2.71857077046111E-15,-0.707106781186757,-0.707106781186338));
#40671=DIRECTION('',(1.,-5.00596043936353E-16,-3.34404360992166E-15));
#40672=DIRECTION('center_axis',(1.,-5.00596043936353E-16,-3.34404360992166E-15));
#40673=DIRECTION('ref_axis',(-2.71857077046111E-15,-0.707106781186757,-0.707106781186338));
#40674=DIRECTION('',(-1.,5.00596043936353E-16,3.34404360992166E-15));
#40675=DIRECTION('center_axis',(-3.34404360992166E-15,5.94374044734026E-16,
-1.));
#40676=DIRECTION('ref_axis',(5.00596043936355E-16,1.,5.94374044734051E-16));
#40677=DIRECTION('',(5.00596043936355E-16,1.,5.94374044734026E-16));
#40678=DIRECTION('',(-1.,5.00596043936353E-16,3.34404360992166E-15));
#40679=DIRECTION('',(-5.00596043936355E-16,-1.,-5.94374044734026E-16));
#40680=DIRECTION('',(1.,-5.00596043936353E-16,-3.34404360992166E-15));
#40681=DIRECTION('',(5.00596043936355E-16,1.,5.94374044734026E-16));
#40682=DIRECTION('',(-1.,5.00596043936353E-16,3.34404360992166E-15));
#40683=DIRECTION('',(-5.00596043936355E-16,-1.,-5.94374044734026E-16));
#40684=DIRECTION('',(1.,-5.00596043936353E-16,-3.34404360992166E-15));
#40685=DIRECTION('',(5.00596043936355E-16,1.,5.94374044734026E-16));
#40686=DIRECTION('',(-1.,5.00596043936353E-16,3.34404360992166E-15));
#40687=DIRECTION('',(-5.00596043936355E-16,-1.,-5.94374044734026E-16));
#40688=DIRECTION('center_axis',(-3.34404360992166E-15,5.94374044734026E-16,
-1.));
#40689=DIRECTION('ref_axis',(-5.00596043936355E-16,-1.,-5.94374044734082E-16));
#40690=DIRECTION('center_axis',(-3.34404360992166E-15,5.94374044734026E-16,
-1.));
#40691=DIRECTION('ref_axis',(-5.00596043936355E-16,-1.,-5.94374044734082E-16));
#40692=DIRECTION('',(-1.,5.00596043936353E-16,3.34404360992166E-15));
#40693=DIRECTION('',(-5.00596043936355E-16,-1.,-5.94374044734026E-16));
#40694=DIRECTION('',(1.,-5.00596043936353E-16,-3.34404360992166E-15));
#40695=DIRECTION('',(5.00596043936355E-16,1.,5.94374044734026E-16));
#40696=DIRECTION('center_axis',(-3.34404360992166E-15,5.94374044734026E-16,
-1.));
#40697=DIRECTION('ref_axis',(-5.00596043936355E-16,-1.,-5.94374044734082E-16));
#40698=DIRECTION('center_axis',(-3.34404360992166E-15,5.94374044734026E-16,
-1.));
#40699=DIRECTION('ref_axis',(-5.00596043936355E-16,-1.,-5.94374044734082E-16));
#40700=DIRECTION('center_axis',(-5.00596043936355E-16,-1.,-5.94374044734026E-16));
#40701=DIRECTION('ref_axis',(0.707106781186527,6.63110602902038E-17,-0.707106781186568));
#40702=DIRECTION('center_axis',(5.00596043936355E-16,1.,6.19091582356982E-16));
#40703=DIRECTION('ref_axis',(0.707106781186527,8.37889987576735E-17,-0.707106781186568));
#40704=DIRECTION('',(-5.00596043936355E-16,-1.,-5.94374044734026E-16));
#40705=DIRECTION('center_axis',(-5.00596043936355E-16,-1.,-5.94374044734026E-16));
#40706=DIRECTION('ref_axis',(0.707106781186527,6.63110602902038E-17,-0.707106781186568));
#40707=DIRECTION('center_axis',(1.,-5.00596043936353E-16,-3.34404360992166E-15));
#40708=DIRECTION('ref_axis',(-5.00596043934382E-16,-1.,5.89417440552492E-13));
#40709=DIRECTION('',(-3.34404360992166E-15,5.94374044734026E-16,-1.));
#40710=DIRECTION('',(-3.34404360992166E-15,6.19091582356982E-16,-1.));
#40711=DIRECTION('',(5.00596043931499E-16,1.,-1.45135967092772E-12));
#40712=DIRECTION('',(-3.34404360992166E-15,6.19091582356982E-16,-1.));
#40713=DIRECTION('',(1.01071973798223E-15,-0.899510317025162,0.436899518843055));
#40714=DIRECTION('',(-5.005960439315E-16,-1.,1.45135967092772E-12));
#40715=DIRECTION('',(-3.34404360992195E-15,-5.89417440552492E-13,-1.));
#40716=DIRECTION('',(5.00596043930822E-16,1.,-1.65391127897018E-12));
#40717=DIRECTION('center_axis',(1.,-5.00596043936353E-16,-3.34404360992166E-15));
#40718=DIRECTION('ref_axis',(-3.37116090328259E-15,-0.224153611366395,-0.974553825353635));
#40719=DIRECTION('',(-1.01071973799428E-15,0.899510317023531,-0.436899518846413));
#40720=DIRECTION('',(5.00596043934382E-16,1.,-5.89417440552492E-13));
#40721=DIRECTION('',(3.34404360992195E-15,5.89417440552492E-13,1.));
#40722=DIRECTION('',(5.00596043931499E-16,1.,-1.45135967092772E-12));
#40723=DIRECTION('center_axis',(1.,-5.00596043936353E-16,-3.34404360992166E-15));
#40724=DIRECTION('ref_axis',(3.37116090328329E-15,0.224153611363817,0.974553825354228));
#40725=DIRECTION('center_axis',(-1.,5.00596043936353E-16,3.34404360992166E-15));
#40726=DIRECTION('ref_axis',(3.37116090328329E-15,0.224153611363817,0.974553825354228));
#40727=DIRECTION('center_axis',(1.,-5.00596043936353E-16,-3.34404360992166E-15));
#40728=DIRECTION('ref_axis',(3.37116090328329E-15,0.224153611363817,0.974553825354228));
#40729=DIRECTION('center_axis',(-1.,-1.77856601184676E-14,1.22258278069232E-14));
#40730=DIRECTION('ref_axis',(1.22258278069229E-14,2.09832519444149E-14,
1.));
#40731=DIRECTION('',(1.,-5.00596043936353E-16,-3.34404360992166E-15));
#40732=DIRECTION('center_axis',(1.,-5.00596043936353E-16,-3.34404360992166E-15));
#40733=DIRECTION('ref_axis',(3.22671189843719E-15,0.436899518843004,0.899510317025186));
#40734=DIRECTION('center_axis',(1.50162002879617E-14,-0.436899518843088,
-0.899510317025146));
#40735=DIRECTION('ref_axis',(5.31748758588635E-11,0.899510317025146,-0.436899518843088));
#40736=DIRECTION('center_axis',(1.70009668144121E-14,-0.436899518843016,
-0.899510317025181));
#40737=DIRECTION('ref_axis',(-3.85139127936184E-11,0.89951031702518,-0.436899518843016));
#40738=DIRECTION('center_axis',(-1.,5.00596043936353E-16,3.34404360992166E-15));
#40739=DIRECTION('ref_axis',(5.00596043936355E-16,1.,6.88301496270999E-16));
#40740=DIRECTION('',(-3.34404360992166E-15,6.19091582356982E-16,-1.));
#40741=DIRECTION('',(-5.00596043931499E-16,-1.,1.45135967092772E-12));
#40742=DIRECTION('',(-3.34404360992166E-15,6.19091582356982E-16,-1.));
#40743=DIRECTION('center_axis',(5.00596043936355E-16,1.,6.19091582356982E-16));
#40744=DIRECTION('ref_axis',(1.,-5.00596043936353E-16,-3.34404360992166E-15));
#40745=DIRECTION('',(1.,-5.00596043936353E-16,-3.34404360992166E-15));
#40746=DIRECTION('center_axis',(-5.00596043936355E-16,-1.,-6.19091582356982E-16));
#40747=DIRECTION('ref_axis',(-4.15545247511164E-15,6.19091582356955E-16,
-1.));
#40748=DIRECTION('',(-1.,5.00596043936353E-16,3.34404360992166E-15));
#40749=DIRECTION('center_axis',(-3.22671189843713E-15,-0.436899518843055,
-0.899510317025162));
#40750=DIRECTION('ref_axis',(-1.01071973798224E-15,0.899510317025162,-0.436899518843055));
#40751=DIRECTION('',(1.,-5.00596043936353E-16,-3.34404360992166E-15));
#40752=DIRECTION('',(1.01071973798224E-15,-0.899510317025162,0.436899518843055));
#40753=DIRECTION('',(-1.,5.00596043936353E-16,3.34404360992166E-15));
#40754=DIRECTION('',(-1.01071973798223E-15,0.899510317025162,-0.436899518843055));
#40755=DIRECTION('center_axis',(-5.00596043936355E-16,-1.,-5.94374044734026E-16));
#40756=DIRECTION('ref_axis',(-0.707106781186548,7.74260774895239E-16,-0.707106781186547));
#40757=DIRECTION('center_axis',(5.00596043936355E-16,1.,6.19091582357991E-16));
#40758=DIRECTION('ref_axis',(-0.707106781186548,7.91738713363403E-16,-0.707106781186547));
#40759=DIRECTION('center_axis',(-5.00596043936355E-16,-1.,-5.94374044734026E-16));
#40760=DIRECTION('ref_axis',(-0.707106781186548,7.74260774895239E-16,-0.707106781186547));
#40761=DIRECTION('',(5.00596043936355E-16,1.,5.94374044734026E-16));
#40762=DIRECTION('center_axis',(0.0929057196031524,-0.979910694923634,0.176475372897471));
#40763=DIRECTION('ref_axis',(-0.456482036021868,-0.199436781899079,-0.867092336960182));
#40764=DIRECTION('center_axis',(-1.0107197379821E-15,0.89951031702518,-0.436899518843017));
#40765=DIRECTION('ref_axis',(-1.,5.00596043936353E-16,3.34404360992166E-15));
#40766=DIRECTION('center_axis',(-5.00596043931531E-16,-1.,1.44206872346462E-12));
#40767=DIRECTION('ref_axis',(-3.34404360992238E-15,-1.44206872346462E-12,
-1.));
#40768=DIRECTION('center_axis',(-1.,5.00596043936353E-16,3.34404360992166E-15));
#40769=DIRECTION('ref_axis',(-3.22671189843719E-15,-0.436899518843004,-0.899510317025186));
#40770=DIRECTION('center_axis',(-0.0929057196030986,-0.979910694923638,
0.176475372897477));
#40771=DIRECTION('ref_axis',(0.456482036021868,-0.199436781899079,-0.867092336960182));
#40772=DIRECTION('center_axis',(1.,-5.00596043936353E-16,-3.34404360992166E-15));
#40773=DIRECTION('ref_axis',(-3.34404360992238E-15,-1.44206872346462E-12,
-1.));
#40774=DIRECTION('center_axis',(-5.00596043931531E-16,-1.,1.44206872346462E-12));
#40775=DIRECTION('ref_axis',(1.,-5.00596043936353E-16,-3.34404360992166E-15));
#40776=DIRECTION('center_axis',(-1.01071973798204E-15,0.899510317025188,
-0.436899518843));
#40777=DIRECTION('ref_axis',(-3.22671189843719E-15,-0.436899518843,-0.899510317025188));
#40778=DIRECTION('center_axis',(-0.408248290464166,0.408248290464166,0.816496580927423));
#40779=DIRECTION('ref_axis',(-0.577350269189777,0.577350269188982,-0.577350269190118));
#40780=DIRECTION('center_axis',(5.00596043931531E-16,1.,-1.44206872346462E-12));
#40781=DIRECTION('ref_axis',(-1.,5.00596043936353E-16,3.34404360992166E-15));
#40782=DIRECTION('center_axis',(-3.34404360992196E-15,-5.89417440552492E-13,
-1.));
#40783=DIRECTION('ref_axis',(5.00596043934382E-16,1.,-5.89417440552492E-13));
#40784=DIRECTION('center_axis',(-1.,5.00596043936353E-16,3.34404360992166E-15));
#40785=DIRECTION('ref_axis',(-3.34404360992238E-15,-1.44206872346462E-12,
-1.));
#40786=DIRECTION('center_axis',(0.408248290463598,-0.816496580928219,-0.408248290463143));
#40787=DIRECTION('ref_axis',(0.577350269189777,0.577350269188982,-0.577350269190118));
#40788=DIRECTION('center_axis',(1.,-5.00596043936353E-16,-3.34404360992166E-15));
#40789=DIRECTION('ref_axis',(5.00596043934382E-16,1.,-5.89417440552492E-13));
#40790=DIRECTION('center_axis',(-3.34404360992196E-15,-5.89417440552492E-13,
-1.));
#40791=DIRECTION('ref_axis',(1.,-5.00596043936353E-16,-3.34404360992166E-15));
#40792=DIRECTION('center_axis',(5.00596043931531E-16,1.,-1.44206872346462E-12));
#40793=DIRECTION('ref_axis',(-3.34404360992238E-15,-1.44206872346462E-12,
-1.));
#40794=DIRECTION('center_axis',(0.816496580927953,0.408248290464147,0.408248290463124));
#40795=DIRECTION('ref_axis',(-0.577350269189285,0.577350269190592,0.577350269189001));
#40796=DIRECTION('center_axis',(3.34404360992196E-15,5.89417440552492E-13,
1.));
#40797=DIRECTION('ref_axis',(-1.,5.00596043936353E-16,3.34404360992166E-15));
#40798=DIRECTION('center_axis',(2.84717690347971E-13,1.,-1.72628581776865E-12));
#40799=DIRECTION('ref_axis',(3.34404360992252E-15,1.72628581776865E-12,
1.));
#40800=DIRECTION('center_axis',(-1.,5.00596043936353E-16,3.34404360992166E-15));
#40801=DIRECTION('ref_axis',(5.00596043934382E-16,1.,-5.89417440552492E-13));
#40802=DIRECTION('center_axis',(0.81649658092784,-0.408248290464147,-0.408248290463351));
#40803=DIRECTION('ref_axis',(0.577350269189436,0.577350269190346,0.577350269189095));
#40804=DIRECTION('center_axis',(1.,-5.00596043936353E-16,-3.34404360992166E-15));
#40805=DIRECTION('ref_axis',(3.34404360992252E-15,1.72628581776865E-12,
1.));
#40806=DIRECTION('center_axis',(5.00596043931531E-16,1.,-1.44206872346462E-12));
#40807=DIRECTION('ref_axis',(1.,-5.00596043936353E-16,-3.34404360992166E-15));
#40808=DIRECTION('center_axis',(3.34404360992196E-15,5.89417440552492E-13,
1.));
#40809=DIRECTION('ref_axis',(5.00596043934382E-16,1.,-5.89417440552492E-13));
#40810=DIRECTION('center_axis',(-1.,5.00596043936353E-16,3.34404360992166E-15));
#40811=DIRECTION('ref_axis',(0.,1.,-5.68434188608075E-13));
#40812=DIRECTION('center_axis',(-1.,5.00596043936353E-16,3.34404360992166E-15));
#40813=DIRECTION('ref_axis',(-3.3711609032826E-15,-0.224153611366396,-0.974553825353635));
#40814=DIRECTION('center_axis',(1.01071973799424E-15,-0.899510317023536,
0.436899518846402));
#40815=DIRECTION('ref_axis',(3.22671189843337E-15,0.436899518846402,0.899510317023536));
#40816=DIRECTION('center_axis',(1.,-5.00596043936353E-16,-3.34404360992166E-15));
#40817=DIRECTION('ref_axis',(-3.34404360992245E-15,-1.58417727061664E-12,
-1.));
#40818=DIRECTION('center_axis',(5.00596043931055E-16,1.,-1.58417727061664E-12));
#40819=DIRECTION('ref_axis',(-1.,5.00596043936353E-16,3.34404360992166E-15));
#40820=DIRECTION('center_axis',(-1.,5.00596043936353E-16,3.34404360992166E-15));
#40821=DIRECTION('ref_axis',(0.,1.,-5.6843418860808E-13));
#40822=DIRECTION('center_axis',(-1.,5.00596043936353E-16,3.34404360992166E-15));
#40823=DIRECTION('ref_axis',(-3.22671189843335E-15,-0.436899518846416,-0.899510317023529));
#40824=DIRECTION('center_axis',(1.01071973799427E-15,-0.899510317023533,
0.436899518846409));
#40825=DIRECTION('ref_axis',(1.,-5.00596043936353E-16,-3.34404360992166E-15));
#40826=DIRECTION('center_axis',(5.00596043931055E-16,1.,-1.58417727061664E-12));
#40827=DIRECTION('ref_axis',(3.34404360992245E-15,1.58417727061664E-12,
1.));
#40828=DIRECTION('center_axis',(-0.0929057196037775,-0.97991069492339,0.176475372898494));
#40829=DIRECTION('ref_axis',(-0.456482036022069,0.199436781900318,0.867092336959791));
#40830=DIRECTION('center_axis',(1.01071973799424E-15,-0.899510317023537,
0.4368995188464));
#40831=DIRECTION('ref_axis',(-1.,5.00596043936353E-16,3.34404360992166E-15));
#40832=DIRECTION('center_axis',(5.00596043934382E-16,1.,-5.89417440552492E-13));
#40833=DIRECTION('ref_axis',(3.34404360992196E-15,5.89417440552492E-13,
1.));
#40834=DIRECTION('center_axis',(-1.,5.00596043936353E-16,3.34404360992166E-15));
#40835=DIRECTION('ref_axis',(3.22671189843336E-15,0.436899518846405,0.899510317023535));
#40836=DIRECTION('center_axis',(0.816496580927783,-0.408248290463579,0.408248290464034));
#40837=DIRECTION('ref_axis',(-0.577350269189588,-0.577350269189304,0.577350269189986));
#40838=DIRECTION('center_axis',(-1.,5.00596043936353E-16,3.34404360992166E-15));
#40839=DIRECTION('ref_axis',(3.34404360992196E-15,5.89417440552492E-13,
1.));
#40840=DIRECTION('center_axis',(-5.00596043934382E-16,-1.,5.89417440552492E-13));
#40841=DIRECTION('ref_axis',(-1.,5.00596043936353E-16,3.34404360992166E-15));
#40842=DIRECTION('center_axis',(-1.09684848857867E-15,5.89417440552492E-13,
1.));
#40843=DIRECTION('ref_axis',(-5.00596043934382E-16,-1.,5.89417440552492E-13));
#40844=DIRECTION('center_axis',(5.00596043934382E-16,1.,-5.89417440552492E-13));
#40845=DIRECTION('ref_axis',(-0.707106781186544,4.17135044021589E-13,0.707106781186551));
#40846=DIRECTION('',(-5.00596043934382E-16,-1.,5.89417440552492E-13));
#40847=DIRECTION('',(5.00596043934382E-16,1.,-5.89417440552492E-13));
#40848=DIRECTION('center_axis',(3.34404360992196E-15,5.89417440552492E-13,
1.));
#40849=DIRECTION('ref_axis',(-0.707106781186543,-0.707106781186552,4.19145665077448E-13));
#40850=DIRECTION('center_axis',(3.34404360992239E-15,1.45135967092772E-12,
1.));
#40851=DIRECTION('ref_axis',(-0.707106781186543,-0.707106781186552,1.02863086116683E-12));
#40852=DIRECTION('',(3.34404360992196E-15,5.89417440552492E-13,1.));
#40853=DIRECTION('',(-3.34404360992196E-15,-5.89417440552492E-13,-1.));
#40854=DIRECTION('center_axis',(0.0929057196037781,-0.97991069492339,0.176475372898495));
#40855=DIRECTION('ref_axis',(0.456482036022066,0.199436781900346,0.867092336959786));
#40856=DIRECTION('center_axis',(5.00596043934382E-16,1.,-5.89417440552492E-13));
#40857=DIRECTION('ref_axis',(1.,-5.00596043936353E-16,-3.34404360992166E-15));
#40858=DIRECTION('center_axis',(4.89116698015727E-15,-0.899510317023533,
0.436899518846409));
#40859=DIRECTION('ref_axis',(3.22671189843336E-15,0.436899518846409,0.899510317023533));
#40860=DIRECTION('center_axis',(1.,-5.00596043936353E-16,-3.34404360992166E-15));
#40861=DIRECTION('ref_axis',(3.34404360992196E-15,5.89417440552492E-13,
1.));
#40862=DIRECTION('center_axis',(-1.01071973799428E-15,0.899510317023531,
-0.436899518846413));
#40863=DIRECTION('ref_axis',(0.707106781186553,0.308934612473437,0.636049844914594));
#40864=DIRECTION('',(1.01071973799428E-15,-0.899510317023531,0.436899518846413));
#40865=DIRECTION('center_axis',(1.,-5.00596043936353E-16,-3.34404360992166E-15));
#40866=DIRECTION('ref_axis',(3.37116090328272E-15,0.22415361136594,0.974553825353739));
#40867=DIRECTION('',(-1.,5.00596043936353E-16,3.34404360992166E-15));
#40868=DIRECTION('',(1.,-5.00596043936353E-16,-3.34404360992166E-15));
#40869=DIRECTION('center_axis',(-0.408248290463825,-0.816496580927991,-0.40824829046337));
#40870=DIRECTION('ref_axis',(0.577350269189588,-0.577350269189247,0.577350269190043));
#40871=DIRECTION('center_axis',(1.,-5.00596043936353E-16,-3.34404360992166E-15));
#40872=DIRECTION('ref_axis',(-5.00596043934382E-16,-1.,5.89417440552492E-13));
#40873=DIRECTION('center_axis',(3.34404360992196E-15,5.98299224749493E-13,
1.));
#40874=DIRECTION('ref_axis',(1.,-5.00596043936353E-16,-3.34404360992166E-15));
#40875=DIRECTION('center_axis',(-5.00596043934382E-16,-1.,5.89417440552492E-13));
#40876=DIRECTION('ref_axis',(3.34404360992196E-15,5.89417440552492E-13,
1.));
#40877=DIRECTION('center_axis',(-3.34404360992195E-15,-5.89417440552492E-13,
-1.));
#40878=DIRECTION('ref_axis',(0.707106781186522,-0.707106781186573,4.14416473251142E-13));
#40879=DIRECTION('center_axis',(3.34404360992239E-15,1.45135967092772E-12,
1.));
#40880=DIRECTION('ref_axis',(0.707106781186522,-0.707106781186573,1.02390166934054E-12));
#40881=DIRECTION('',(-3.34404360992195E-15,-5.89417440552492E-13,-1.));
#40882=DIRECTION('center_axis',(5.00596043934382E-16,1.,-5.89417440552492E-13));
#40883=DIRECTION('ref_axis',(0.707106781186528,4.16427094306996E-13,0.707106781186567));
#40884=DIRECTION('',(-5.00596043934382E-16,-1.,5.89417440552492E-13));
#40885=DIRECTION('center_axis',(1.,-5.00596043936353E-16,-3.34404360992166E-15));
#40886=DIRECTION('ref_axis',(2.01062105585817E-15,-0.707106781186137,0.707106781186958));
#40887=DIRECTION('',(-1.,5.00596043936353E-16,3.34404360992166E-15));
#40888=DIRECTION('',(1.,-5.00596043936353E-16,-3.34404360992166E-15));
#40889=DIRECTION('center_axis',(-1.01071973799428E-15,0.899510317023531,
-0.436899518846413));
#40890=DIRECTION('ref_axis',(-0.707106781186563,0.308934612473431,0.636049844914586));
#40891=DIRECTION('',(1.01071973799428E-15,-0.899510317023531,0.436899518846413));
#40892=DIRECTION('',(-1.01071973799428E-15,0.899510317023531,-0.436899518846413));
#40893=DIRECTION('center_axis',(5.00596043930822E-16,1.,-1.65391127897018E-12));
#40894=DIRECTION('ref_axis',(0.707106781186531,1.16913790598346E-12,0.707106781186564));
#40895=DIRECTION('',(-5.00596043930822E-16,-1.,1.65391127897018E-12));
#40896=DIRECTION('center_axis',(1.,-5.00596043936353E-16,-3.34404360992166E-15));
#40897=DIRECTION('ref_axis',(-3.37116090328261E-15,-0.224153611366358,-0.974553825353643));
#40898=DIRECTION('',(-1.,5.00596043936353E-16,3.34404360992166E-15));
#40899=DIRECTION('',(1.,-5.00596043936353E-16,-3.34404360992166E-15));
#40900=DIRECTION('center_axis',(5.00596043930822E-16,1.,-1.65391127897018E-12));
#40901=DIRECTION('ref_axis',(-0.707106781186547,1.16984585569803E-12,0.707106781186548));
#40902=DIRECTION('',(-5.00596043930822E-16,-1.,1.65391127897018E-12));
#40903=DIRECTION('',(5.00596043930822E-16,1.,-1.65391127897018E-12));
#40904=DIRECTION('center_axis',(-3.34404360992195E-15,-5.89417440552492E-13,
-1.));
#40905=DIRECTION('ref_axis',(0.707106781186648,0.707106781186447,-4.19145665077386E-13));
#40906=DIRECTION('',(3.34404360992195E-15,5.89417440552492E-13,1.));
#40907=DIRECTION('center_axis',(1.,-5.00596043936353E-16,-3.34404360992166E-15));
#40908=DIRECTION('ref_axis',(2.71857077045914E-15,0.707106781187448,0.707106781185647));
#40909=DIRECTION('',(-1.,5.00596043936353E-16,3.34404360992166E-15));
#40910=DIRECTION('',(1.,-5.00596043936353E-16,-3.34404360992166E-15));
#40911=DIRECTION('center_axis',(-3.34404360992196E-15,-5.89417440552492E-13,
-1.));
#40912=DIRECTION('ref_axis',(-0.707106781186668,0.707106781186427,-4.14416473251055E-13));
#40913=DIRECTION('',(3.34404360992196E-15,5.89417440552492E-13,1.));
#40914=DIRECTION('',(-3.34404360992196E-15,-5.89417440552492E-13,-1.));
#40915=DIRECTION('center_axis',(-5.005960439315E-16,-1.,1.45135967092772E-12));
#40916=DIRECTION('ref_axis',(0.707106781186527,-1.026620240111E-12,-0.707106781186568));
#40917=DIRECTION('',(5.005960439315E-16,1.,-1.45135967092772E-12));
#40918=DIRECTION('center_axis',(1.,-5.00596043936353E-16,-3.34404360992166E-15));
#40919=DIRECTION('ref_axis',(-2.01062105585943E-15,0.70710678118581,-0.707106781187285));
#40920=DIRECTION('',(-1.,5.00596043936353E-16,3.34404360992166E-15));
#40921=DIRECTION('',(1.,-5.00596043936353E-16,-3.34404360992166E-15));
#40922=DIRECTION('center_axis',(-5.00596043931499E-16,-1.,1.45135967092772E-12));
#40923=DIRECTION('ref_axis',(-0.707106781186551,-1.02591229039636E-12,-0.707106781186544));
#40924=DIRECTION('',(5.00596043931499E-16,1.,-1.45135967092772E-12));
#40925=DIRECTION('',(-5.00596043931499E-16,-1.,1.45135967092772E-12));
#40926=DIRECTION('center_axis',(1.01071973798223E-15,-0.899510317025162,
0.436899518843055));
#40927=DIRECTION('ref_axis',(0.707106781186558,-0.308934612471059,-0.636049844915743));
#40928=DIRECTION('center_axis',(1.,-5.00596043936353E-16,-3.34404360992166E-15));
#40929=DIRECTION('ref_axis',(-3.3711609032831E-15,-0.224153611364509,-0.974553825354069));
#40930=DIRECTION('',(1.,-5.00596043936353E-16,-3.34404360992166E-15));
#40931=DIRECTION('center_axis',(1.01071973798224E-15,-0.899510317025162,
0.436899518843055));
#40932=DIRECTION('ref_axis',(-0.70710678118655,-0.308934612471064,-0.63604984491575));
#40933=DIRECTION('center_axis',(-5.00596043936355E-16,-1.,-6.19091582357991E-16));
#40934=DIRECTION('ref_axis',(-2.96954721060321E-15,6.19091582357976E-16,
-1.));
#40935=DIRECTION('',(-1.01071973798224E-15,0.899510317025162,-0.436899518843055));
#40936=DIRECTION('center_axis',(-5.00596043934382E-16,-1.,5.89417440552492E-13));
#40937=DIRECTION('ref_axis',(-3.34404360992196E-15,-5.89417440552492E-13,
-1.));
#40938=DIRECTION('',(-3.34404360992166E-15,5.94374044734026E-16,-1.));
#40939=DIRECTION('',(1.,-1.44934907093772E-13,-3.34404360971203E-15));
#40940=DIRECTION('',(1.,-5.00596043936353E-16,-3.34404360992166E-15));
#40941=DIRECTION('',(-3.34404360992166E-15,5.94374044734026E-16,-1.));
#40942=DIRECTION('center_axis',(-3.34404360992239E-15,-1.45135967092772E-12,
-1.));
#40943=DIRECTION('ref_axis',(-1.,5.00596043936353E-16,3.34404360992166E-15));
#40944=DIRECTION('',(-5.00596043931499E-16,-1.,1.45135967092772E-12));
#40945=DIRECTION('',(-1.,5.00596043936353E-16,3.34404360992166E-15));
#40946=DIRECTION('',(5.00596043931499E-16,1.,-1.45135967092772E-12));
#40947=DIRECTION('center_axis',(-1.,5.00596043936353E-16,3.34404360992166E-15));
#40948=DIRECTION('ref_axis',(5.00596043934382E-16,1.,-5.89417440552492E-13));
#40949=DIRECTION('',(-3.34404360992166E-15,5.94374044734026E-16,-1.));
#40950=DIRECTION('',(-3.34404360992166E-15,6.19091582358092E-16,-1.));
#40951=DIRECTION('',(-5.00596043931499E-16,-1.,1.45135967092772E-12));
#40952=DIRECTION('',(-3.34404360992166E-15,6.19091582358092E-16,-1.));
#40953=DIRECTION('center_axis',(3.34404360992196E-15,5.89417440552492E-13,
1.));
#40954=DIRECTION('ref_axis',(-5.00596043934382E-16,-1.,5.89417440552492E-13));
#40955=DIRECTION('center_axis',(3.34404360992196E-15,5.89417440552492E-13,
1.));
#40956=DIRECTION('ref_axis',(5.00596043934382E-16,1.,-5.89417440552492E-13));
#40957=DIRECTION('center_axis',(3.34404360992196E-15,5.89417440552492E-13,
1.));
#40958=DIRECTION('ref_axis',(5.00596043934382E-16,1.,-5.89417440552492E-13));
#40959=DIRECTION('',(1.,-5.00596043936353E-16,-3.34404360992166E-15));
#40960=DIRECTION('',(-5.00596043934382E-16,-1.,5.89417440552492E-13));
#40961=DIRECTION('',(-1.,5.00596043936353E-16,3.34404360992166E-15));
#40962=DIRECTION('',(5.00596043934382E-16,1.,-5.89417440552492E-13));
#40963=DIRECTION('center_axis',(3.34404360992196E-15,5.89417440552492E-13,
1.));
#40964=DIRECTION('ref_axis',(5.00596043934382E-16,1.,-5.89417440552492E-13));
#40965=DIRECTION('center_axis',(3.34404360992196E-15,5.89417440552492E-13,
1.));
#40966=DIRECTION('ref_axis',(5.00596043934382E-16,1.,-5.89417440552492E-13));
#40967=DIRECTION('center_axis',(3.22671189843335E-15,0.436899518846413,
0.899510317023531));
#40968=DIRECTION('ref_axis',(1.01071973799428E-15,-0.899510317023531,0.436899518846413));
#40969=DIRECTION('center_axis',(3.34404360992249E-15,1.65391127897018E-12,
1.));
#40970=DIRECTION('ref_axis',(-5.00596043930822E-16,-1.,1.65391127897018E-12));
#40971=DIRECTION('center_axis',(5.00596043934382E-16,1.,-5.89417440552492E-13));
#40972=DIRECTION('ref_axis',(3.34404360992196E-15,5.89417440552492E-13,
1.));
#40973=DIRECTION('center_axis',(-3.34404360992239E-15,-1.45135967092772E-12,
-1.));
#40974=DIRECTION('ref_axis',(5.005960439315E-16,1.,-1.45135967092772E-12));
#40975=DIRECTION('center_axis',(3.34404360992196E-15,5.89417440552492E-13,
1.));
#40976=DIRECTION('ref_axis',(5.00596043934382E-16,1.,-5.89417440552492E-13));
#40977=DIRECTION('center_axis',(-3.34404360992196E-15,-5.89417440552492E-13,
-1.));
#40978=DIRECTION('ref_axis',(5.00596043934382E-16,1.,-5.89417440552492E-13));
#40979=DIRECTION('',(2.09721666198178E-15,-0.707106781051793,0.707106781321302));
#40980=DIRECTION('center_axis',(-3.34404360992166E-15,5.94374044734026E-16,
-1.));
#40981=DIRECTION('ref_axis',(5.00596043936355E-16,1.,5.94374044734015E-16));
#40982=DIRECTION('',(-3.34404360992166E-15,5.94374044734026E-16,-1.));
#40983=DIRECTION('center_axis',(3.34404360992166E-15,-5.94374044734026E-16,
1.));
#40984=DIRECTION('ref_axis',(-5.00596043936355E-16,-1.,-5.94374044734015E-16));
#40985=DIRECTION('center_axis',(3.34404360992166E-15,-5.94374044734026E-16,
1.));
#40986=DIRECTION('ref_axis',(-5.00596043936355E-16,-1.,-5.94374044734015E-16));
#40987=DIRECTION('center_axis',(3.34404360992196E-15,5.89417440552492E-13,
1.));
#40988=DIRECTION('ref_axis',(5.00596043934382E-16,1.,-5.89417440552492E-13));
#40989=DIRECTION('center_axis',(-3.34404360992196E-15,-5.89417440552492E-13,
-1.));
#40990=DIRECTION('ref_axis',(5.00596043934382E-16,1.,-5.89417440552492E-13));
#40991=DIRECTION('',(2.09721666164013E-15,-0.707106781143578,0.707106781229517));
#40992=DIRECTION('center_axis',(-3.34404360992166E-15,5.94374044734026E-16,
-1.));
#40993=DIRECTION('ref_axis',(5.00596043936355E-16,1.,5.94374044734015E-16));
#40994=DIRECTION('',(-3.34404360992166E-15,5.94374044734026E-16,-1.));
#40995=DIRECTION('center_axis',(3.34404360992166E-15,-5.94374044734026E-16,
1.));
#40996=DIRECTION('ref_axis',(-5.00596043936355E-16,-1.,-5.94374044734015E-16));
#40997=DIRECTION('center_axis',(3.34404360992166E-15,-5.94374044734026E-16,
1.));
#40998=DIRECTION('ref_axis',(-5.00596043936355E-16,-1.,-5.94374044734015E-16));
#40999=DIRECTION('center_axis',(3.34404360992196E-15,5.89417440552492E-13,
1.));
#41000=DIRECTION('ref_axis',(5.00596043934382E-16,1.,-5.89417440552492E-13));
#41001=DIRECTION('center_axis',(-3.34404360992196E-15,-5.89417440552492E-13,
-1.));
#41002=DIRECTION('ref_axis',(5.00596043934382E-16,1.,-5.89417440552492E-13));
#41003=DIRECTION('',(2.09721666164013E-15,-0.707106781143578,0.707106781229517));
#41004=DIRECTION('center_axis',(-3.34404360992166E-15,5.94374044734026E-16,
-1.));
#41005=DIRECTION('ref_axis',(5.00596043936355E-16,1.,5.94374044734015E-16));
#41006=DIRECTION('',(-3.34404360992166E-15,5.94374044734026E-16,-1.));
#41007=DIRECTION('center_axis',(3.34404360992166E-15,-5.94374044734026E-16,
1.));
#41008=DIRECTION('ref_axis',(-5.00596043936355E-16,-1.,-5.94374044734015E-16));
#41009=DIRECTION('center_axis',(3.34404360992166E-15,-5.94374044734026E-16,
1.));
#41010=DIRECTION('ref_axis',(-5.00596043936355E-16,-1.,-5.94374044734015E-16));
#41011=DIRECTION('center_axis',(3.34404360992196E-15,5.89417440552492E-13,
1.));
#41012=DIRECTION('ref_axis',(5.00596043934382E-16,1.,-5.89417440552492E-13));
#41013=DIRECTION('center_axis',(-3.34404360992196E-15,-5.89417440552492E-13,
-1.));
#41014=DIRECTION('ref_axis',(5.00596043934382E-16,1.,-5.89417440552492E-13));
#41015=DIRECTION('',(2.09721666198178E-15,-0.707106781051793,0.707106781321302));
#41016=DIRECTION('center_axis',(-3.34404360992166E-15,5.94374044734026E-16,
-1.));
#41017=DIRECTION('ref_axis',(5.00596043936355E-16,1.,5.94374044734015E-16));
#41018=DIRECTION('',(-3.34404360992166E-15,5.94374044734026E-16,-1.));
#41019=DIRECTION('center_axis',(3.34404360992166E-15,-5.94374044734026E-16,
1.));
#41020=DIRECTION('ref_axis',(-5.00596043936355E-16,-1.,-5.94374044734015E-16));
#41021=DIRECTION('center_axis',(3.34404360992166E-15,-5.94374044734026E-16,
1.));
#41022=DIRECTION('ref_axis',(-5.00596043936355E-16,-1.,-5.94374044734015E-16));
#41023=DIRECTION('center_axis',(-3.34404360992166E-15,1.22120854809198E-15,
-1.));
#41024=DIRECTION('ref_axis',(-5.00596043936357E-16,-1.,-1.22120854809206E-15));
#41025=DIRECTION('',(-1.92402545023304E-15,0.707106781186548,-0.707106781186547));
#41026=DIRECTION('center_axis',(-3.34404360992165E-15,1.4543884843594E-14,
-1.));
#41027=DIRECTION('ref_axis',(-5.00596043936402E-16,-1.,-1.45438848435941E-14));
#41028=DIRECTION('',(-1.92402545023302E-15,0.707106781186553,-0.707106781186542));
#41029=DIRECTION('center_axis',(-3.34404360992165E-15,1.4543884843594E-14,
-1.));
#41030=DIRECTION('ref_axis',(-5.00596043936402E-16,-1.,-1.45438848435941E-14));
#41031=DIRECTION('',(-1.92402545023302E-15,0.707106781186553,-0.707106781186542));
#41032=DIRECTION('center_axis',(-3.34404360992166E-15,1.22120854809198E-15,
-1.));
#41033=DIRECTION('ref_axis',(-5.00596043936357E-16,-1.,-1.22120854809206E-15));
#41034=DIRECTION('',(-1.92402545023304E-15,0.707106781186548,-0.707106781186547));
#41035=DIRECTION('center_axis',(5.00596043936355E-16,1.,5.94374044734026E-16));
#41036=DIRECTION('ref_axis',(1.,-5.00596043936353E-16,-3.34404360992166E-15));
#41037=DIRECTION('',(-3.34404360992166E-15,5.94374044734026E-16,-1.));
#41038=DIRECTION('center_axis',(1.,-5.00596043936353E-16,-3.34404360992166E-15));
#41039=DIRECTION('ref_axis',(-5.00596043936355E-16,-1.,-6.88301496270999E-16));
#41040=DIRECTION('center_axis',(-3.34404360992239E-15,-1.45135967092772E-12,
-1.));
#41041=DIRECTION('ref_axis',(-1.,5.00596043936353E-16,3.34404360992166E-15));
#41042=DIRECTION('',(-1.,5.00596043936353E-16,3.34404360992166E-15));
#41043=DIRECTION('',(5.00596043931499E-16,1.,-1.45135967092772E-12));
#41044=DIRECTION('',(1.,-5.00596043936353E-16,-3.34404360992166E-15));
#41045=DIRECTION('center_axis',(-5.00596043936355E-16,-1.,-6.19091582357991E-16));
#41046=DIRECTION('ref_axis',(-1.,5.00596043936353E-16,3.34404360992166E-15));
#41047=DIRECTION('',(-3.34404360992166E-15,6.19091582358092E-16,-1.));
#41048=DIRECTION('center_axis',(5.00596043936355E-16,1.,6.19091582357991E-16));
#41049=DIRECTION('ref_axis',(1.,-5.00596043936353E-16,-3.34404360992166E-15));
#41050=DIRECTION('',(-3.34404360992166E-15,6.19091582358092E-16,-1.));
#41051=DIRECTION('center_axis',(1.,-5.00596043936353E-16,-3.34404360992166E-15));
#41052=DIRECTION('ref_axis',(-5.00596043936355E-16,-1.,-6.88301496270999E-16));
#41053=DIRECTION('center_axis',(-1.,5.00596043936353E-16,3.34404360992166E-15));
#41054=DIRECTION('ref_axis',(5.00596043936355E-16,1.,6.88301496270999E-16));
#41055=DIRECTION('',(-5.00596043931499E-16,-1.,1.45135967092772E-12));
#41056=DIRECTION('',(-3.34404360992166E-15,5.94374044734026E-16,-1.));
#41057=DIRECTION('center_axis',(5.00596043936355E-16,1.,5.94374044734026E-16));
#41058=DIRECTION('ref_axis',(1.,-5.00596043936353E-16,-3.34404360992166E-15));
#41059=DIRECTION('',(-1.,5.00596043936353E-16,3.34404360992166E-15));
#41060=DIRECTION('center_axis',(-3.34404360992239E-15,-1.45135967092772E-12,
-1.));
#41061=DIRECTION('ref_axis',(-1.,5.00596043936353E-16,3.34404360992166E-15));
#41062=DIRECTION('center_axis',(-3.34404360992239E-15,-1.45135967092772E-12,
-1.));
#41063=DIRECTION('ref_axis',(-1.,5.00596043936353E-16,3.34404360992166E-15));
#41064=DIRECTION('',(1.,-5.00596043936353E-16,-3.34404360992166E-15));
#41065=DIRECTION('center_axis',(-5.00596043936355E-16,-1.,-6.19091582356982E-16));
#41066=DIRECTION('ref_axis',(-1.,5.00596043936353E-16,3.34404360992166E-15));
#41067=DIRECTION('center_axis',(-5.00596043936355E-16,-1.,-6.19091607820957E-16));
#41068=DIRECTION('ref_axis',(-1.,5.00596043936353E-16,3.34404360992166E-15));
#41069=DIRECTION('',(3.34404360992166E-15,-6.19091607821058E-16,1.));
#41070=DIRECTION('',(-3.34404360992166E-15,6.19091607821058E-16,-1.));
#41071=DIRECTION('center_axis',(1.,-5.00596043936353E-16,-3.34404360992166E-15));
#41072=DIRECTION('ref_axis',(-5.00596043936355E-16,-1.,-6.88301496270999E-16));
#41073=DIRECTION('',(3.34404360992166E-15,-6.19091607821058E-16,1.));
#41074=DIRECTION('center_axis',(5.00596043936355E-16,1.,6.19091607820957E-16));
#41075=DIRECTION('ref_axis',(1.,-5.00596043936353E-16,-3.34404360992166E-15));
#41076=DIRECTION('',(3.34404360992166E-15,-6.19091607821058E-16,1.));
#41077=DIRECTION('center_axis',(-1.,5.00596043936353E-16,3.34404360992166E-15));
#41078=DIRECTION('ref_axis',(5.00596043936355E-16,1.,6.88301496270999E-16));
#41079=DIRECTION('axis',(0.,0.,1.));
#41080=DIRECTION('refdir',(1.,0.,0.));
#41081=DIRECTION('center_axis',(-1.53651348736138E-16,-1.,1.45117688885522E-12));
#41082=DIRECTION('ref_axis',(-3.34404360992238E-15,-1.45117688885522E-12,
-1.));
#41083=DIRECTION('',(1.,-1.53651348740991E-16,-3.34404360992216E-15));
#41084=DIRECTION('',(3.34404360992238E-15,1.45117688885522E-12,1.));
#41085=DIRECTION('',(1.,-1.53651348740991E-16,-3.34404360992216E-15));
#41086=DIRECTION('',(3.34404360992238E-15,1.45117688885522E-12,1.));
#41087=DIRECTION('center_axis',(3.34404360992238E-15,1.45117688885522E-12,
1.));
#41088=DIRECTION('ref_axis',(5.00596043931499E-16,1.,-1.45117688885522E-12));
#41089=DIRECTION('center_axis',(3.34404360992238E-15,1.45117688885522E-12,
1.));
#41090=DIRECTION('ref_axis',(5.00596043931499E-16,1.,-1.45117688885522E-12));
#41091=DIRECTION('',(3.34404360992238E-15,1.45117688885522E-12,1.));
#41092=DIRECTION('center_axis',(3.34404360992238E-15,1.45117688885522E-12,
1.));
#41093=DIRECTION('ref_axis',(5.00596043931499E-16,1.,-1.45117688885522E-12));
#41094=DIRECTION('center_axis',(1.,-3.61818165858207E-16,-3.34404360992185E-15));
#41095=DIRECTION('ref_axis',(-3.34404360992238E-15,-1.45117688885522E-12,
-1.));
#41096=DIRECTION('',(3.61818165853354E-16,1.,-1.45117688885522E-12));
#41097=DIRECTION('',(3.34404360992238E-15,1.45117688885522E-12,1.));
#41098=DIRECTION('',(3.61818165853354E-16,1.,-1.45117688885522E-12));
#41099=DIRECTION('center_axis',(3.34404360992238E-15,1.45117688885522E-12,
1.));
#41100=DIRECTION('ref_axis',(-1.,5.00596043936352E-16,3.34404360992165E-15));
#41101=DIRECTION('center_axis',(3.34404360992238E-15,1.45117688885522E-12,
1.));
#41102=DIRECTION('ref_axis',(-1.,5.00596043936352E-16,3.34404360992165E-15));
#41103=DIRECTION('',(3.34404360992238E-15,1.45117688885522E-12,1.));
#41104=DIRECTION('center_axis',(3.34404360992238E-15,1.45117688885522E-12,
1.));
#41105=DIRECTION('ref_axis',(-1.,5.00596043936352E-16,3.34404360992165E-15));
#41106=DIRECTION('center_axis',(1.,-6.39373922014497E-16,-3.34404360992145E-15));
#41107=DIRECTION('ref_axis',(-3.34404360992238E-15,-1.45117688885522E-12,
-1.));
#41108=DIRECTION('',(-6.39373922009644E-16,-1.,1.45117688885522E-12));
#41109=DIRECTION('',(3.34404360992238E-15,1.45117688885522E-12,1.));
#41110=DIRECTION('',(-6.39373922009644E-16,-1.,1.45117688885522E-12));
#41111=DIRECTION('',(3.34404360992238E-15,1.45117688885522E-12,1.));
#41112=DIRECTION('center_axis',(3.34404360992238E-15,1.45117688885522E-12,
1.));
#41113=DIRECTION('ref_axis',(-5.45154683810787E-17,1.,-1.45117688885522E-12));
#41114=DIRECTION('center_axis',(-3.34404360992238E-15,-1.45117688885522E-12,
-1.));
#41115=DIRECTION('ref_axis',(-5.45154683810787E-17,1.,-1.45117688885522E-12));
#41116=DIRECTION('',(3.34404360992238E-15,1.45117688885522E-12,1.));
#41117=DIRECTION('center_axis',(-3.34404360992238E-15,-1.45117688885522E-12,
-1.));
#41118=DIRECTION('ref_axis',(-5.45154683810787E-17,1.,-1.45117688885522E-12));
#41119=DIRECTION('center_axis',(-5.00596043931499E-16,-1.,1.45117688885522E-12));
#41120=DIRECTION('ref_axis',(-3.34404360992238E-15,-1.45117688885522E-12,
-1.));
#41121=DIRECTION('',(-1.,5.00596043936352E-16,3.34404360992165E-15));
#41122=DIRECTION('',(3.34404360992238E-15,1.45117688885522E-12,1.));
#41123=DIRECTION('',(-1.,5.00596043936352E-16,3.34404360992165E-15));
#41124=DIRECTION('center_axis',(3.34404360992238E-15,1.45117688885522E-12,
1.));
#41125=DIRECTION('ref_axis',(1.,-5.00596043936352E-16,-3.34404360992165E-15));
#41126=DIRECTION('center_axis',(-3.34404360992238E-15,-1.45117688885522E-12,
-1.));
#41127=DIRECTION('ref_axis',(1.,-5.00596043936352E-16,-3.34404360992165E-15));
#41128=DIRECTION('',(3.34404360992238E-15,1.45117688885522E-12,1.));
#41129=DIRECTION('center_axis',(-3.34404360992238E-15,-1.45117688885522E-12,
-1.));
#41130=DIRECTION('ref_axis',(1.,-5.00596043936352E-16,-3.34404360992165E-15));
#41131=DIRECTION('center_axis',(3.61818165853354E-16,1.,-1.45117688885522E-12));
#41132=DIRECTION('ref_axis',(3.34404360992238E-15,1.45117688885522E-12,
1.));
#41133=DIRECTION('',(-1.,3.61818165858207E-16,3.34404360992185E-15));
#41134=DIRECTION('',(3.34404360992238E-15,1.45117688885522E-12,1.));
#41135=DIRECTION('',(-1.,3.61818165858207E-16,3.34404360992185E-15));
#41136=DIRECTION('center_axis',(3.34404360992238E-15,1.45117688885522E-12,
1.));
#41137=DIRECTION('ref_axis',(1.,-5.00596043936352E-16,-3.34404360992165E-15));
#41138=DIRECTION('center_axis',(3.34404360992238E-15,1.45117688885522E-12,
1.));
#41139=DIRECTION('ref_axis',(1.,-5.00596043936352E-16,-3.34404360992165E-15));
#41140=DIRECTION('center_axis',(3.34404360992238E-15,1.45117688885522E-12,
1.));
#41141=DIRECTION('ref_axis',(1.,-5.00596043936352E-16,-3.34404360992165E-15));
#41142=DIRECTION('',(3.34404360992238E-15,1.45117688885522E-12,1.));
#41143=DIRECTION('center_axis',(-1.,3.61818165858207E-16,3.34404360992185E-15));
#41144=DIRECTION('ref_axis',(3.34404360992238E-15,1.45117688885522E-12,
1.));
#41145=DIRECTION('',(-3.61818165853354E-16,-1.,1.45117688885522E-12));
#41146=DIRECTION('',(-3.61818165853354E-16,-1.,1.45117688885522E-12));
#41147=DIRECTION('',(3.34404360992238E-15,1.45117688885522E-12,1.));
#41148=DIRECTION('center_axis',(3.34404360992238E-15,1.45117688885522E-12,
1.));
#41149=DIRECTION('ref_axis',(-5.00596043931499E-16,-1.,1.45117688885522E-12));
#41150=DIRECTION('center_axis',(3.34404360992238E-15,1.45117688885522E-12,
1.));
#41151=DIRECTION('ref_axis',(-5.00596043931499E-16,-1.,1.45117688885522E-12));
#41152=DIRECTION('center_axis',(3.34404360992238E-15,1.45117688885522E-12,
1.));
#41153=DIRECTION('ref_axis',(-5.00596043931499E-16,-1.,1.45117688885522E-12));
#41154=DIRECTION('center_axis',(-1.,5.00596043936352E-16,3.34404360992165E-15));
#41155=DIRECTION('ref_axis',(3.34404360992238E-15,1.45117688885522E-12,
1.));
#41156=DIRECTION('',(5.00596043931499E-16,1.,-1.45117688885522E-12));
#41157=DIRECTION('',(3.34404360992238E-15,1.45117688885522E-12,1.));
#41158=DIRECTION('',(5.00596043931499E-16,1.,-1.45117688885522E-12));
#41159=DIRECTION('center_axis',(3.34404360992238E-15,1.45117688885522E-12,
1.));
#41160=DIRECTION('ref_axis',(-5.00596043931499E-16,-1.,1.45117688885522E-12));
#41161=DIRECTION('center_axis',(-3.34404360992238E-15,-1.45117688885522E-12,
-1.));
#41162=DIRECTION('ref_axis',(-5.00596043931499E-16,-1.,1.45117688885522E-12));
#41163=DIRECTION('',(3.34404360992238E-15,1.45117688885522E-12,1.));
#41164=DIRECTION('center_axis',(-3.34404360992238E-15,-1.45117688885522E-12,
-1.));
#41165=DIRECTION('ref_axis',(-5.00596043931499E-16,-1.,1.45117688885522E-12));
#41166=DIRECTION('center_axis',(-5.45154683810787E-17,1.,-1.45117688885522E-12));
#41167=DIRECTION('ref_axis',(3.34404360992238E-15,1.45117688885522E-12,
1.));
#41168=DIRECTION('',(1.,5.45154683762259E-17,-3.34404360992246E-15));
#41169=DIRECTION('',(3.34404360992238E-15,1.45117688885522E-12,1.));
#41170=DIRECTION('',(1.,5.45154683762259E-17,-3.34404360992246E-15));
#41171=DIRECTION('center_axis',(3.34404360992238E-15,1.45117688885522E-12,
1.));
#41172=DIRECTION('ref_axis',(-1.,5.00596043936352E-16,3.34404360992165E-15));
#41173=DIRECTION('center_axis',(-3.34404360992238E-15,-1.45117688885522E-12,
-1.));
#41174=DIRECTION('ref_axis',(-1.,5.00596043936352E-16,3.34404360992165E-15));
#41175=DIRECTION('center_axis',(-3.34404360992238E-15,-1.45117688885522E-12,
-1.));
#41176=DIRECTION('ref_axis',(-1.,5.00596043936352E-16,3.34404360992165E-15));
#41177=DIRECTION('center_axis',(3.34404360992238E-15,1.45117688885522E-12,
1.));
#41178=DIRECTION('ref_axis',(1.,-5.00596043936352E-16,-3.34404360992165E-15));
#41179=DIRECTION('center_axis',(3.34404360992238E-15,1.45117688885522E-12,
1.));
#41180=DIRECTION('ref_axis',(1.,-5.00596043936352E-16,-3.34404360992165E-15));
#41181=DIRECTION('center_axis',(-1.53651348736138E-16,-1.,1.45117688885522E-12));
#41182=DIRECTION('ref_axis',(-3.34404360992238E-15,-1.45117688885522E-12,
-1.));
#41183=DIRECTION('',(1.,-1.53651348740991E-16,-3.34404360992216E-15));
#41184=DIRECTION('',(3.34404360992238E-15,1.45117688885522E-12,1.));
#41185=DIRECTION('',(1.,-1.53651348740991E-16,-3.34404360992216E-15));
#41186=DIRECTION('',(3.34404360992238E-15,1.45117688885522E-12,1.));
#41187=DIRECTION('center_axis',(3.34404360992238E-15,1.45117688885522E-12,
1.));
#41188=DIRECTION('ref_axis',(5.00596043931499E-16,1.,-1.45117688885522E-12));
#41189=DIRECTION('center_axis',(3.34404360992238E-15,1.45117688885522E-12,
1.));
#41190=DIRECTION('ref_axis',(5.00596043931499E-16,1.,-1.45117688885522E-12));
#41191=DIRECTION('',(3.34404360992238E-15,1.45117688885522E-12,1.));
#41192=DIRECTION('center_axis',(3.34404360992238E-15,1.45117688885522E-12,
1.));
#41193=DIRECTION('ref_axis',(5.00596043931499E-16,1.,-1.45117688885522E-12));
#41194=DIRECTION('center_axis',(1.,-3.61818165858207E-16,-3.34404360992185E-15));
#41195=DIRECTION('ref_axis',(-3.34404360992238E-15,-1.45117688885522E-12,
-1.));
#41196=DIRECTION('',(3.61818165853354E-16,1.,-1.45117688885522E-12));
#41197=DIRECTION('',(3.34404360992238E-15,1.45117688885522E-12,1.));
#41198=DIRECTION('',(3.61818165853354E-16,1.,-1.45117688885522E-12));
#41199=DIRECTION('center_axis',(3.34404360992238E-15,1.45117688885522E-12,
1.));
#41200=DIRECTION('ref_axis',(-1.,5.00596043936352E-16,3.34404360992165E-15));
#41201=DIRECTION('center_axis',(3.34404360992238E-15,1.45117688885522E-12,
1.));
#41202=DIRECTION('ref_axis',(-1.,5.00596043936352E-16,3.34404360992165E-15));
#41203=DIRECTION('',(3.34404360992238E-15,1.45117688885522E-12,1.));
#41204=DIRECTION('center_axis',(3.34404360992238E-15,1.45117688885522E-12,
1.));
#41205=DIRECTION('ref_axis',(-1.,5.00596043936352E-16,3.34404360992165E-15));
#41206=DIRECTION('center_axis',(1.,-6.39373922014497E-16,-3.34404360992145E-15));
#41207=DIRECTION('ref_axis',(-3.34404360992238E-15,-1.45117688885522E-12,
-1.));
#41208=DIRECTION('',(-6.39373922009644E-16,-1.,1.45117688885522E-12));
#41209=DIRECTION('',(3.34404360992238E-15,1.45117688885522E-12,1.));
#41210=DIRECTION('',(-6.39373922009644E-16,-1.,1.45117688885522E-12));
#41211=DIRECTION('',(3.34404360992238E-15,1.45117688885522E-12,1.));
#41212=DIRECTION('center_axis',(3.34404360992238E-15,1.45117688885522E-12,
1.));
#41213=DIRECTION('ref_axis',(-5.45154683810787E-17,1.,-1.45117688885522E-12));
#41214=DIRECTION('center_axis',(-3.34404360992238E-15,-1.45117688885522E-12,
-1.));
#41215=DIRECTION('ref_axis',(-5.45154683810787E-17,1.,-1.45117688885522E-12));
#41216=DIRECTION('',(3.34404360992238E-15,1.45117688885522E-12,1.));
#41217=DIRECTION('center_axis',(-3.34404360992238E-15,-1.45117688885522E-12,
-1.));
#41218=DIRECTION('ref_axis',(-5.45154683810787E-17,1.,-1.45117688885522E-12));
#41219=DIRECTION('center_axis',(-5.00596043931499E-16,-1.,1.45117688885522E-12));
#41220=DIRECTION('ref_axis',(-3.34404360992238E-15,-1.45117688885522E-12,
-1.));
#41221=DIRECTION('',(-1.,5.00596043936352E-16,3.34404360992165E-15));
#41222=DIRECTION('',(3.34404360992238E-15,1.45117688885522E-12,1.));
#41223=DIRECTION('',(-1.,5.00596043936352E-16,3.34404360992165E-15));
#41224=DIRECTION('center_axis',(3.34404360992238E-15,1.45117688885522E-12,
1.));
#41225=DIRECTION('ref_axis',(1.,-5.00596043936352E-16,-3.34404360992165E-15));
#41226=DIRECTION('center_axis',(-3.34404360992238E-15,-1.45117688885522E-12,
-1.));
#41227=DIRECTION('ref_axis',(1.,-5.00596043936352E-16,-3.34404360992165E-15));
#41228=DIRECTION('',(3.34404360992238E-15,1.45117688885522E-12,1.));
#41229=DIRECTION('center_axis',(-3.34404360992238E-15,-1.45117688885522E-12,
-1.));
#41230=DIRECTION('ref_axis',(1.,-5.00596043936352E-16,-3.34404360992165E-15));
#41231=DIRECTION('center_axis',(3.61818165853354E-16,1.,-1.45117688885522E-12));
#41232=DIRECTION('ref_axis',(3.34404360992238E-15,1.45117688885522E-12,
1.));
#41233=DIRECTION('',(-1.,3.61818165858207E-16,3.34404360992185E-15));
#41234=DIRECTION('',(3.34404360992238E-15,1.45117688885522E-12,1.));
#41235=DIRECTION('',(-1.,3.61818165858207E-16,3.34404360992185E-15));
#41236=DIRECTION('center_axis',(3.34404360992238E-15,1.45117688885522E-12,
1.));
#41237=DIRECTION('ref_axis',(1.,-5.00596043936352E-16,-3.34404360992165E-15));
#41238=DIRECTION('center_axis',(3.34404360992238E-15,1.45117688885522E-12,
1.));
#41239=DIRECTION('ref_axis',(1.,-5.00596043936352E-16,-3.34404360992165E-15));
#41240=DIRECTION('center_axis',(3.34404360992238E-15,1.45117688885522E-12,
1.));
#41241=DIRECTION('ref_axis',(1.,-5.00596043936352E-16,-3.34404360992165E-15));
#41242=DIRECTION('',(3.34404360992238E-15,1.45117688885522E-12,1.));
#41243=DIRECTION('center_axis',(-1.,3.61818165858207E-16,3.34404360992185E-15));
#41244=DIRECTION('ref_axis',(3.34404360992238E-15,1.45117688885522E-12,
1.));
#41245=DIRECTION('',(-3.61818165853354E-16,-1.,1.45117688885522E-12));
#41246=DIRECTION('',(-3.61818165853354E-16,-1.,1.45117688885522E-12));
#41247=DIRECTION('',(3.34404360992238E-15,1.45117688885522E-12,1.));
#41248=DIRECTION('center_axis',(3.34404360992238E-15,1.45117688885522E-12,
1.));
#41249=DIRECTION('ref_axis',(-5.00596043931499E-16,-1.,1.45117688885522E-12));
#41250=DIRECTION('center_axis',(3.34404360992238E-15,1.45117688885522E-12,
1.));
#41251=DIRECTION('ref_axis',(-5.00596043931499E-16,-1.,1.45117688885522E-12));
#41252=DIRECTION('center_axis',(3.34404360992238E-15,1.45117688885522E-12,
1.));
#41253=DIRECTION('ref_axis',(-5.00596043931499E-16,-1.,1.45117688885522E-12));
#41254=DIRECTION('center_axis',(-1.,5.00596043936352E-16,3.34404360992165E-15));
#41255=DIRECTION('ref_axis',(3.34404360992238E-15,1.45117688885522E-12,
1.));
#41256=DIRECTION('',(5.00596043931499E-16,1.,-1.45117688885522E-12));
#41257=DIRECTION('',(3.34404360992238E-15,1.45117688885522E-12,1.));
#41258=DIRECTION('',(5.00596043931499E-16,1.,-1.45117688885522E-12));
#41259=DIRECTION('center_axis',(3.34404360992238E-15,1.45117688885522E-12,
1.));
#41260=DIRECTION('ref_axis',(-5.00596043931499E-16,-1.,1.45117688885522E-12));
#41261=DIRECTION('center_axis',(-3.34404360992238E-15,-1.45117688885522E-12,
-1.));
#41262=DIRECTION('ref_axis',(-5.00596043931499E-16,-1.,1.45117688885522E-12));
#41263=DIRECTION('',(3.34404360992238E-15,1.45117688885522E-12,1.));
#41264=DIRECTION('center_axis',(-3.34404360992238E-15,-1.45117688885522E-12,
-1.));
#41265=DIRECTION('ref_axis',(-5.00596043931499E-16,-1.,1.45117688885522E-12));
#41266=DIRECTION('center_axis',(-5.45154683810787E-17,1.,-1.45117688885522E-12));
#41267=DIRECTION('ref_axis',(3.34404360992238E-15,1.45117688885522E-12,
1.));
#41268=DIRECTION('',(1.,5.45154683762259E-17,-3.34404360992246E-15));
#41269=DIRECTION('',(3.34404360992238E-15,1.45117688885522E-12,1.));
#41270=DIRECTION('',(1.,5.45154683762259E-17,-3.34404360992246E-15));
#41271=DIRECTION('center_axis',(3.34404360992238E-15,1.45117688885522E-12,
1.));
#41272=DIRECTION('ref_axis',(-1.,5.00596043936352E-16,3.34404360992165E-15));
#41273=DIRECTION('center_axis',(-3.34404360992238E-15,-1.45117688885522E-12,
-1.));
#41274=DIRECTION('ref_axis',(-1.,5.00596043936352E-16,3.34404360992165E-15));
#41275=DIRECTION('center_axis',(-3.34404360992238E-15,-1.45117688885522E-12,
-1.));
#41276=DIRECTION('ref_axis',(-1.,5.00596043936352E-16,3.34404360992165E-15));
#41277=DIRECTION('center_axis',(3.34404360992238E-15,1.45117688885522E-12,
1.));
#41278=DIRECTION('ref_axis',(1.,-5.00596043936352E-16,-3.34404360992165E-15));
#41279=DIRECTION('center_axis',(3.34404360992238E-15,1.45117688885522E-12,
1.));
#41280=DIRECTION('ref_axis',(1.,-5.00596043936352E-16,-3.34404360992165E-15));
#41281=DIRECTION('center_axis',(-1.53651348736138E-16,-1.,1.45117688885522E-12));
#41282=DIRECTION('ref_axis',(-3.34404360992238E-15,-1.45117688885522E-12,
-1.));
#41283=DIRECTION('',(1.,-1.53651348740991E-16,-3.34404360992216E-15));
#41284=DIRECTION('',(3.34404360992238E-15,1.45117688885522E-12,1.));
#41285=DIRECTION('',(1.,-1.53651348740991E-16,-3.34404360992216E-15));
#41286=DIRECTION('',(3.34404360992238E-15,1.45117688885522E-12,1.));
#41287=DIRECTION('center_axis',(3.34404360992238E-15,1.45117688885522E-12,
1.));
#41288=DIRECTION('ref_axis',(5.00596043931499E-16,1.,-1.45117688885522E-12));
#41289=DIRECTION('center_axis',(3.34404360992238E-15,1.45117688885522E-12,
1.));
#41290=DIRECTION('ref_axis',(5.00596043931499E-16,1.,-1.45117688885522E-12));
#41291=DIRECTION('',(3.34404360992238E-15,1.45117688885522E-12,1.));
#41292=DIRECTION('center_axis',(3.34404360992238E-15,1.45117688885522E-12,
1.));
#41293=DIRECTION('ref_axis',(5.00596043931499E-16,1.,-1.45117688885522E-12));
#41294=DIRECTION('center_axis',(1.,-3.61818165858207E-16,-3.34404360992185E-15));
#41295=DIRECTION('ref_axis',(-3.34404360992238E-15,-1.45117688885522E-12,
-1.));
#41296=DIRECTION('',(3.61818165853354E-16,1.,-1.45117688885522E-12));
#41297=DIRECTION('',(3.34404360992238E-15,1.45117688885522E-12,1.));
#41298=DIRECTION('',(3.61818165853354E-16,1.,-1.45117688885522E-12));
#41299=DIRECTION('center_axis',(3.34404360992238E-15,1.45117688885522E-12,
1.));
#41300=DIRECTION('ref_axis',(-1.,5.00596043936352E-16,3.34404360992165E-15));
#41301=DIRECTION('center_axis',(3.34404360992238E-15,1.45117688885522E-12,
1.));
#41302=DIRECTION('ref_axis',(-1.,5.00596043936352E-16,3.34404360992165E-15));
#41303=DIRECTION('',(3.34404360992238E-15,1.45117688885522E-12,1.));
#41304=DIRECTION('center_axis',(3.34404360992238E-15,1.45117688885522E-12,
1.));
#41305=DIRECTION('ref_axis',(-1.,5.00596043936352E-16,3.34404360992165E-15));
#41306=DIRECTION('center_axis',(1.,-6.39373922014497E-16,-3.34404360992145E-15));
#41307=DIRECTION('ref_axis',(-3.34404360992238E-15,-1.45117688885522E-12,
-1.));
#41308=DIRECTION('',(-6.39373922009644E-16,-1.,1.45117688885522E-12));
#41309=DIRECTION('',(3.34404360992238E-15,1.45117688885522E-12,1.));
#41310=DIRECTION('',(-6.39373922009644E-16,-1.,1.45117688885522E-12));
#41311=DIRECTION('',(3.34404360992238E-15,1.45117688885522E-12,1.));
#41312=DIRECTION('center_axis',(3.34404360992238E-15,1.45117688885522E-12,
1.));
#41313=DIRECTION('ref_axis',(-5.45154683810787E-17,1.,-1.45117688885522E-12));
#41314=DIRECTION('center_axis',(-3.34404360992238E-15,-1.45117688885522E-12,
-1.));
#41315=DIRECTION('ref_axis',(-5.45154683810787E-17,1.,-1.45117688885522E-12));
#41316=DIRECTION('',(3.34404360992238E-15,1.45117688885522E-12,1.));
#41317=DIRECTION('center_axis',(-3.34404360992238E-15,-1.45117688885522E-12,
-1.));
#41318=DIRECTION('ref_axis',(-5.45154683810787E-17,1.,-1.45117688885522E-12));
#41319=DIRECTION('center_axis',(-5.00596043931499E-16,-1.,1.45117688885522E-12));
#41320=DIRECTION('ref_axis',(-3.34404360992238E-15,-1.45117688885522E-12,
-1.));
#41321=DIRECTION('',(-1.,5.00596043936352E-16,3.34404360992165E-15));
#41322=DIRECTION('',(3.34404360992238E-15,1.45117688885522E-12,1.));
#41323=DIRECTION('',(-1.,5.00596043936352E-16,3.34404360992165E-15));
#41324=DIRECTION('center_axis',(3.34404360992238E-15,1.45117688885522E-12,
1.));
#41325=DIRECTION('ref_axis',(1.,-5.00596043936352E-16,-3.34404360992165E-15));
#41326=DIRECTION('center_axis',(-3.34404360992238E-15,-1.45117688885522E-12,
-1.));
#41327=DIRECTION('ref_axis',(1.,-5.00596043936352E-16,-3.34404360992165E-15));
#41328=DIRECTION('',(3.34404360992238E-15,1.45117688885522E-12,1.));
#41329=DIRECTION('center_axis',(-3.34404360992238E-15,-1.45117688885522E-12,
-1.));
#41330=DIRECTION('ref_axis',(1.,-5.00596043936352E-16,-3.34404360992165E-15));
#41331=DIRECTION('center_axis',(3.61818165853354E-16,1.,-1.45117688885522E-12));
#41332=DIRECTION('ref_axis',(3.34404360992238E-15,1.45117688885522E-12,
1.));
#41333=DIRECTION('',(-1.,3.61818165858207E-16,3.34404360992185E-15));
#41334=DIRECTION('',(3.34404360992238E-15,1.45117688885522E-12,1.));
#41335=DIRECTION('',(-1.,3.61818165858207E-16,3.34404360992185E-15));
#41336=DIRECTION('center_axis',(3.34404360992238E-15,1.45117688885522E-12,
1.));
#41337=DIRECTION('ref_axis',(1.,-5.00596043936352E-16,-3.34404360992165E-15));
#41338=DIRECTION('center_axis',(3.34404360992238E-15,1.45117688885522E-12,
1.));
#41339=DIRECTION('ref_axis',(1.,-5.00596043936352E-16,-3.34404360992165E-15));
#41340=DIRECTION('center_axis',(3.34404360992238E-15,1.45117688885522E-12,
1.));
#41341=DIRECTION('ref_axis',(1.,-5.00596043936352E-16,-3.34404360992165E-15));
#41342=DIRECTION('',(3.34404360992238E-15,1.45117688885522E-12,1.));
#41343=DIRECTION('center_axis',(-1.,3.61818165858207E-16,3.34404360992185E-15));
#41344=DIRECTION('ref_axis',(3.34404360992238E-15,1.45117688885522E-12,
1.));
#41345=DIRECTION('',(-3.61818165853354E-16,-1.,1.45117688885522E-12));
#41346=DIRECTION('',(-3.61818165853354E-16,-1.,1.45117688885522E-12));
#41347=DIRECTION('',(3.34404360992238E-15,1.45117688885522E-12,1.));
#41348=DIRECTION('center_axis',(3.34404360992238E-15,1.45117688885522E-12,
1.));
#41349=DIRECTION('ref_axis',(-5.00596043931499E-16,-1.,1.45117688885522E-12));
#41350=DIRECTION('center_axis',(3.34404360992238E-15,1.45117688885522E-12,
1.));
#41351=DIRECTION('ref_axis',(-5.00596043931499E-16,-1.,1.45117688885522E-12));
#41352=DIRECTION('center_axis',(3.34404360992238E-15,1.45117688885522E-12,
1.));
#41353=DIRECTION('ref_axis',(-5.00596043931499E-16,-1.,1.45117688885522E-12));
#41354=DIRECTION('center_axis',(-1.,5.00596043936352E-16,3.34404360992165E-15));
#41355=DIRECTION('ref_axis',(3.34404360992238E-15,1.45117688885522E-12,
1.));
#41356=DIRECTION('',(5.00596043931499E-16,1.,-1.45117688885522E-12));
#41357=DIRECTION('',(3.34404360992238E-15,1.45117688885522E-12,1.));
#41358=DIRECTION('',(5.00596043931499E-16,1.,-1.45117688885522E-12));
#41359=DIRECTION('center_axis',(3.34404360992238E-15,1.45117688885522E-12,
1.));
#41360=DIRECTION('ref_axis',(-5.00596043931499E-16,-1.,1.45117688885522E-12));
#41361=DIRECTION('center_axis',(-3.34404360992238E-15,-1.45117688885522E-12,
-1.));
#41362=DIRECTION('ref_axis',(-5.00596043931499E-16,-1.,1.45117688885522E-12));
#41363=DIRECTION('',(3.34404360992238E-15,1.45117688885522E-12,1.));
#41364=DIRECTION('center_axis',(-3.34404360992238E-15,-1.45117688885522E-12,
-1.));
#41365=DIRECTION('ref_axis',(-5.00596043931499E-16,-1.,1.45117688885522E-12));
#41366=DIRECTION('center_axis',(-5.45154683810787E-17,1.,-1.45117688885522E-12));
#41367=DIRECTION('ref_axis',(3.34404360992238E-15,1.45117688885522E-12,
1.));
#41368=DIRECTION('',(1.,5.45154683762259E-17,-3.34404360992246E-15));
#41369=DIRECTION('',(3.34404360992238E-15,1.45117688885522E-12,1.));
#41370=DIRECTION('',(1.,5.45154683762259E-17,-3.34404360992246E-15));
#41371=DIRECTION('center_axis',(3.34404360992238E-15,1.45117688885522E-12,
1.));
#41372=DIRECTION('ref_axis',(-1.,5.00596043936352E-16,3.34404360992165E-15));
#41373=DIRECTION('center_axis',(-3.34404360992238E-15,-1.45117688885522E-12,
-1.));
#41374=DIRECTION('ref_axis',(-1.,5.00596043936352E-16,3.34404360992165E-15));
#41375=DIRECTION('center_axis',(-3.34404360992238E-15,-1.45117688885522E-12,
-1.));
#41376=DIRECTION('ref_axis',(-1.,5.00596043936352E-16,3.34404360992165E-15));
#41377=DIRECTION('center_axis',(3.34404360992238E-15,1.45117688885522E-12,
1.));
#41378=DIRECTION('ref_axis',(1.,-5.00596043936352E-16,-3.34404360992165E-15));
#41379=DIRECTION('center_axis',(3.34404360992238E-15,1.45117688885522E-12,
1.));
#41380=DIRECTION('ref_axis',(1.,-5.00596043936352E-16,-3.34404360992165E-15));
#41381=DIRECTION('center_axis',(-1.53651348736138E-16,-1.,1.45117688885522E-12));
#41382=DIRECTION('ref_axis',(-3.34404360992238E-15,-1.45117688885522E-12,
-1.));
#41383=DIRECTION('',(1.,-1.53651348740991E-16,-3.34404360992216E-15));
#41384=DIRECTION('',(3.34404360992238E-15,1.45117688885522E-12,1.));
#41385=DIRECTION('',(1.,-1.53651348740991E-16,-3.34404360992216E-15));
#41386=DIRECTION('',(3.34404360992238E-15,1.45117688885522E-12,1.));
#41387=DIRECTION('center_axis',(3.34404360992238E-15,1.45117688885522E-12,
1.));
#41388=DIRECTION('ref_axis',(5.00596043931499E-16,1.,-1.45117688885522E-12));
#41389=DIRECTION('center_axis',(3.34404360992238E-15,1.45117688885522E-12,
1.));
#41390=DIRECTION('ref_axis',(5.00596043931499E-16,1.,-1.45117688885522E-12));
#41391=DIRECTION('',(3.34404360992238E-15,1.45117688885522E-12,1.));
#41392=DIRECTION('center_axis',(3.34404360992238E-15,1.45117688885522E-12,
1.));
#41393=DIRECTION('ref_axis',(5.00596043931499E-16,1.,-1.45117688885522E-12));
#41394=DIRECTION('center_axis',(1.,-3.61818165858207E-16,-3.34404360992185E-15));
#41395=DIRECTION('ref_axis',(-3.34404360992238E-15,-1.45117688885522E-12,
-1.));
#41396=DIRECTION('',(3.61818165853354E-16,1.,-1.45117688885522E-12));
#41397=DIRECTION('',(3.34404360992238E-15,1.45117688885522E-12,1.));
#41398=DIRECTION('',(3.61818165853354E-16,1.,-1.45117688885522E-12));
#41399=DIRECTION('center_axis',(3.34404360992238E-15,1.45117688885522E-12,
1.));
#41400=DIRECTION('ref_axis',(-1.,5.00596043936352E-16,3.34404360992165E-15));
#41401=DIRECTION('center_axis',(3.34404360992238E-15,1.45117688885522E-12,
1.));
#41402=DIRECTION('ref_axis',(-1.,5.00596043936352E-16,3.34404360992165E-15));
#41403=DIRECTION('',(3.34404360992238E-15,1.45117688885522E-12,1.));
#41404=DIRECTION('center_axis',(3.34404360992238E-15,1.45117688885522E-12,
1.));
#41405=DIRECTION('ref_axis',(-1.,5.00596043936352E-16,3.34404360992165E-15));
#41406=DIRECTION('center_axis',(1.,-6.39373922014497E-16,-3.34404360992145E-15));
#41407=DIRECTION('ref_axis',(-3.34404360992238E-15,-1.45117688885522E-12,
-1.));
#41408=DIRECTION('',(-6.39373922009644E-16,-1.,1.45117688885522E-12));
#41409=DIRECTION('',(3.34404360992238E-15,1.45117688885522E-12,1.));
#41410=DIRECTION('',(-6.39373922009644E-16,-1.,1.45117688885522E-12));
#41411=DIRECTION('',(3.34404360992238E-15,1.45117688885522E-12,1.));
#41412=DIRECTION('center_axis',(3.34404360992238E-15,1.45117688885522E-12,
1.));
#41413=DIRECTION('ref_axis',(-5.45154683810787E-17,1.,-1.45117688885522E-12));
#41414=DIRECTION('center_axis',(-3.34404360992238E-15,-1.45117688885522E-12,
-1.));
#41415=DIRECTION('ref_axis',(-5.45154683810787E-17,1.,-1.45117688885522E-12));
#41416=DIRECTION('',(3.34404360992238E-15,1.45117688885522E-12,1.));
#41417=DIRECTION('center_axis',(-3.34404360992238E-15,-1.45117688885522E-12,
-1.));
#41418=DIRECTION('ref_axis',(-5.45154683810787E-17,1.,-1.45117688885522E-12));
#41419=DIRECTION('center_axis',(-5.00596043931499E-16,-1.,1.45117688885522E-12));
#41420=DIRECTION('ref_axis',(-3.34404360992238E-15,-1.45117688885522E-12,
-1.));
#41421=DIRECTION('',(-1.,5.00596043936352E-16,3.34404360992165E-15));
#41422=DIRECTION('',(3.34404360992238E-15,1.45117688885522E-12,1.));
#41423=DIRECTION('',(-1.,5.00596043936352E-16,3.34404360992165E-15));
#41424=DIRECTION('center_axis',(3.34404360992238E-15,1.45117688885522E-12,
1.));
#41425=DIRECTION('ref_axis',(1.,-5.00596043936352E-16,-3.34404360992165E-15));
#41426=DIRECTION('center_axis',(-3.34404360992238E-15,-1.45117688885522E-12,
-1.));
#41427=DIRECTION('ref_axis',(1.,-5.00596043936352E-16,-3.34404360992165E-15));
#41428=DIRECTION('',(3.34404360992238E-15,1.45117688885522E-12,1.));
#41429=DIRECTION('center_axis',(-3.34404360992238E-15,-1.45117688885522E-12,
-1.));
#41430=DIRECTION('ref_axis',(1.,-5.00596043936352E-16,-3.34404360992165E-15));
#41431=DIRECTION('center_axis',(3.61818165853354E-16,1.,-1.45117688885522E-12));
#41432=DIRECTION('ref_axis',(3.34404360992238E-15,1.45117688885522E-12,
1.));
#41433=DIRECTION('',(-1.,3.61818165858207E-16,3.34404360992185E-15));
#41434=DIRECTION('',(3.34404360992238E-15,1.45117688885522E-12,1.));
#41435=DIRECTION('',(-1.,3.61818165858207E-16,3.34404360992185E-15));
#41436=DIRECTION('center_axis',(3.34404360992238E-15,1.45117688885522E-12,
1.));
#41437=DIRECTION('ref_axis',(1.,-5.00596043936352E-16,-3.34404360992165E-15));
#41438=DIRECTION('center_axis',(3.34404360992238E-15,1.45117688885522E-12,
1.));
#41439=DIRECTION('ref_axis',(1.,-5.00596043936352E-16,-3.34404360992165E-15));
#41440=DIRECTION('center_axis',(3.34404360992238E-15,1.45117688885522E-12,
1.));
#41441=DIRECTION('ref_axis',(1.,-5.00596043936352E-16,-3.34404360992165E-15));
#41442=DIRECTION('',(3.34404360992238E-15,1.45117688885522E-12,1.));
#41443=DIRECTION('center_axis',(-1.,3.61818165858207E-16,3.34404360992185E-15));
#41444=DIRECTION('ref_axis',(3.34404360992238E-15,1.45117688885522E-12,
1.));
#41445=DIRECTION('',(-3.61818165853354E-16,-1.,1.45117688885522E-12));
#41446=DIRECTION('',(-3.61818165853354E-16,-1.,1.45117688885522E-12));
#41447=DIRECTION('',(3.34404360992238E-15,1.45117688885522E-12,1.));
#41448=DIRECTION('center_axis',(3.34404360992238E-15,1.45117688885522E-12,
1.));
#41449=DIRECTION('ref_axis',(-5.00596043931499E-16,-1.,1.45117688885522E-12));
#41450=DIRECTION('center_axis',(3.34404360992238E-15,1.45117688885522E-12,
1.));
#41451=DIRECTION('ref_axis',(-5.00596043931499E-16,-1.,1.45117688885522E-12));
#41452=DIRECTION('center_axis',(3.34404360992238E-15,1.45117688885522E-12,
1.));
#41453=DIRECTION('ref_axis',(-5.00596043931499E-16,-1.,1.45117688885522E-12));
#41454=DIRECTION('center_axis',(-1.,5.00596043936352E-16,3.34404360992165E-15));
#41455=DIRECTION('ref_axis',(3.34404360992238E-15,1.45117688885522E-12,
1.));
#41456=DIRECTION('',(5.00596043931499E-16,1.,-1.45117688885522E-12));
#41457=DIRECTION('',(3.34404360992238E-15,1.45117688885522E-12,1.));
#41458=DIRECTION('',(5.00596043931499E-16,1.,-1.45117688885522E-12));
#41459=DIRECTION('center_axis',(3.34404360992238E-15,1.45117688885522E-12,
1.));
#41460=DIRECTION('ref_axis',(-5.00596043931499E-16,-1.,1.45117688885522E-12));
#41461=DIRECTION('center_axis',(-3.34404360992238E-15,-1.45117688885522E-12,
-1.));
#41462=DIRECTION('ref_axis',(-5.00596043931499E-16,-1.,1.45117688885522E-12));
#41463=DIRECTION('',(3.34404360992238E-15,1.45117688885522E-12,1.));
#41464=DIRECTION('center_axis',(-3.34404360992238E-15,-1.45117688885522E-12,
-1.));
#41465=DIRECTION('ref_axis',(-5.00596043931499E-16,-1.,1.45117688885522E-12));
#41466=DIRECTION('center_axis',(-5.45154683810787E-17,1.,-1.45117688885522E-12));
#41467=DIRECTION('ref_axis',(3.34404360992238E-15,1.45117688885522E-12,
1.));
#41468=DIRECTION('',(1.,5.45154683762259E-17,-3.34404360992246E-15));
#41469=DIRECTION('',(3.34404360992238E-15,1.45117688885522E-12,1.));
#41470=DIRECTION('',(1.,5.45154683762259E-17,-3.34404360992246E-15));
#41471=DIRECTION('center_axis',(3.34404360992238E-15,1.45117688885522E-12,
1.));
#41472=DIRECTION('ref_axis',(-1.,5.00596043936352E-16,3.34404360992165E-15));
#41473=DIRECTION('center_axis',(-3.34404360992238E-15,-1.45117688885522E-12,
-1.));
#41474=DIRECTION('ref_axis',(-1.,5.00596043936352E-16,3.34404360992165E-15));
#41475=DIRECTION('center_axis',(-3.34404360992238E-15,-1.45117688885522E-12,
-1.));
#41476=DIRECTION('ref_axis',(-1.,5.00596043936352E-16,3.34404360992165E-15));
#41477=DIRECTION('center_axis',(3.34404360992238E-15,1.45117688885522E-12,
1.));
#41478=DIRECTION('ref_axis',(1.,-5.00596043936352E-16,-3.34404360992165E-15));
#41479=DIRECTION('center_axis',(3.34404360992238E-15,1.45117688885522E-12,
1.));
#41480=DIRECTION('ref_axis',(1.,-5.00596043936352E-16,-3.34404360992165E-15));
#41481=DIRECTION('center_axis',(-0.707106781186547,0.707106781186548,-1.02377242289756E-12));
#41482=DIRECTION('ref_axis',(-0.707106781186548,-0.707106781186547,1.02850161472388E-12));
#41483=DIRECTION('center_axis',(-0.707106781186547,0.707106781186548,-1.02377242289756E-12));
#41484=DIRECTION('ref_axis',(-0.707106781186548,-0.707106781186547,1.02850161472388E-12));
#41485=DIRECTION('',(0.707106781186548,0.707106781186547,-1.02889413783855E-12));
#41486=DIRECTION('center_axis',(-0.707106781186547,0.707106781186548,-1.02377242289756E-12));
#41487=DIRECTION('ref_axis',(0.707106781186548,0.707106781186547,-1.02850161472388E-12));
#41488=DIRECTION('',(-3.20526573184424E-15,-1.45117688885522E-12,-1.));
#41489=DIRECTION('center_axis',(-0.707106781186547,0.707106781186548,-1.02377242289756E-12));
#41490=DIRECTION('ref_axis',(0.707106781186548,0.707106781186547,-1.02889413783855E-12));
#41491=DIRECTION('',(-0.707106781186548,-0.707106781186547,1.02850161472388E-12));
#41492=DIRECTION('center_axis',(-0.707106781186547,0.707106781186548,-1.02377242289756E-12));
#41493=DIRECTION('ref_axis',(-0.707106781186548,-0.707106781186547,1.02850161472388E-12));
#41494=DIRECTION('',(-3.34404360992239E-15,-1.45117688885522E-12,-1.));
#41495=DIRECTION('',(-0.707106781186548,-0.707106781186547,1.02859974550255E-12));
#41496=DIRECTION('center_axis',(0.707106781186547,-0.707106781186548,1.02377242289756E-12));
#41497=DIRECTION('ref_axis',(-0.707106781186548,-0.707106781186547,1.02850161472388E-12));
#41498=DIRECTION('',(3.48282148800053E-15,1.4513156667333E-12,1.));
#41499=DIRECTION('center_axis',(0.707106781186547,-0.707106781186548,1.02377242289756E-12));
#41500=DIRECTION('ref_axis',(-0.707106781186548,-0.707106781186547,1.02850161472388E-12));
#41501=DIRECTION('',(0.707106781186548,0.707106781186547,-1.02874694167055E-12));
#41502=DIRECTION('center_axis',(0.707106781186547,-0.707106781186548,1.02377242289756E-12));
#41503=DIRECTION('ref_axis',(0.707106781186548,0.707106781186547,-1.02850161472388E-12));
#41504=DIRECTION('',(-3.48282148800053E-15,-1.4513156667333E-12,-1.));
#41505=DIRECTION('center_axis',(0.707106781186547,-0.707106781186548,1.02377242289756E-12));
#41506=DIRECTION('ref_axis',(0.707106781186548,0.707106781186547,-1.02850161472388E-12));
#41507=DIRECTION('center_axis',(-3.69098830511775E-15,-1.45117688885522E-12,
-1.));
#41508=DIRECTION('ref_axis',(-5.00596043931499E-16,-1.,1.45117688885522E-12));
#41509=DIRECTION('',(5.00596043931499E-16,1.,-1.45117688885522E-12));
#41510=DIRECTION('',(-0.707106781186304,0.707106781186791,-1.02352709595125E-12));
#41511=DIRECTION('',(5.00596043931499E-16,1.,-1.45117688885522E-12));
#41512=DIRECTION('center_axis',(5.00596043931499E-16,1.,-1.45117688885522E-12));
#41513=DIRECTION('ref_axis',(-1.,5.00596043936352E-16,3.34404360992166E-15));
#41514=DIRECTION('',(5.00596043931499E-16,1.,-1.45117688885522E-12));
#41515=DIRECTION('center_axis',(0.707106781186791,0.707106781186304,-1.02850161472353E-12));
#41516=DIRECTION('ref_axis',(-0.707106781186304,0.707106781186791,-1.02377242289792E-12));
#41517=DIRECTION('center_axis',(1.,-5.00596043936553E-16,-3.48282148799981E-15));
#41518=DIRECTION('ref_axis',(5.00596043931499E-16,1.,-1.45117688885522E-12));
#41519=DIRECTION('',(5.00596043931499E-16,1.,-1.45117688885522E-12));
#41520=DIRECTION('',(-3.48282148800053E-15,-1.45103811097714E-12,-1.));
#41521=DIRECTION('center_axis',(5.00596043931499E-16,1.,-1.45117688885522E-12));
#41522=DIRECTION('ref_axis',(-3.34404360992239E-15,-1.45117688885522E-12,
-1.));
#41523=DIRECTION('',(5.00596043931499E-16,1.,-1.45117688885522E-12));
#41524=DIRECTION('center_axis',(0.707106781186791,0.707106781186304,-1.02850161472353E-12));
#41525=DIRECTION('ref_axis',(-0.707106781186304,0.707106781186791,-1.02377242289792E-12));
#41526=DIRECTION('center_axis',(5.00596043931499E-16,1.,-1.45117688885522E-12));
#41527=DIRECTION('ref_axis',(3.89915512223497E-15,1.45117688885522E-12,
1.));
#41528=DIRECTION('',(5.00596043931499E-16,1.,-1.45117688885522E-12));
#41529=DIRECTION('center_axis',(-0.707106781186791,-0.707106781186304,1.02850161472353E-12));
#41530=DIRECTION('ref_axis',(0.707106781186304,-0.707106781186791,1.02337989978325E-12));
#41531=DIRECTION('',(5.00596043931499E-16,1.,-1.45117688885522E-12));
#41532=DIRECTION('center_axis',(5.00596043931499E-16,1.,-1.45117688885522E-12));
#41533=DIRECTION('ref_axis',(1.,-5.00596043936352E-16,-3.34404360992166E-15));
#41534=DIRECTION('',(5.00596043931499E-16,1.,-1.45117688885522E-12));
#41535=DIRECTION('center_axis',(-0.707106781186791,-0.707106781186304,1.02850161472353E-12));
#41536=DIRECTION('ref_axis',(0.707106781186304,-0.707106781186791,1.02377242289792E-12));
#41537=DIRECTION('',(5.00596043931499E-16,1.,-1.45117688885522E-12));
#41538=DIRECTION('center_axis',(3.89915512223496E-15,1.45117688885522E-12,
1.));
#41539=DIRECTION('ref_axis',(5.00596043931499E-16,1.,-1.45117688885522E-12));
#41540=DIRECTION('',(5.00596043931499E-16,1.,-1.45117688885522E-12));
#41541=DIRECTION('',(-0.707106781186304,0.707106781186791,-1.02337989978325E-12));
#41542=DIRECTION('center_axis',(-0.707106781186791,-0.707106781186304,1.02850161472353E-12));
#41543=DIRECTION('ref_axis',(0.707106781186304,-0.707106781186791,1.02377242289792E-12));
#41544=DIRECTION('',(-3.20526573184424E-15,-1.45117688885522E-12,-1.));
#41545=DIRECTION('center_axis',(-0.707106781186791,-0.707106781186304,1.02850161472353E-12));
#41546=DIRECTION('ref_axis',(-0.707106781186304,0.707106781186791,-1.02377242289792E-12));
#41547=DIRECTION('',(3.34404360992239E-15,1.45117688885522E-12,1.));
#41548=DIRECTION('center_axis',(-0.707106781186791,-0.707106781186304,1.02850161472353E-12));
#41549=DIRECTION('ref_axis',(-0.707106781186304,0.707106781186791,-1.02377242289792E-12));
#41550=DIRECTION('',(0.707106781186304,-0.707106781186791,1.02377242289792E-12));
#41551=DIRECTION('',(0.707106781186304,-0.707106781186791,1.02367429211925E-12));
#41552=DIRECTION('center_axis',(0.707106781186791,0.707106781186304,-1.02850161472353E-12));
#41553=DIRECTION('ref_axis',(0.707106781186304,-0.707106781186791,1.02377242289792E-12));
#41554=DIRECTION('',(3.48282148800053E-15,1.45103811097714E-12,1.));
#41555=DIRECTION('center_axis',(0.707106781186791,0.707106781186304,-1.02850161472353E-12));
#41556=DIRECTION('ref_axis',(0.707106781186304,-0.707106781186791,1.02377242289792E-12));
#41557=DIRECTION('center_axis',(3.48282148800053E-15,1.45117688885522E-12,
1.));
#41558=DIRECTION('ref_axis',(5.00596043931499E-16,1.,-1.45117688885522E-12));
#41559=DIRECTION('',(5.00596043931499E-16,1.,-1.45117688885522E-12));
#41560=DIRECTION('center_axis',(5.00596043931499E-16,1.,-1.45117688885522E-12));
#41561=DIRECTION('ref_axis',(-3.34404360992239E-15,-1.45117688885522E-12,
-1.));
#41562=DIRECTION('',(5.00596043931499E-16,1.,-1.45117688885522E-12));
#41563=DIRECTION('center_axis',(5.00596043931499E-16,1.,-1.45117688885522E-12));
#41564=DIRECTION('ref_axis',(3.34404360992239E-15,1.45117688885522E-12,
1.));
#41565=DIRECTION('',(5.00596043931499E-16,1.,-1.45117688885522E-12));
#41566=DIRECTION('center_axis',(-1.,5.00596043936553E-16,3.48282148799981E-15));
#41567=DIRECTION('ref_axis',(-5.00596043931499E-16,-1.,1.45117688885522E-12));
#41568=DIRECTION('',(5.00596043931499E-16,1.,-1.45117688885522E-12));
#41569=DIRECTION('center_axis',(5.00596043931499E-16,1.,-1.45117688885522E-12));
#41570=DIRECTION('ref_axis',(1.,-5.00596043936352E-16,-3.34404360992166E-15));
#41571=DIRECTION('center_axis',(-1.,5.0059604393615E-16,3.20526573184352E-15));
#41572=DIRECTION('ref_axis',(-5.00596043931499E-16,-1.,1.45117688885522E-12));
#41573=DIRECTION('center_axis',(-3.34404360992239E-15,-1.45117688885522E-12,
-1.));
#41574=DIRECTION('ref_axis',(-5.00596043931499E-16,-1.,1.45117688885522E-12));
#41575=DIRECTION('',(5.00596043931499E-16,1.,-1.45117688885522E-12));
#41576=DIRECTION('center_axis',(5.00596043931499E-16,1.,-1.45117688885522E-12));
#41577=DIRECTION('ref_axis',(-1.,5.00596043936352E-16,3.34404360992166E-15));
#41578=DIRECTION('',(5.00596043931499E-16,1.,-1.45117688885522E-12));
#41579=DIRECTION('center_axis',(1.,-5.00596043936352E-16,-3.34404360992166E-15));
#41580=DIRECTION('ref_axis',(5.00596043931499E-16,1.,-1.45117688885522E-12));
#41581=DIRECTION('center_axis',(0.707106781186548,0.707106781186547,-1.02850161472388E-12));
#41582=DIRECTION('ref_axis',(-0.707106781186547,0.707106781186548,-1.02377242289756E-12));
#41583=DIRECTION('center_axis',(0.707106781186548,0.707106781186547,-1.02850161472388E-12));
#41584=DIRECTION('ref_axis',(-0.707106781186547,0.707106781186548,-1.02377242289756E-12));
#41585=DIRECTION('',(0.707106781186547,-0.707106781186548,1.02337989978289E-12));
#41586=DIRECTION('center_axis',(0.707106781186548,0.707106781186547,-1.02850161472388E-12));
#41587=DIRECTION('ref_axis',(0.707106781186547,-0.707106781186548,1.02377242289756E-12));
#41588=DIRECTION('',(3.20526573184424E-15,1.4513156667333E-12,1.));
#41589=DIRECTION('center_axis',(0.707106781186548,0.707106781186547,-1.02850161472388E-12));
#41590=DIRECTION('ref_axis',(0.707106781186547,-0.707106781186548,1.02337989978289E-12));
#41591=DIRECTION('',(-0.707106781186547,0.707106781186548,-1.02377242289756E-12));
#41592=DIRECTION('center_axis',(0.707106781186548,0.707106781186547,-1.02850161472388E-12));
#41593=DIRECTION('ref_axis',(-0.707106781186547,0.707106781186548,-1.02377242289756E-12));
#41594=DIRECTION('',(3.34404360992239E-15,1.45117688885522E-12,1.));
#41595=DIRECTION('',(-0.707106781186547,0.707106781186548,-1.0236742921189E-12));
#41596=DIRECTION('center_axis',(-0.707106781186548,-0.707106781186547,1.02850161472388E-12));
#41597=DIRECTION('ref_axis',(-0.707106781186547,0.707106781186548,-1.02377242289756E-12));
#41598=DIRECTION('',(3.48282148800053E-15,1.45103811097714E-12,1.));
#41599=DIRECTION('center_axis',(-0.707106781186548,-0.707106781186547,1.02850161472388E-12));
#41600=DIRECTION('ref_axis',(-0.707106781186547,0.707106781186548,-1.02377242289756E-12));
#41601=DIRECTION('',(0.707106781186547,-0.707106781186548,1.0235270959509E-12));
#41602=DIRECTION('center_axis',(-0.707106781186548,-0.707106781186547,1.02850161472388E-12));
#41603=DIRECTION('ref_axis',(0.707106781186547,-0.707106781186548,1.02377242289756E-12));
#41604=DIRECTION('',(-3.48282148800053E-15,-1.45103811097714E-12,-1.));
#41605=DIRECTION('center_axis',(-0.707106781186548,-0.707106781186547,1.02850161472388E-12));
#41606=DIRECTION('ref_axis',(0.707106781186547,-0.707106781186548,1.02377242289756E-12));
#41607=DIRECTION('center_axis',(-3.69098830511775E-15,-1.45117688885522E-12,
-1.));
#41608=DIRECTION('ref_axis',(-5.00596043931499E-16,-1.,1.45117688885522E-12));
#41609=DIRECTION('',(5.00596043931499E-16,1.,-1.45117688885522E-12));
#41610=DIRECTION('',(-0.707106781186304,-0.707106781186791,1.0287469416709E-12));
#41611=DIRECTION('',(5.00596043931499E-16,1.,-1.45117688885522E-12));
#41612=DIRECTION('center_axis',(5.00596043931499E-16,1.,-1.45117688885522E-12));
#41613=DIRECTION('ref_axis',(-1.,5.00596043936352E-16,3.34404360992166E-15));
#41614=DIRECTION('',(5.00596043931499E-16,1.,-1.45117688885522E-12));
#41615=DIRECTION('center_axis',(-0.707106781186791,0.707106781186304,-1.02377242289721E-12));
#41616=DIRECTION('ref_axis',(-0.707106781186304,-0.707106781186791,1.02850161472423E-12));
#41617=DIRECTION('center_axis',(1.,-5.00596043936553E-16,-3.48282148799981E-15));
#41618=DIRECTION('ref_axis',(5.00596043931499E-16,1.,-1.45117688885522E-12));
#41619=DIRECTION('',(5.00596043931499E-16,1.,-1.45117688885522E-12));
#41620=DIRECTION('',(-3.48282148800053E-15,-1.4513156667333E-12,-1.));
#41621=DIRECTION('center_axis',(5.00596043931499E-16,1.,-1.45117688885522E-12));
#41622=DIRECTION('ref_axis',(-3.34404360992239E-15,-1.45117688885522E-12,
-1.));
#41623=DIRECTION('',(5.00596043931499E-16,1.,-1.45117688885522E-12));
#41624=DIRECTION('center_axis',(-0.707106781186791,0.707106781186304,-1.02377242289721E-12));
#41625=DIRECTION('ref_axis',(-0.707106781186304,-0.707106781186791,1.02850161472423E-12));
#41626=DIRECTION('center_axis',(5.00596043931499E-16,1.,-1.45117688885522E-12));
#41627=DIRECTION('ref_axis',(3.89915512223497E-15,1.45117688885522E-12,
1.));
#41628=DIRECTION('',(5.00596043931499E-16,1.,-1.45117688885522E-12));
#41629=DIRECTION('center_axis',(0.707106781186791,-0.707106781186304,1.02377242289721E-12));
#41630=DIRECTION('ref_axis',(0.707106781186304,0.707106781186791,-1.02889413783891E-12));
#41631=DIRECTION('',(5.00596043931499E-16,1.,-1.45117688885522E-12));
#41632=DIRECTION('center_axis',(-1.,5.0059604393615E-16,3.20526573184352E-15));
#41633=DIRECTION('ref_axis',(-5.00596043931499E-16,-1.,1.45117688885522E-12));
#41634=DIRECTION('',(5.00596043931499E-16,1.,-1.45117688885522E-12));
#41635=DIRECTION('',(-3.20526573184424E-15,-1.45103811097714E-12,-1.));
#41636=DIRECTION('center_axis',(5.00596043931499E-16,1.,-1.45117688885522E-12));
#41637=DIRECTION('ref_axis',(1.,-5.00596043936352E-16,-3.34404360992166E-15));
#41638=DIRECTION('',(5.00596043931499E-16,1.,-1.45117688885522E-12));
#41639=DIRECTION('center_axis',(0.707106781186791,-0.707106781186304,1.02377242289721E-12));
#41640=DIRECTION('ref_axis',(0.707106781186304,0.707106781186791,-1.02850161472423E-12));
#41641=DIRECTION('center_axis',(3.89915512223496E-15,1.45117688885522E-12,
1.));
#41642=DIRECTION('ref_axis',(5.00596043931499E-16,1.,-1.45117688885522E-12));
#41643=DIRECTION('',(5.00596043931499E-16,1.,-1.45117688885522E-12));
#41644=DIRECTION('',(-0.707106781186304,-0.707106781186791,1.02889413783891E-12));
#41645=DIRECTION('center_axis',(0.707106781186791,-0.707106781186304,1.02377242289721E-12));
#41646=DIRECTION('ref_axis',(0.707106781186304,0.707106781186791,-1.02850161472423E-12));
#41647=DIRECTION('center_axis',(0.707106781186791,-0.707106781186304,1.02377242289721E-12));
#41648=DIRECTION('ref_axis',(-0.707106781186304,-0.707106781186791,1.02850161472423E-12));
#41649=DIRECTION('',(3.34404360992239E-15,1.45117688885522E-12,1.));
#41650=DIRECTION('center_axis',(0.707106781186791,-0.707106781186304,1.02377242289721E-12));
#41651=DIRECTION('ref_axis',(-0.707106781186304,-0.707106781186791,1.02850161472423E-12));
#41652=DIRECTION('',(0.707106781186304,0.707106781186791,-1.02850161472423E-12));
#41653=DIRECTION('',(0.707106781186304,0.707106781186791,-1.0285997455029E-12));
#41654=DIRECTION('center_axis',(-0.707106781186791,0.707106781186304,-1.02377242289721E-12));
#41655=DIRECTION('ref_axis',(0.707106781186304,0.707106781186791,-1.02850161472423E-12));
#41656=DIRECTION('',(3.48282148800053E-15,1.4513156667333E-12,1.));
#41657=DIRECTION('center_axis',(-0.707106781186791,0.707106781186304,-1.02377242289721E-12));
#41658=DIRECTION('ref_axis',(0.707106781186304,0.707106781186791,-1.02850161472423E-12));
#41659=DIRECTION('center_axis',(3.48282148800053E-15,1.45117688885522E-12,
1.));
#41660=DIRECTION('ref_axis',(5.00596043931499E-16,1.,-1.45117688885522E-12));
#41661=DIRECTION('',(5.00596043931499E-16,1.,-1.45117688885522E-12));
#41662=DIRECTION('center_axis',(5.00596043931499E-16,1.,-1.45117688885522E-12));
#41663=DIRECTION('ref_axis',(-3.34404360992239E-15,-1.45117688885522E-12,
-1.));
#41664=DIRECTION('',(5.00596043931499E-16,1.,-1.45117688885522E-12));
#41665=DIRECTION('center_axis',(5.00596043931499E-16,1.,-1.45117688885522E-12));
#41666=DIRECTION('ref_axis',(3.34404360992239E-15,1.45117688885522E-12,
1.));
#41667=DIRECTION('',(5.00596043931499E-16,1.,-1.45117688885522E-12));
#41668=DIRECTION('center_axis',(-1.,5.00596043936553E-16,3.48282148799981E-15));
#41669=DIRECTION('ref_axis',(-5.00596043931499E-16,-1.,1.45117688885522E-12));
#41670=DIRECTION('',(5.00596043931499E-16,1.,-1.45117688885522E-12));
#41671=DIRECTION('center_axis',(5.00596043931499E-16,1.,-1.45117688885522E-12));
#41672=DIRECTION('ref_axis',(1.,-5.00596043936352E-16,-3.34404360992166E-15));
#41673=DIRECTION('center_axis',(-3.34404360992239E-15,-1.45117688885522E-12,
-1.));
#41674=DIRECTION('ref_axis',(-5.00596043931499E-16,-1.,1.45117688885522E-12));
#41675=DIRECTION('',(5.00596043931499E-16,1.,-1.45117688885522E-12));
#41676=DIRECTION('center_axis',(5.00596043931499E-16,1.,-1.45117688885522E-12));
#41677=DIRECTION('ref_axis',(-1.,5.00596043936352E-16,3.34404360992166E-15));
#41678=DIRECTION('',(5.00596043931499E-16,1.,-1.45117688885522E-12));
#41679=DIRECTION('center_axis',(1.,-5.00596043936352E-16,-3.34404360992166E-15));
#41680=DIRECTION('ref_axis',(5.00596043931499E-16,1.,-1.45117688885522E-12));
#41681=DIRECTION('center_axis',(-0.707106781186792,0.707106781186303,-1.02360964389904E-12));
#41682=DIRECTION('ref_axis',(-8.58100867314579E-13,5.89501773663249E-13,
1.));
#41683=DIRECTION('',(0.707106781186303,0.707106781186792,-4.19016418634642E-13));
#41684=DIRECTION('center_axis',(-0.707106781186792,0.707106781186303,-1.02360964389904E-12));
#41685=DIRECTION('ref_axis',(0.707106781186303,0.707106781186792,-4.19016418634642E-13));
#41686=DIRECTION('',(-8.58367982497838E-13,5.89234658479989E-13,1.));
#41687=DIRECTION('center_axis',(-0.707106781186792,0.707106781186303,-1.02360964389904E-12));
#41688=DIRECTION('ref_axis',(0.707106781186303,0.707106781186792,-4.18623895519971E-13));
#41689=DIRECTION('',(-0.707106781186303,-0.707106781186792,4.1911454941331E-13));
#41690=DIRECTION('center_axis',(-0.707106781186792,0.707106781186303,-1.02360964389904E-12));
#41691=DIRECTION('ref_axis',(-0.707106781186303,-0.707106781186792,4.19016418634642E-13));
#41692=DIRECTION('',(-3.34404360992195E-15,-5.88679546967676E-13,-1.));
#41693=DIRECTION('center_axis',(-0.707106781186792,0.707106781186303,-1.02360964389904E-12));
#41694=DIRECTION('ref_axis',(-0.707106781186303,-0.707106781186792,4.19016418634642E-13));
#41695=DIRECTION('',(-8.58506760375916E-13,5.89095880601911E-13,1.));
#41696=DIRECTION('center_axis',(0.707106781186792,-0.707106781186303,1.02360964389904E-12));
#41697=DIRECTION('ref_axis',(-0.707106781186303,-0.707106781186792,4.19016418634642E-13));
#41698=DIRECTION('',(0.707106781186303,0.707106781186792,-4.18918287855974E-13));
#41699=DIRECTION('center_axis',(0.707106781186792,-0.707106781186303,1.02360964389904E-12));
#41700=DIRECTION('ref_axis',(0.707106781186303,0.707106781186792,-4.19016418634642E-13));
#41701=DIRECTION('',(8.58714927193033E-13,-5.88887713784794E-13,-1.));
#41702=DIRECTION('center_axis',(0.707106781186792,-0.707106781186303,1.02360964389904E-12));
#41703=DIRECTION('ref_axis',(0.707106781186303,0.707106781186792,-4.19016418634642E-13));
#41704=DIRECTION('',(-0.707106781186303,-0.707106781186792,4.18918287855974E-13));
#41705=DIRECTION('center_axis',(0.707106781186792,-0.707106781186303,1.02360964389904E-12));
#41706=DIRECTION('ref_axis',(-0.707106781186303,-0.707106781186792,4.19016418634642E-13));
#41707=DIRECTION('center_axis',(-5.00596043934383E-16,-1.,5.88887713784794E-13));
#41708=DIRECTION('ref_axis',(-1.,5.00596043936352E-16,3.34404360992166E-15));
#41709=DIRECTION('',(-1.,5.00596043936352E-16,3.34404360992166E-15));
#41710=DIRECTION('',(8.65180980907738E-13,5.88887713784793E-13,1.));
#41711=DIRECTION('',(-1.,5.00596043936352E-16,3.34404360992166E-15));
#41712=DIRECTION('center_axis',(1.,-5.00596043936352E-16,-3.34404360992166E-15));
#41713=DIRECTION('ref_axis',(5.00596043934382E-16,1.,-5.89234658479989E-13));
#41714=DIRECTION('',(-1.,5.00596043936352E-16,3.34404360992166E-15));
#41715=DIRECTION('center_axis',(-0.707106781186791,-0.707106781186304,1.02818183432823E-12));
#41716=DIRECTION('ref_axis',(-0.707106781186304,0.707106781186791,-4.14287226808325E-13));
#41717=DIRECTION('center_axis',(-3.34404360992196E-15,-5.89095880601911E-13,
-1.));
#41718=DIRECTION('ref_axis',(-1.,5.00596043936352E-16,3.34404360992166E-15));
#41719=DIRECTION('',(-1.,5.00596043936352E-16,3.34404360992166E-15));
#41720=DIRECTION('',(0.707106781186304,-0.707106781186791,4.14189096029657E-13));
#41721=DIRECTION('center_axis',(1.,-5.00596043936352E-16,-3.34404360992166E-15));
#41722=DIRECTION('ref_axis',(3.34404360992196E-15,5.89234658479989E-13,
1.));
#41723=DIRECTION('',(-1.,5.00596043936352E-16,3.34404360992166E-15));
#41724=DIRECTION('center_axis',(-0.707106781186791,-0.707106781186304,1.02818183432823E-12));
#41725=DIRECTION('ref_axis',(0.707106781186304,-0.707106781186791,4.14287226808325E-13));
#41726=DIRECTION('center_axis',(-3.34404360992196E-15,-5.89373436358067E-13,
-1.));
#41727=DIRECTION('ref_axis',(-1.,5.00596043936352E-16,3.34404360992166E-15));
#41728=DIRECTION('',(-1.,5.00596043936352E-16,3.34404360992166E-15));
#41729=DIRECTION('',(-0.707106781186304,0.707106781186791,-4.14385357586993E-13));
#41730=DIRECTION('',(-1.,5.00596043936352E-16,3.34404360992166E-15));
#41731=DIRECTION('center_axis',(1.,-5.00596043936352E-16,-3.34404360992166E-15));
#41732=DIRECTION('ref_axis',(5.00596043934384E-16,1.,-5.88679546967676E-13));
#41733=DIRECTION('',(-1.,5.00596043936352E-16,3.34404360992166E-15));
#41734=DIRECTION('center_axis',(0.707106781186791,0.707106781186304,-1.02818183432823E-12));
#41735=DIRECTION('ref_axis',(-0.707106781186304,0.707106781186791,-4.13894703693654E-13));
#41736=DIRECTION('center_axis',(-5.00596043934382E-16,-1.,5.89234658479989E-13));
#41737=DIRECTION('ref_axis',(-1.,5.00596043936352E-16,3.34404360992166E-15));
#41738=DIRECTION('',(1.,-5.00596043936352E-16,-3.34404360992166E-15));
#41739=DIRECTION('',(-8.64834036212544E-13,-5.89234658479989E-13,-1.));
#41740=DIRECTION('center_axis',(1.,-5.00596043936352E-16,-3.34404360992166E-15));
#41741=DIRECTION('ref_axis',(-3.34404360992196E-15,-5.89234658479989E-13,
-1.));
#41742=DIRECTION('',(-1.,5.00596043936352E-16,3.34404360992166E-15));
#41743=DIRECTION('center_axis',(0.707106781186791,0.707106781186304,-1.02818183432823E-12));
#41744=DIRECTION('ref_axis',(-0.707106781186304,0.707106781186791,-4.14287226808325E-13));
#41745=DIRECTION('center_axis',(0.707106781186791,0.707106781186304,-1.02818183432823E-12));
#41746=DIRECTION('ref_axis',(-8.64855573465793E-13,-5.89213121226739E-13,
-1.));
#41747=DIRECTION('',(0.707106781186304,-0.707106781186791,4.14287226808325E-13));
#41748=DIRECTION('center_axis',(0.707106781186791,0.707106781186304,-1.02818183432823E-12));
#41749=DIRECTION('ref_axis',(0.707106781186304,-0.707106781186791,4.14287226808325E-13));
#41750=DIRECTION('',(-3.34404360992195E-15,-5.88679546967676E-13,-1.));
#41751=DIRECTION('center_axis',(0.707106781186791,0.707106781186304,-1.02818183432823E-12));
#41752=DIRECTION('ref_axis',(0.707106781186304,-0.707106781186791,4.14287226808325E-13));
#41753=DIRECTION('',(-8.64972814090621E-13,-5.8909588060191E-13,-1.));
#41754=DIRECTION('center_axis',(-0.707106781186791,-0.707106781186304,1.02818183432823E-12));
#41755=DIRECTION('ref_axis',(0.707106781186304,-0.707106781186791,4.14287226808325E-13));
#41756=DIRECTION('',(-0.707106781186304,0.707106781186791,-4.14189096029657E-13));
#41757=DIRECTION('center_axis',(-0.707106781186791,-0.707106781186304,1.02818183432823E-12));
#41758=DIRECTION('ref_axis',(-0.707106781186304,0.707106781186791,-4.14287226808325E-13));
#41759=DIRECTION('center_axis',(5.00596043934382E-16,1.,-5.89095880601911E-13));
#41760=DIRECTION('ref_axis',(1.,-5.00596043936352E-16,-3.34404360992166E-15));
#41761=DIRECTION('',(-1.,5.00596043936352E-16,3.34404360992166E-15));
#41762=DIRECTION('center_axis',(3.34404360992196E-15,5.89234658479989E-13,
1.));
#41763=DIRECTION('ref_axis',(1.,-5.00596043936352E-16,-3.34404360992166E-15));
#41764=DIRECTION('',(-1.,5.00596043936352E-16,3.34404360992166E-15));
#41765=DIRECTION('center_axis',(1.,-5.00596043936352E-16,-3.34404360992166E-15));
#41766=DIRECTION('ref_axis',(-3.34404360992196E-15,-5.89234658479989E-13,
-1.));
#41767=DIRECTION('',(-1.,5.00596043936352E-16,3.34404360992166E-15));
#41768=DIRECTION('center_axis',(3.34404360992196E-15,5.89095880601911E-13,
1.));
#41769=DIRECTION('ref_axis',(1.,-5.00596043936352E-16,-3.34404360992166E-15));
#41770=DIRECTION('',(1.,-5.00596043936352E-16,-3.34404360992166E-15));
#41771=DIRECTION('center_axis',(1.,-5.00596043936352E-16,-3.34404360992166E-15));
#41772=DIRECTION('ref_axis',(-5.00596043934382E-16,-1.,5.89234658479989E-13));
#41773=DIRECTION('center_axis',(1.,-5.00596043936352E-16,-3.34404360992166E-15));
#41774=DIRECTION('ref_axis',(-5.00596043934382E-16,-1.,5.89234658479989E-13));
#41775=DIRECTION('',(-1.,5.00596043936352E-16,3.34404360992166E-15));
#41776=DIRECTION('center_axis',(5.00596043934384E-16,1.,-5.88679546967676E-13));
#41777=DIRECTION('ref_axis',(1.,-5.00596043936352E-16,-3.34404360992166E-15));
#41778=DIRECTION('',(-1.,5.00596043936352E-16,3.34404360992166E-15));
#41779=DIRECTION('center_axis',(1.,-5.00596043936352E-16,-3.34404360992166E-15));
#41780=DIRECTION('ref_axis',(3.34404360992196E-15,5.89234658479989E-13,
1.));
#41781=DIRECTION('center_axis',(-0.707106781186547,-0.707106781186548,1.02850161472388E-12));
#41782=DIRECTION('ref_axis',(3.34404360992239E-15,1.45117688885522E-12,
1.));
#41783=DIRECTION('',(0.707106781186548,-0.707106781186547,1.02377242289756E-12));
#41784=DIRECTION('center_axis',(-0.707106781186547,-0.707106781186548,1.02850161472388E-12));
#41785=DIRECTION('ref_axis',(0.707106781186548,-0.707106781186547,1.02377242289756E-12));
#41786=DIRECTION('',(-2.78893209760981E-15,-1.45173200036753E-12,-1.));
#41787=DIRECTION('center_axis',(-0.707106781186547,-0.707106781186548,1.02850161472388E-12));
#41788=DIRECTION('ref_axis',(0.707106781186548,-0.707106781186547,1.02377242289756E-12));
#41789=DIRECTION('',(-0.707106781186548,0.707106781186547,-1.0236742921189E-12));
#41790=DIRECTION('center_axis',(-0.707106781186547,-0.707106781186548,1.02850161472388E-12));
#41791=DIRECTION('ref_axis',(-0.707106781186548,0.707106781186547,-1.02416494601223E-12));
#41792=DIRECTION('',(-3.34404360992239E-15,-1.45117688885522E-12,-1.));
#41793=DIRECTION('center_axis',(-0.707106781186547,-0.707106781186548,1.02850161472388E-12));
#41794=DIRECTION('ref_axis',(-0.707106781186548,0.707106781186547,-1.02377242289756E-12));
#41795=DIRECTION('',(3.20526573184424E-15,1.4513156667333E-12,1.));
#41796=DIRECTION('center_axis',(0.707106781186547,0.707106781186548,-1.02850161472388E-12));
#41797=DIRECTION('ref_axis',(0.707106781186548,-0.707106781186547,1.02377242289756E-12));
#41798=DIRECTION('',(-0.707106781186548,0.707106781186547,-1.02387055367623E-12));
#41799=DIRECTION('center_axis',(0.707106781186547,0.707106781186548,-1.02850161472388E-12));
#41800=DIRECTION('ref_axis',(-0.707106781186548,0.707106781186547,-1.02377242289756E-12));
#41801=DIRECTION('',(-2.99709891472702E-15,-1.45152383355042E-12,-1.));
#41802=DIRECTION('center_axis',(0.707106781186547,0.707106781186548,-1.02850161472388E-12));
#41803=DIRECTION('ref_axis',(-0.707106781186548,0.707106781186547,-1.02377242289756E-12));
#41804=DIRECTION('',(0.707106781186548,-0.707106781186547,1.02387055367623E-12));
#41805=DIRECTION('center_axis',(0.707106781186547,0.707106781186548,-1.02850161472388E-12));
#41806=DIRECTION('ref_axis',(0.707106781186548,-0.707106781186547,1.02377242289756E-12));
#41807=DIRECTION('center_axis',(-5.00596043931498E-16,-1.,1.45152383355042E-12));
#41808=DIRECTION('ref_axis',(1.,-5.00596043936352E-16,-3.34404360992166E-15));
#41809=DIRECTION('',(-1.,5.00596043936352E-16,3.34404360992166E-15));
#41810=DIRECTION('',(3.69098830511775E-15,1.45152383355042E-12,1.));
#41811=DIRECTION('',(-1.,5.00596043936352E-16,3.34404360992166E-15));
#41812=DIRECTION('center_axis',(-1.,5.00596043936352E-16,3.34404360992166E-15));
#41813=DIRECTION('ref_axis',(3.34404360992239E-15,1.45117688885522E-12,
1.));
#41814=DIRECTION('',(-1.,5.00596043936352E-16,3.34404360992166E-15));
#41815=DIRECTION('center_axis',(-0.707106781186547,0.707106781186548,-1.02377242289756E-12));
#41816=DIRECTION('ref_axis',(0.707106781186548,0.707106781186547,-1.02850161472388E-12));
#41817=DIRECTION('center_axis',(-3.34404360992239E-15,-1.4513156667333E-12,
-1.));
#41818=DIRECTION('ref_axis',(-1.,5.00596043936352E-16,3.34404360992166E-15));
#41819=DIRECTION('',(-1.,5.00596043936352E-16,3.34404360992166E-15));
#41820=DIRECTION('',(-0.707106781186548,-0.707106781186547,1.02859974550255E-12));
#41821=DIRECTION('center_axis',(-1.,5.00596043936352E-16,3.34404360992166E-15));
#41822=DIRECTION('ref_axis',(-5.00596043931499E-16,-1.,1.45117688885522E-12));
#41823=DIRECTION('',(-1.,5.00596043936352E-16,3.34404360992166E-15));
#41824=DIRECTION('center_axis',(-0.707106781186547,0.707106781186548,-1.02377242289756E-12));
#41825=DIRECTION('ref_axis',(-0.707106781186548,-0.707106781186547,1.02850161472388E-12));
#41826=DIRECTION('center_axis',(3.34404360992239E-15,1.45103811097714E-12,
1.));
#41827=DIRECTION('ref_axis',(1.,-5.00596043936352E-16,-3.34404360992166E-15));
#41828=DIRECTION('',(-1.,5.00596043936352E-16,3.34404360992166E-15));
#41829=DIRECTION('',(-0.707106781186548,-0.707106781186547,1.02840348394521E-12));
#41830=DIRECTION('',(-1.,5.00596043936352E-16,3.34404360992166E-15));
#41831=DIRECTION('center_axis',(-1.,5.00596043936352E-16,3.34404360992166E-15));
#41832=DIRECTION('ref_axis',(-3.34404360992239E-15,-1.45117688885522E-12,
-1.));
#41833=DIRECTION('',(-1.,5.00596043936352E-16,3.34404360992166E-15));
#41834=DIRECTION('center_axis',(0.707106781186547,-0.707106781186548,1.02377242289756E-12));
#41835=DIRECTION('ref_axis',(-0.707106781186548,-0.707106781186547,1.02850161472388E-12));
#41836=DIRECTION('center_axis',(5.00596043931497E-16,1.,-1.45173200036753E-12));
#41837=DIRECTION('ref_axis',(-1.,5.00596043936352E-16,3.34404360992166E-15));
#41838=DIRECTION('',(-1.,5.00596043936352E-16,3.34404360992166E-15));
#41839=DIRECTION('',(3.89915512223497E-15,1.45173200036753E-12,1.));
#41840=DIRECTION('center_axis',(-1.,5.00596043936352E-16,3.34404360992166E-15));
#41841=DIRECTION('ref_axis',(-5.00596043931499E-16,-1.,1.45117688885522E-12));
#41842=DIRECTION('',(-1.,5.00596043936352E-16,3.34404360992166E-15));
#41843=DIRECTION('center_axis',(0.707106781186547,-0.707106781186548,1.02377242289756E-12));
#41844=DIRECTION('ref_axis',(-0.707106781186548,-0.707106781186547,1.02850161472388E-12));
#41845=DIRECTION('center_axis',(0.707106781186547,-0.707106781186548,1.02377242289756E-12));
#41846=DIRECTION('ref_axis',(-3.34404360992239E-15,-1.45117688885522E-12,
-1.));
#41847=DIRECTION('',(0.707106781186548,0.707106781186547,-1.02850161472388E-12));
#41848=DIRECTION('center_axis',(0.707106781186547,-0.707106781186548,1.02377242289756E-12));
#41849=DIRECTION('ref_axis',(0.707106781186548,0.707106781186547,-1.02850161472388E-12));
#41850=DIRECTION('',(-3.34404360992239E-15,-1.45117688885522E-12,-1.));
#41851=DIRECTION('center_axis',(0.707106781186547,-0.707106781186548,1.02377242289756E-12));
#41852=DIRECTION('ref_axis',(0.707106781186548,0.707106781186547,-1.02889413783855E-12));
#41853=DIRECTION('',(-3.48282148800053E-15,-1.4513156667333E-12,-1.));
#41854=DIRECTION('center_axis',(-0.707106781186547,0.707106781186548,-1.02377242289756E-12));
#41855=DIRECTION('ref_axis',(-0.707106781186548,-0.707106781186547,1.02850161472388E-12));
#41856=DIRECTION('',(0.707106781186548,0.707106781186547,-1.02859974550255E-12));
#41857=DIRECTION('center_axis',(-0.707106781186547,0.707106781186548,-1.02377242289756E-12));
#41858=DIRECTION('ref_axis',(0.707106781186548,0.707106781186547,-1.02850161472388E-12));
#41859=DIRECTION('center_axis',(5.00596043931499E-16,1.,-1.4513156667333E-12));
#41860=DIRECTION('ref_axis',(-1.,5.00596043936352E-16,3.34404360992166E-15));
#41861=DIRECTION('',(-1.,5.00596043936352E-16,3.34404360992166E-15));
#41862=DIRECTION('center_axis',(-3.34404360992239E-15,-1.45117688885522E-12,
-1.));
#41863=DIRECTION('ref_axis',(-1.,5.00596043936352E-16,3.34404360992166E-15));
#41864=DIRECTION('',(-1.,5.00596043936352E-16,3.34404360992166E-15));
#41865=DIRECTION('center_axis',(-1.,5.00596043936352E-16,3.34404360992166E-15));
#41866=DIRECTION('ref_axis',(5.00596043931499E-16,1.,-1.45117688885522E-12));
#41867=DIRECTION('',(-1.,5.00596043936352E-16,3.34404360992166E-15));
#41868=DIRECTION('center_axis',(3.34404360992239E-15,1.4513156667333E-12,
1.));
#41869=DIRECTION('ref_axis',(1.,-5.00596043936352E-16,-3.34404360992166E-15));
#41870=DIRECTION('',(-1.,5.00596043936352E-16,3.34404360992166E-15));
#41871=DIRECTION('center_axis',(-1.,5.00596043936352E-16,3.34404360992166E-15));
#41872=DIRECTION('ref_axis',(-3.34404360992239E-15,-1.45117688885522E-12,
-1.));
#41873=DIRECTION('center_axis',(-1.,5.00596043936352E-16,3.34404360992166E-15));
#41874=DIRECTION('ref_axis',(5.00596043931497E-16,1.,-1.45173200036753E-12));
#41875=DIRECTION('',(-1.,5.00596043936352E-16,3.34404360992166E-15));
#41876=DIRECTION('center_axis',(-5.00596043931499E-16,-1.,1.45117688885522E-12));
#41877=DIRECTION('ref_axis',(1.,-5.00596043936352E-16,-3.34404360992166E-15));
#41878=DIRECTION('',(-1.,5.00596043936352E-16,3.34404360992166E-15));
#41879=DIRECTION('center_axis',(-1.,5.00596043936352E-16,3.34404360992166E-15));
#41880=DIRECTION('ref_axis',(3.34404360992239E-15,1.45117688885522E-12,
1.));
#41881=DIRECTION('center_axis',(-5.00596043934463E-16,-1.,-1.46803972383759E-15));
#41882=DIRECTION('ref_axis',(-1.,5.00596043934458E-16,3.60315789384389E-15));
#41883=DIRECTION('',(-3.60315789384389E-15,1.46803972383759E-15,-1.));
#41884=DIRECTION('',(1.,-5.00596043934458E-16,-3.60315789384389E-15));
#41885=DIRECTION('',(-3.60315789384389E-15,1.46803972383759E-15,-1.));
#41886=DIRECTION('',(1.,-5.00596043934458E-16,-3.60315789384389E-15));
#41887=DIRECTION('center_axis',(1.,-5.00596043934458E-16,-3.60315789384389E-15));
#41888=DIRECTION('ref_axis',(5.00596043934462E-16,1.,1.12109502864223E-15));
#41889=DIRECTION('center_axis',(1.,-5.00596043934458E-16,-3.60315789384389E-15));
#41890=DIRECTION('ref_axis',(5.00596043934462E-16,1.,1.12109502864223E-15));
#41891=DIRECTION('',(1.,-5.00596043934458E-16,-3.60315789384389E-15));
#41892=DIRECTION('center_axis',(1.,-5.00596043934458E-16,-3.60315789384389E-15));
#41893=DIRECTION('ref_axis',(5.00596043934462E-16,1.,1.12109502864223E-15));
#41894=DIRECTION('center_axis',(-3.60315789384389E-15,1.25987290672038E-15,
-1.));
#41895=DIRECTION('ref_axis',(-1.,5.00596043934458E-16,3.60315789384389E-15));
#41896=DIRECTION('',(5.00596043934463E-16,1.,1.25987290672037E-15));
#41897=DIRECTION('',(1.,-5.00596043934458E-16,-3.60315789384389E-15));
#41898=DIRECTION('',(5.00596043934463E-16,1.,1.25987290672037E-15));
#41899=DIRECTION('center_axis',(1.,-5.00596043934458E-16,-3.60315789384389E-15));
#41900=DIRECTION('ref_axis',(3.60315789384389E-15,-1.12109502864223E-15,
1.));
#41901=DIRECTION('center_axis',(1.,-5.00596043934458E-16,-3.60315789384389E-15));
#41902=DIRECTION('ref_axis',(3.60315789384389E-15,-1.12109502864223E-15,
1.));
#41903=DIRECTION('',(1.,-5.00596043934458E-16,-3.60315789384389E-15));
#41904=DIRECTION('center_axis',(1.,-5.00596043934458E-16,-3.60315789384389E-15));
#41905=DIRECTION('ref_axis',(3.60315789384389E-15,-1.12109502864223E-15,
1.));
#41906=DIRECTION('center_axis',(-3.60315789384389E-15,9.82317150564085E-16,
-1.));
#41907=DIRECTION('ref_axis',(-1.,5.00596043934458E-16,3.60315789384389E-15));
#41908=DIRECTION('',(-5.00596043934462E-16,-1.,-9.82317150564083E-16));
#41909=DIRECTION('',(1.,-5.00596043934458E-16,-3.60315789384389E-15));
#41910=DIRECTION('',(-5.00596043934462E-16,-1.,-9.82317150564083E-16));
#41911=DIRECTION('',(1.,-5.00596043934458E-16,-3.60315789384389E-15));
#41912=DIRECTION('center_axis',(1.,-5.00596043934458E-16,-3.60315789384389E-15));
#41913=DIRECTION('ref_axis',(5.00596043934464E-16,1.,1.67620654095481E-15));
#41914=DIRECTION('center_axis',(-1.,5.00596043934458E-16,3.60315789384389E-15));
#41915=DIRECTION('ref_axis',(5.00596043934464E-16,1.,1.67620654095481E-15));
#41916=DIRECTION('',(1.,-5.00596043934458E-16,-3.60315789384389E-15));
#41917=DIRECTION('center_axis',(-1.,5.00596043934458E-16,3.60315789384389E-15));
#41918=DIRECTION('ref_axis',(5.00596043934464E-16,1.,1.67620654095481E-15));
#41919=DIRECTION('center_axis',(-5.00596043934462E-16,-1.,-1.12109502864223E-15));
#41920=DIRECTION('ref_axis',(-1.,5.00596043934458E-16,3.60315789384389E-15));
#41921=DIRECTION('',(3.60315789384389E-15,-1.12109502864223E-15,1.));
#41922=DIRECTION('',(1.,-5.00596043934458E-16,-3.60315789384389E-15));
#41923=DIRECTION('',(3.60315789384389E-15,-1.12109502864223E-15,1.));
#41924=DIRECTION('center_axis',(1.,-5.00596043934458E-16,-3.60315789384389E-15));
#41925=DIRECTION('ref_axis',(-3.60315789384389E-15,1.12109502864223E-15,
-1.));
#41926=DIRECTION('center_axis',(-1.,5.00596043934458E-16,3.60315789384389E-15));
#41927=DIRECTION('ref_axis',(-3.60315789384389E-15,1.12109502864223E-15,
-1.));
#41928=DIRECTION('',(1.,-5.00596043934458E-16,-3.60315789384389E-15));
#41929=DIRECTION('center_axis',(-1.,5.00596043934458E-16,3.60315789384389E-15));
#41930=DIRECTION('ref_axis',(-3.60315789384389E-15,1.12109502864223E-15,
-1.));
#41931=DIRECTION('center_axis',(5.00596043934463E-16,1.,1.25987290672037E-15));
#41932=DIRECTION('ref_axis',(1.,-5.00596043934458E-16,-3.60315789384389E-15));
#41933=DIRECTION('',(3.60315789384389E-15,-1.25987290672038E-15,1.));
#41934=DIRECTION('',(1.,-5.00596043934458E-16,-3.60315789384389E-15));
#41935=DIRECTION('',(3.60315789384389E-15,-1.25987290672038E-15,1.));
#41936=DIRECTION('center_axis',(1.,-5.00596043934458E-16,-3.60315789384389E-15));
#41937=DIRECTION('ref_axis',(-3.60315789384389E-15,1.12109502864223E-15,
-1.));
#41938=DIRECTION('center_axis',(1.,-5.00596043934458E-16,-3.60315789384389E-15));
#41939=DIRECTION('ref_axis',(-3.60315789384389E-15,1.12109502864223E-15,
-1.));
#41940=DIRECTION('center_axis',(1.,-5.00596043934458E-16,-3.60315789384389E-15));
#41941=DIRECTION('ref_axis',(-3.60315789384389E-15,1.12109502864223E-15,
-1.));
#41942=DIRECTION('',(1.,-5.00596043934458E-16,-3.60315789384389E-15));
#41943=DIRECTION('center_axis',(3.60315789384389E-15,-1.25987290672038E-15,
1.));
#41944=DIRECTION('ref_axis',(1.,-5.00596043934458E-16,-3.60315789384389E-15));
#41945=DIRECTION('',(-5.00596043934463E-16,-1.,-1.25987290672037E-15));
#41946=DIRECTION('',(-5.00596043934463E-16,-1.,-1.25987290672037E-15));
#41947=DIRECTION('',(1.,-5.00596043934458E-16,-3.60315789384389E-15));
#41948=DIRECTION('center_axis',(1.,-5.00596043934458E-16,-3.60315789384389E-15));
#41949=DIRECTION('ref_axis',(-5.00596043934462E-16,-1.,-1.12109502864223E-15));
#41950=DIRECTION('center_axis',(1.,-5.00596043934458E-16,-3.60315789384389E-15));
#41951=DIRECTION('ref_axis',(-5.00596043934462E-16,-1.,-1.12109502864223E-15));
#41952=DIRECTION('center_axis',(1.,-5.00596043934458E-16,-3.60315789384389E-15));
#41953=DIRECTION('ref_axis',(-5.00596043934462E-16,-1.,-1.12109502864223E-15));
#41954=DIRECTION('center_axis',(3.60315789384389E-15,-1.12109502864223E-15,
1.));
#41955=DIRECTION('ref_axis',(1.,-5.00596043934458E-16,-3.60315789384389E-15));
#41956=DIRECTION('',(5.00596043934462E-16,1.,1.12109502864223E-15));
#41957=DIRECTION('',(1.,-5.00596043934458E-16,-3.60315789384389E-15));
#41958=DIRECTION('',(5.00596043934462E-16,1.,1.12109502864223E-15));
#41959=DIRECTION('center_axis',(1.,-5.00596043934458E-16,-3.60315789384389E-15));
#41960=DIRECTION('ref_axis',(-5.00596043934462E-16,-1.,-1.12109502864223E-15));
#41961=DIRECTION('center_axis',(-1.,5.00596043934458E-16,3.60315789384389E-15));
#41962=DIRECTION('ref_axis',(-5.00596043934462E-16,-1.,-1.12109502864223E-15));
#41963=DIRECTION('',(1.,-5.00596043934458E-16,-3.60315789384389E-15));
#41964=DIRECTION('center_axis',(-1.,5.00596043934458E-16,3.60315789384389E-15));
#41965=DIRECTION('ref_axis',(-5.00596043934462E-16,-1.,-1.12109502864223E-15));
#41966=DIRECTION('center_axis',(5.00596043934464E-16,1.,1.67620654095481E-15));
#41967=DIRECTION('ref_axis',(1.,-5.00596043934458E-16,-3.60315789384389E-15));
#41968=DIRECTION('',(-3.60315789384389E-15,1.67620654095481E-15,-1.));
#41969=DIRECTION('',(1.,-5.00596043934458E-16,-3.60315789384389E-15));
#41970=DIRECTION('',(-3.60315789384389E-15,1.67620654095481E-15,-1.));
#41971=DIRECTION('center_axis',(1.,-5.00596043934458E-16,-3.60315789384389E-15));
#41972=DIRECTION('ref_axis',(3.60315789384389E-15,-1.12109502864223E-15,
1.));
#41973=DIRECTION('center_axis',(-1.,5.00596043934458E-16,3.60315789384389E-15));
#41974=DIRECTION('ref_axis',(3.60315789384389E-15,-1.12109502864223E-15,
1.));
#41975=DIRECTION('center_axis',(-1.,5.00596043934458E-16,3.60315789384389E-15));
#41976=DIRECTION('ref_axis',(3.60315789384389E-15,-1.12109502864223E-15,
1.));
#41977=DIRECTION('center_axis',(1.,-5.00596043934458E-16,-3.60315789384389E-15));
#41978=DIRECTION('ref_axis',(-3.60315789384389E-15,1.12109502864223E-15,
-1.));
#41979=DIRECTION('center_axis',(1.,-5.00596043934458E-16,-3.60315789384389E-15));
#41980=DIRECTION('ref_axis',(-3.60315789384389E-15,1.12109502864223E-15,
-1.));
#41981=DIRECTION('center_axis',(-5.00596043934463E-16,-1.,-1.46803972383759E-15));
#41982=DIRECTION('ref_axis',(-1.,5.00596043934458E-16,3.60315789384389E-15));
#41983=DIRECTION('',(-3.60315789384389E-15,1.46803972383759E-15,-1.));
#41984=DIRECTION('',(1.,-5.00596043934458E-16,-3.60315789384389E-15));
#41985=DIRECTION('',(-3.60315789384389E-15,1.46803972383759E-15,-1.));
#41986=DIRECTION('',(1.,-5.00596043934458E-16,-3.60315789384389E-15));
#41987=DIRECTION('center_axis',(1.,-5.00596043934458E-16,-3.60315789384389E-15));
#41988=DIRECTION('ref_axis',(5.00596043934462E-16,1.,1.12109502864223E-15));
#41989=DIRECTION('center_axis',(1.,-5.00596043934458E-16,-3.60315789384389E-15));
#41990=DIRECTION('ref_axis',(5.00596043934462E-16,1.,1.12109502864223E-15));
#41991=DIRECTION('',(1.,-5.00596043934458E-16,-3.60315789384389E-15));
#41992=DIRECTION('center_axis',(1.,-5.00596043934458E-16,-3.60315789384389E-15));
#41993=DIRECTION('ref_axis',(5.00596043934462E-16,1.,1.12109502864223E-15));
#41994=DIRECTION('center_axis',(-3.60315789384389E-15,1.25987290672038E-15,
-1.));
#41995=DIRECTION('ref_axis',(-1.,5.00596043934458E-16,3.60315789384389E-15));
#41996=DIRECTION('',(5.00596043934463E-16,1.,1.25987290672037E-15));
#41997=DIRECTION('',(1.,-5.00596043934458E-16,-3.60315789384389E-15));
#41998=DIRECTION('',(5.00596043934463E-16,1.,1.25987290672037E-15));
#41999=DIRECTION('center_axis',(1.,-5.00596043934458E-16,-3.60315789384389E-15));
#42000=DIRECTION('ref_axis',(3.60315789384389E-15,-1.12109502864223E-15,
1.));
#42001=DIRECTION('center_axis',(1.,-5.00596043934458E-16,-3.60315789384389E-15));
#42002=DIRECTION('ref_axis',(3.60315789384389E-15,-1.12109502864223E-15,
1.));
#42003=DIRECTION('',(1.,-5.00596043934458E-16,-3.60315789384389E-15));
#42004=DIRECTION('center_axis',(1.,-5.00596043934458E-16,-3.60315789384389E-15));
#42005=DIRECTION('ref_axis',(3.60315789384389E-15,-1.12109502864223E-15,
1.));
#42006=DIRECTION('center_axis',(-3.60315789384389E-15,9.82317150564085E-16,
-1.));
#42007=DIRECTION('ref_axis',(-1.,5.00596043934458E-16,3.60315789384389E-15));
#42008=DIRECTION('',(-5.00596043934462E-16,-1.,-9.82317150564083E-16));
#42009=DIRECTION('',(1.,-5.00596043934458E-16,-3.60315789384389E-15));
#42010=DIRECTION('',(-5.00596043934462E-16,-1.,-9.82317150564083E-16));
#42011=DIRECTION('',(1.,-5.00596043934458E-16,-3.60315789384389E-15));
#42012=DIRECTION('center_axis',(1.,-5.00596043934458E-16,-3.60315789384389E-15));
#42013=DIRECTION('ref_axis',(5.00596043934464E-16,1.,1.67620654095481E-15));
#42014=DIRECTION('center_axis',(-1.,5.00596043934458E-16,3.60315789384389E-15));
#42015=DIRECTION('ref_axis',(5.00596043934464E-16,1.,1.67620654095481E-15));
#42016=DIRECTION('',(1.,-5.00596043934458E-16,-3.60315789384389E-15));
#42017=DIRECTION('center_axis',(-1.,5.00596043934458E-16,3.60315789384389E-15));
#42018=DIRECTION('ref_axis',(5.00596043934464E-16,1.,1.67620654095481E-15));
#42019=DIRECTION('center_axis',(-5.00596043934462E-16,-1.,-1.12109502864223E-15));
#42020=DIRECTION('ref_axis',(-1.,5.00596043934458E-16,3.60315789384389E-15));
#42021=DIRECTION('',(3.60315789384389E-15,-1.12109502864223E-15,1.));
#42022=DIRECTION('',(1.,-5.00596043934458E-16,-3.60315789384389E-15));
#42023=DIRECTION('',(3.60315789384389E-15,-1.12109502864223E-15,1.));
#42024=DIRECTION('center_axis',(1.,-5.00596043934458E-16,-3.60315789384389E-15));
#42025=DIRECTION('ref_axis',(-3.60315789384389E-15,1.12109502864223E-15,
-1.));
#42026=DIRECTION('center_axis',(-1.,5.00596043934458E-16,3.60315789384389E-15));
#42027=DIRECTION('ref_axis',(-3.60315789384389E-15,1.12109502864223E-15,
-1.));
#42028=DIRECTION('',(1.,-5.00596043934458E-16,-3.60315789384389E-15));
#42029=DIRECTION('center_axis',(-1.,5.00596043934458E-16,3.60315789384389E-15));
#42030=DIRECTION('ref_axis',(-3.60315789384389E-15,1.12109502864223E-15,
-1.));
#42031=DIRECTION('center_axis',(5.00596043934463E-16,1.,1.25987290672037E-15));
#42032=DIRECTION('ref_axis',(1.,-5.00596043934458E-16,-3.60315789384389E-15));
#42033=DIRECTION('',(3.60315789384389E-15,-1.25987290672038E-15,1.));
#42034=DIRECTION('',(1.,-5.00596043934458E-16,-3.60315789384389E-15));
#42035=DIRECTION('',(3.60315789384389E-15,-1.25987290672038E-15,1.));
#42036=DIRECTION('center_axis',(1.,-5.00596043934458E-16,-3.60315789384389E-15));
#42037=DIRECTION('ref_axis',(-3.60315789384389E-15,1.12109502864223E-15,
-1.));
#42038=DIRECTION('center_axis',(1.,-5.00596043934458E-16,-3.60315789384389E-15));
#42039=DIRECTION('ref_axis',(-3.60315789384389E-15,1.12109502864223E-15,
-1.));
#42040=DIRECTION('center_axis',(1.,-5.00596043934458E-16,-3.60315789384389E-15));
#42041=DIRECTION('ref_axis',(-3.60315789384389E-15,1.12109502864223E-15,
-1.));
#42042=DIRECTION('',(1.,-5.00596043934458E-16,-3.60315789384389E-15));
#42043=DIRECTION('center_axis',(3.60315789384389E-15,-1.25987290672038E-15,
1.));
#42044=DIRECTION('ref_axis',(1.,-5.00596043934458E-16,-3.60315789384389E-15));
#42045=DIRECTION('',(-5.00596043934463E-16,-1.,-1.25987290672037E-15));
#42046=DIRECTION('',(-5.00596043934463E-16,-1.,-1.25987290672037E-15));
#42047=DIRECTION('',(1.,-5.00596043934458E-16,-3.60315789384389E-15));
#42048=DIRECTION('center_axis',(1.,-5.00596043934458E-16,-3.60315789384389E-15));
#42049=DIRECTION('ref_axis',(-5.00596043934462E-16,-1.,-1.12109502864223E-15));
#42050=DIRECTION('center_axis',(1.,-5.00596043934458E-16,-3.60315789384389E-15));
#42051=DIRECTION('ref_axis',(-5.00596043934462E-16,-1.,-1.12109502864223E-15));
#42052=DIRECTION('center_axis',(1.,-5.00596043934458E-16,-3.60315789384389E-15));
#42053=DIRECTION('ref_axis',(-5.00596043934462E-16,-1.,-1.12109502864223E-15));
#42054=DIRECTION('center_axis',(3.60315789384389E-15,-1.12109502864223E-15,
1.));
#42055=DIRECTION('ref_axis',(1.,-5.00596043934458E-16,-3.60315789384389E-15));
#42056=DIRECTION('',(5.00596043934462E-16,1.,1.12109502864223E-15));
#42057=DIRECTION('',(1.,-5.00596043934458E-16,-3.60315789384389E-15));
#42058=DIRECTION('',(5.00596043934462E-16,1.,1.12109502864223E-15));
#42059=DIRECTION('center_axis',(1.,-5.00596043934458E-16,-3.60315789384389E-15));
#42060=DIRECTION('ref_axis',(-5.00596043934462E-16,-1.,-1.12109502864223E-15));
#42061=DIRECTION('center_axis',(-1.,5.00596043934458E-16,3.60315789384389E-15));
#42062=DIRECTION('ref_axis',(-5.00596043934462E-16,-1.,-1.12109502864223E-15));
#42063=DIRECTION('',(1.,-5.00596043934458E-16,-3.60315789384389E-15));
#42064=DIRECTION('center_axis',(-1.,5.00596043934458E-16,3.60315789384389E-15));
#42065=DIRECTION('ref_axis',(-5.00596043934462E-16,-1.,-1.12109502864223E-15));
#42066=DIRECTION('center_axis',(5.00596043934464E-16,1.,1.67620654095481E-15));
#42067=DIRECTION('ref_axis',(1.,-5.00596043934458E-16,-3.60315789384389E-15));
#42068=DIRECTION('',(-3.60315789384389E-15,1.67620654095481E-15,-1.));
#42069=DIRECTION('',(1.,-5.00596043934458E-16,-3.60315789384389E-15));
#42070=DIRECTION('',(-3.60315789384389E-15,1.67620654095481E-15,-1.));
#42071=DIRECTION('center_axis',(1.,-5.00596043934458E-16,-3.60315789384389E-15));
#42072=DIRECTION('ref_axis',(3.60315789384389E-15,-1.12109502864223E-15,
1.));
#42073=DIRECTION('center_axis',(-1.,5.00596043934458E-16,3.60315789384389E-15));
#42074=DIRECTION('ref_axis',(3.60315789384389E-15,-1.12109502864223E-15,
1.));
#42075=DIRECTION('center_axis',(-1.,5.00596043934458E-16,3.60315789384389E-15));
#42076=DIRECTION('ref_axis',(3.60315789384389E-15,-1.12109502864223E-15,
1.));
#42077=DIRECTION('center_axis',(1.,-5.00596043934458E-16,-3.60315789384389E-15));
#42078=DIRECTION('ref_axis',(-3.60315789384389E-15,1.12109502864223E-15,
-1.));
#42079=DIRECTION('center_axis',(1.,-5.00596043934458E-16,-3.60315789384389E-15));
#42080=DIRECTION('ref_axis',(-3.60315789384389E-15,1.12109502864223E-15,
-1.));
#42081=DIRECTION('center_axis',(3.25621319864853E-15,-1.12109502864222E-15,
1.));
#42082=DIRECTION('ref_axis',(4.72840468318833E-16,1.,1.12109502864222E-15));
#42083=DIRECTION('',(-1.,4.72840468318829E-16,3.25621319864853E-15));
#42084=DIRECTION('',(-4.72840468318833E-16,-1.,-1.12109502864222E-15));
#42085=DIRECTION('',(-1.,4.72840468318829E-16,3.25621319864853E-15));
#42086=DIRECTION('',(-4.72840468318833E-16,-1.,-1.12109502864222E-15));
#42087=DIRECTION('center_axis',(-4.72840468318833E-16,-1.,-1.12109502864222E-15));
#42088=DIRECTION('ref_axis',(-3.60315789384389E-15,1.12109502864222E-15,
-1.));
#42089=DIRECTION('center_axis',(-4.72840468318833E-16,-1.,-1.12109502864222E-15));
#42090=DIRECTION('ref_axis',(-3.60315789384389E-15,1.12109502864222E-15,
-1.));
#42091=DIRECTION('',(-4.72840468318833E-16,-1.,-1.12109502864222E-15));
#42092=DIRECTION('center_axis',(-4.72840468318833E-16,-1.,-1.12109502864222E-15));
#42093=DIRECTION('ref_axis',(-3.60315789384389E-15,1.12109502864222E-15,
-1.));
#42094=DIRECTION('center_axis',(-1.,4.72840468318829E-16,3.46438001576575E-15));
#42095=DIRECTION('ref_axis',(4.72840468318833E-16,1.,1.12109502864222E-15));
#42096=DIRECTION('',(-3.46438001576574E-15,1.12109502864222E-15,-1.));
#42097=DIRECTION('',(-4.72840468318833E-16,-1.,-1.12109502864222E-15));
#42098=DIRECTION('',(-3.46438001576574E-15,1.12109502864222E-15,-1.));
#42099=DIRECTION('center_axis',(-4.72840468318833E-16,-1.,-1.12109502864222E-15));
#42100=DIRECTION('ref_axis',(1.,-4.72840468318829E-16,-3.60315789384389E-15));
#42101=DIRECTION('center_axis',(-4.72840468318833E-16,-1.,-1.12109502864222E-15));
#42102=DIRECTION('ref_axis',(1.,-4.72840468318829E-16,-3.60315789384389E-15));
#42103=DIRECTION('',(-4.72840468318833E-16,-1.,-1.12109502864222E-15));
#42104=DIRECTION('center_axis',(-4.72840468318833E-16,-1.,-1.12109502864222E-15));
#42105=DIRECTION('ref_axis',(1.,-4.72840468318829E-16,-3.60315789384389E-15));
#42106=DIRECTION('center_axis',(-1.,4.72840468318829E-16,3.74193577192204E-15));
#42107=DIRECTION('ref_axis',(4.72840468318833E-16,1.,1.12109502864222E-15));
#42108=DIRECTION('',(3.74193577192203E-15,-1.12109502864222E-15,1.));
#42109=DIRECTION('',(-4.72840468318833E-16,-1.,-1.12109502864222E-15));
#42110=DIRECTION('',(3.74193577192203E-15,-1.12109502864222E-15,1.));
#42111=DIRECTION('',(-4.72840468318833E-16,-1.,-1.12109502864222E-15));
#42112=DIRECTION('center_axis',(-4.72840468318833E-16,-1.,-1.12109502864222E-15));
#42113=DIRECTION('ref_axis',(-3.04804638153131E-15,1.12109502864222E-15,
-1.));
#42114=DIRECTION('center_axis',(4.72840468318833E-16,1.,1.12109502864222E-15));
#42115=DIRECTION('ref_axis',(-3.04804638153131E-15,1.12109502864222E-15,
-1.));
#42116=DIRECTION('',(-4.72840468318833E-16,-1.,-1.12109502864222E-15));
#42117=DIRECTION('center_axis',(4.72840468318833E-16,1.,1.12109502864222E-15));
#42118=DIRECTION('ref_axis',(-3.04804638153131E-15,1.12109502864222E-15,
-1.));
#42119=DIRECTION('center_axis',(3.60315789384389E-15,-1.12109502864222E-15,
1.));
#42120=DIRECTION('ref_axis',(4.72840468318833E-16,1.,1.12109502864222E-15));
#42121=DIRECTION('',(1.,-4.72840468318829E-16,-3.60315789384389E-15));
#42122=DIRECTION('',(-4.72840468318833E-16,-1.,-1.12109502864222E-15));
#42123=DIRECTION('',(1.,-4.72840468318829E-16,-3.60315789384389E-15));
#42124=DIRECTION('center_axis',(-4.72840468318833E-16,-1.,-1.12109502864222E-15));
#42125=DIRECTION('ref_axis',(-1.,4.72840468318829E-16,3.60315789384389E-15));
#42126=DIRECTION('center_axis',(4.72840468318833E-16,1.,1.12109502864222E-15));
#42127=DIRECTION('ref_axis',(-1.,4.72840468318829E-16,3.60315789384389E-15));
#42128=DIRECTION('',(-4.72840468318833E-16,-1.,-1.12109502864222E-15));
#42129=DIRECTION('center_axis',(4.72840468318833E-16,1.,1.12109502864222E-15));
#42130=DIRECTION('ref_axis',(-1.,4.72840468318829E-16,3.60315789384389E-15));
#42131=DIRECTION('center_axis',(-3.46438001576574E-15,1.12109502864222E-15,
-1.));
#42132=DIRECTION('ref_axis',(-4.72840468318833E-16,-1.,-1.12109502864222E-15));
#42133=DIRECTION('',(1.,-4.72840468318829E-16,-3.46438001576575E-15));
#42134=DIRECTION('',(-4.72840468318833E-16,-1.,-1.12109502864222E-15));
#42135=DIRECTION('',(1.,-4.72840468318829E-16,-3.46438001576575E-15));
#42136=DIRECTION('center_axis',(-4.72840468318833E-16,-1.,-1.12109502864222E-15));
#42137=DIRECTION('ref_axis',(-1.,4.72840468318829E-16,3.60315789384389E-15));
#42138=DIRECTION('center_axis',(-4.72840468318833E-16,-1.,-1.12109502864222E-15));
#42139=DIRECTION('ref_axis',(-1.,4.72840468318829E-16,3.60315789384389E-15));
#42140=DIRECTION('center_axis',(-4.72840468318833E-16,-1.,-1.12109502864222E-15));
#42141=DIRECTION('ref_axis',(-1.,4.72840468318829E-16,3.60315789384389E-15));
#42142=DIRECTION('',(-4.72840468318833E-16,-1.,-1.12109502864222E-15));
#42143=DIRECTION('center_axis',(1.,-4.72840468318829E-16,-3.46438001576575E-15));
#42144=DIRECTION('ref_axis',(-4.72840468318833E-16,-1.,-1.12109502864222E-15));
#42145=DIRECTION('',(3.46438001576574E-15,-1.12109502864222E-15,1.));
#42146=DIRECTION('',(3.46438001576574E-15,-1.12109502864222E-15,1.));
#42147=DIRECTION('',(-4.72840468318833E-16,-1.,-1.12109502864222E-15));
#42148=DIRECTION('center_axis',(-4.72840468318833E-16,-1.,-1.12109502864222E-15));
#42149=DIRECTION('ref_axis',(3.60315789384389E-15,-1.12109502864222E-15,
1.));
#42150=DIRECTION('center_axis',(-4.72840468318833E-16,-1.,-1.12109502864222E-15));
#42151=DIRECTION('ref_axis',(3.60315789384389E-15,-1.12109502864222E-15,
1.));
#42152=DIRECTION('center_axis',(-4.72840468318833E-16,-1.,-1.12109502864222E-15));
#42153=DIRECTION('ref_axis',(3.60315789384389E-15,-1.12109502864222E-15,
1.));
#42154=DIRECTION('center_axis',(1.,-4.72840468318829E-16,-3.60315789384389E-15));
#42155=DIRECTION('ref_axis',(-4.72840468318833E-16,-1.,-1.12109502864222E-15));
#42156=DIRECTION('',(-3.60315789384389E-15,1.12109502864222E-15,-1.));
#42157=DIRECTION('',(-4.72840468318833E-16,-1.,-1.12109502864222E-15));
#42158=DIRECTION('',(-3.60315789384389E-15,1.12109502864222E-15,-1.));
#42159=DIRECTION('center_axis',(-4.72840468318833E-16,-1.,-1.12109502864222E-15));
#42160=DIRECTION('ref_axis',(3.60315789384389E-15,-1.12109502864222E-15,
1.));
#42161=DIRECTION('center_axis',(4.72840468318833E-16,1.,1.12109502864222E-15));
#42162=DIRECTION('ref_axis',(3.60315789384389E-15,-1.12109502864222E-15,
1.));
#42163=DIRECTION('',(-4.72840468318833E-16,-1.,-1.12109502864222E-15));
#42164=DIRECTION('center_axis',(4.72840468318833E-16,1.,1.12109502864222E-15));
#42165=DIRECTION('ref_axis',(3.60315789384389E-15,-1.12109502864222E-15,
1.));
#42166=DIRECTION('center_axis',(-3.04804638153131E-15,1.12109502864222E-15,
-1.));
#42167=DIRECTION('ref_axis',(-4.72840468318833E-16,-1.,-1.12109502864222E-15));
#42168=DIRECTION('',(-1.,4.7284046831883E-16,3.04804638153131E-15));
#42169=DIRECTION('',(-4.72840468318833E-16,-1.,-1.12109502864222E-15));
#42170=DIRECTION('',(-1.,4.7284046831883E-16,3.04804638153131E-15));
#42171=DIRECTION('center_axis',(-4.72840468318833E-16,-1.,-1.12109502864222E-15));
#42172=DIRECTION('ref_axis',(1.,-4.72840468318829E-16,-3.60315789384389E-15));
#42173=DIRECTION('center_axis',(4.72840468318833E-16,1.,1.12109502864222E-15));
#42174=DIRECTION('ref_axis',(1.,-4.72840468318829E-16,-3.60315789384389E-15));
#42175=DIRECTION('center_axis',(4.72840468318833E-16,1.,1.12109502864222E-15));
#42176=DIRECTION('ref_axis',(1.,-4.72840468318829E-16,-3.60315789384389E-15));
#42177=DIRECTION('center_axis',(-4.72840468318833E-16,-1.,-1.12109502864222E-15));
#42178=DIRECTION('ref_axis',(-1.,4.72840468318829E-16,3.60315789384389E-15));
#42179=DIRECTION('center_axis',(-4.72840468318833E-16,-1.,-1.12109502864222E-15));
#42180=DIRECTION('ref_axis',(-1.,4.72840468318829E-16,3.60315789384389E-15));
#42181=DIRECTION('center_axis',(-3.34404360992238E-15,-1.45117688885522E-12,
-1.));
#42182=DIRECTION('ref_axis',(-5.00596043931499E-16,-1.,1.45117688885522E-12));
#42183=DIRECTION('center_axis',(-3.34404360992238E-15,-1.45117688885522E-12,
-1.));
#42184=DIRECTION('ref_axis',(-5.00596043931499E-16,-1.,1.45117688885522E-12));
#42185=DIRECTION('',(-3.34404360992238E-15,-1.45117688885522E-12,-1.));
#42186=DIRECTION('center_axis',(3.34404360992238E-15,1.45117688885522E-12,
1.));
#42187=DIRECTION('ref_axis',(-5.00596043931499E-16,-1.,1.45117688885522E-12));
#42188=DIRECTION('',(-3.34404360992238E-15,-1.45117688885522E-12,-1.));
#42189=DIRECTION('center_axis',(-2.72104209318181E-15,-1.,1.45117688885522E-12));
#42190=DIRECTION('ref_axis',(-1.,2.72104209318666E-15,3.34404360991843E-15));
#42191=DIRECTION('',(-1.,2.72104209318666E-15,3.34404360991843E-15));
#42192=DIRECTION('',(-3.34404360992238E-15,-1.45117688885522E-12,-1.));
#42193=DIRECTION('',(1.,-2.72104209318666E-15,-3.34404360991843E-15));
#42194=DIRECTION('center_axis',(-3.34404360992238E-15,-1.45117688885522E-12,
-1.));
#42195=DIRECTION('ref_axis',(1.,-5.00596043936352E-16,-3.34404360992165E-15));
#42196=DIRECTION('center_axis',(-3.34404360992238E-15,-1.45117688885522E-12,
-1.));
#42197=DIRECTION('ref_axis',(1.,-5.00596043936352E-16,-3.34404360992165E-15));
#42198=DIRECTION('',(-3.34404360992238E-15,-1.45117688885522E-12,-1.));
#42199=DIRECTION('center_axis',(3.34404360992238E-15,1.45117688885522E-12,
1.));
#42200=DIRECTION('ref_axis',(1.,-5.00596043936352E-16,-3.34404360992165E-15));
#42201=DIRECTION('center_axis',(1.,-5.00596043936352E-16,-3.34404360992165E-15));
#42202=DIRECTION('ref_axis',(-5.00596043931499E-16,-1.,1.45117688885522E-12));
#42203=DIRECTION('',(-5.00596043931499E-16,-1.,1.45117688885522E-12));
#42204=DIRECTION('',(-3.34404360992238E-15,-1.45117688885522E-12,-1.));
#42205=DIRECTION('',(5.00596043931499E-16,1.,-1.45117688885522E-12));
#42206=DIRECTION('center_axis',(-3.34404360992238E-15,-1.45117688885522E-12,
-1.));
#42207=DIRECTION('ref_axis',(-1.72629723500711E-14,1.,-1.45117688885522E-12));
#42208=DIRECTION('center_axis',(-3.34404360992238E-15,-1.45117688885522E-12,
-1.));
#42209=DIRECTION('ref_axis',(-1.72629723500711E-14,1.,-1.45117688885522E-12));
#42210=DIRECTION('',(-3.34404360992238E-15,-1.45117688885522E-12,-1.));
#42211=DIRECTION('center_axis',(3.34404360992238E-15,1.45117688885522E-12,
1.));
#42212=DIRECTION('ref_axis',(-1.72629723500711E-14,1.,-1.45117688885522E-12));
#42213=DIRECTION('center_axis',(5.00596043931499E-16,1.,-1.45117688885522E-12));
#42214=DIRECTION('ref_axis',(1.,-5.00596043936352E-16,-3.34404360992165E-15));
#42215=DIRECTION('',(1.,-5.00596043936352E-16,-3.34404360992165E-15));
#42216=DIRECTION('',(-3.34404360992238E-15,-1.45117688885522E-12,-1.));
#42217=DIRECTION('',(-1.,5.00596043936352E-16,3.34404360992165E-15));
#42218=DIRECTION('center_axis',(-3.34404360992238E-15,-1.45117688885522E-12,
-1.));
#42219=DIRECTION('ref_axis',(-1.,5.00596043936352E-16,3.34404360992165E-15));
#42220=DIRECTION('center_axis',(-3.34404360992238E-15,-1.45117688885522E-12,
-1.));
#42221=DIRECTION('ref_axis',(-1.,5.00596043936352E-16,3.34404360992165E-15));
#42222=DIRECTION('',(-3.34404360992238E-15,-1.45117688885522E-12,-1.));
#42223=DIRECTION('center_axis',(3.34404360992238E-15,1.45117688885522E-12,
1.));
#42224=DIRECTION('ref_axis',(-1.,5.00596043936352E-16,3.34404360992165E-15));
#42225=DIRECTION('center_axis',(-1.,5.00596043936352E-16,3.34404360992165E-15));
#42226=DIRECTION('ref_axis',(5.00596043931499E-16,1.,-1.45117688885522E-12));
#42227=DIRECTION('',(5.00596043931499E-16,1.,-1.45117688885522E-12));
#42228=DIRECTION('',(-5.00596043931499E-16,-1.,1.45117688885522E-12));
#42229=DIRECTION('center_axis',(-3.34404360992238E-15,-1.45117688885522E-12,
-1.));
#42230=DIRECTION('ref_axis',(1.,-2.49924255013345E-12,-3.34404360629554E-15));
#42231=DIRECTION('center_axis',(3.34404360992238E-15,1.45117688885522E-12,
1.));
#42232=DIRECTION('ref_axis',(1.,-2.49924255013345E-12,-3.34404360629554E-15));
#42233=DIRECTION('',(-3.34404360992238E-15,-1.45117688885522E-12,-1.));
#42234=DIRECTION('center_axis',(-3.34404360992238E-15,-1.45117688885522E-12,
-1.));
#42235=DIRECTION('ref_axis',(1.,-2.49924255013345E-12,-3.34404360629554E-15));
#42236=DIRECTION('',(-3.34404360992238E-15,-1.45117688885522E-12,-1.));
#42237=DIRECTION('center_axis',(-1.,5.00596043936352E-16,3.34404360992165E-15));
#42238=DIRECTION('ref_axis',(5.00596043931499E-16,1.,-1.45117688885522E-12));
#42239=DIRECTION('',(-5.00596043931499E-16,-1.,1.45117688885522E-12));
#42240=DIRECTION('',(5.00596043931499E-16,1.,-1.45117688885522E-12));
#42241=DIRECTION('',(-3.34404360992238E-15,-1.45117688885522E-12,-1.));
#42242=DIRECTION('center_axis',(-3.34404360992238E-15,-1.45117688885522E-12,
-1.));
#42243=DIRECTION('ref_axis',(9.41969720926E-13,1.,-1.45117688885522E-12));
#42244=DIRECTION('center_axis',(3.34404360992238E-15,1.45117688885522E-12,
1.));
#42245=DIRECTION('ref_axis',(9.41969720926E-13,1.,-1.45117688885522E-12));
#42246=DIRECTION('center_axis',(-3.34404360992238E-15,-1.45117688885522E-12,
-1.));
#42247=DIRECTION('ref_axis',(9.41969720926E-13,1.,-1.45117688885522E-12));
#42248=DIRECTION('',(-3.34404360992238E-15,-1.45117688885522E-12,-1.));
#42249=DIRECTION('center_axis',(-5.00596043931499E-16,-1.,1.45117688885522E-12));
#42250=DIRECTION('ref_axis',(-1.,5.00596043936352E-16,3.34404360992165E-15));
#42251=DIRECTION('',(1.,-5.00596043936352E-16,-3.34404360992165E-15));
#42252=DIRECTION('',(-1.,5.00596043936352E-16,3.34404360992165E-15));
#42253=DIRECTION('',(-3.34404360992238E-15,-1.45117688885522E-12,-1.));
#42254=DIRECTION('center_axis',(-3.34404360992238E-15,-1.45117688885522E-12,
-1.));
#42255=DIRECTION('ref_axis',(-1.,2.35121281351676E-12,3.34404360651035E-15));
#42256=DIRECTION('center_axis',(3.34404360992238E-15,1.45117688885522E-12,
1.));
#42257=DIRECTION('ref_axis',(-1.,2.35121281351676E-12,3.34404360651035E-15));
#42258=DIRECTION('center_axis',(-3.34404360992238E-15,-1.45117688885522E-12,
-1.));
#42259=DIRECTION('ref_axis',(-1.,2.35121281351676E-12,3.34404360651035E-15));
#42260=DIRECTION('',(-3.34404360992238E-15,-1.45117688885522E-12,-1.));
#42261=DIRECTION('center_axis',(1.,-5.00596043936352E-16,-3.34404360992165E-15));
#42262=DIRECTION('ref_axis',(-5.00596043931499E-16,-1.,1.45117688885522E-12));
#42263=DIRECTION('',(5.00596043931499E-16,1.,-1.45117688885522E-12));
#42264=DIRECTION('',(-5.00596043931499E-16,-1.,1.45117688885522E-12));
#42265=DIRECTION('',(-3.34404360992238E-15,-1.45117688885522E-12,-1.));
#42266=DIRECTION('center_axis',(-3.34404360992238E-15,-1.45117688885522E-12,
-1.));
#42267=DIRECTION('ref_axis',(2.15629266646105E-12,-1.,1.45117688885521E-12));
#42268=DIRECTION('center_axis',(3.34404360992238E-15,1.45117688885522E-12,
1.));
#42269=DIRECTION('ref_axis',(2.15629266646105E-12,-1.,1.45117688885521E-12));
#42270=DIRECTION('center_axis',(-3.34404360992238E-15,-1.45117688885522E-12,
-1.));
#42271=DIRECTION('ref_axis',(2.15629266646105E-12,-1.,1.45117688885521E-12));
#42272=DIRECTION('',(-3.34404360992238E-15,-1.45117688885522E-12,-1.));
#42273=DIRECTION('center_axis',(5.00596043931499E-16,1.,-1.45117688885522E-12));
#42274=DIRECTION('ref_axis',(1.,-5.00596043936352E-16,-3.34404360992165E-15));
#42275=DIRECTION('',(-1.,5.00596043936352E-16,3.34404360992165E-15));
#42276=DIRECTION('',(1.,-5.00596043936352E-16,-3.34404360992165E-15));
#42277=DIRECTION('center_axis',(-3.34404360992238E-15,-1.45117688885522E-12,
-1.));
#42278=DIRECTION('ref_axis',(-1.,5.00596043936352E-16,3.34404360992165E-15));
#42279=DIRECTION('center_axis',(-3.34404360992238E-15,-1.45117688885522E-12,
-1.));
#42280=DIRECTION('ref_axis',(-1.,5.00596043936352E-16,3.34404360992165E-15));
#42281=DIRECTION('center_axis',(-3.34404360992238E-15,-1.45117688885522E-12,
-1.));
#42282=DIRECTION('ref_axis',(-5.00596043931499E-16,-1.,1.45117688885522E-12));
#42283=DIRECTION('center_axis',(-3.34404360992238E-15,-1.45117688885522E-12,
-1.));
#42284=DIRECTION('ref_axis',(-5.00596043931499E-16,-1.,1.45117688885522E-12));
#42285=DIRECTION('',(-3.34404360992238E-15,-1.45117688885522E-12,-1.));
#42286=DIRECTION('center_axis',(3.34404360992238E-15,1.45117688885522E-12,
1.));
#42287=DIRECTION('ref_axis',(-5.00596043931499E-16,-1.,1.45117688885522E-12));
#42288=DIRECTION('',(-3.34404360992238E-15,-1.45117688885522E-12,-1.));
#42289=DIRECTION('center_axis',(-2.72104209318181E-15,-1.,1.45117688885522E-12));
#42290=DIRECTION('ref_axis',(-1.,2.72104209318666E-15,3.34404360991843E-15));
#42291=DIRECTION('',(-1.,2.72104209318666E-15,3.34404360991843E-15));
#42292=DIRECTION('',(-3.34404360992238E-15,-1.45117688885522E-12,-1.));
#42293=DIRECTION('',(1.,-2.72104209318666E-15,-3.34404360991843E-15));
#42294=DIRECTION('center_axis',(-3.34404360992238E-15,-1.45117688885522E-12,
-1.));
#42295=DIRECTION('ref_axis',(1.,-5.00596043936352E-16,-3.34404360992165E-15));
#42296=DIRECTION('center_axis',(-3.34404360992238E-15,-1.45117688885522E-12,
-1.));
#42297=DIRECTION('ref_axis',(1.,-5.00596043936352E-16,-3.34404360992165E-15));
#42298=DIRECTION('',(-3.34404360992238E-15,-1.45117688885522E-12,-1.));
#42299=DIRECTION('center_axis',(3.34404360992238E-15,1.45117688885522E-12,
1.));
#42300=DIRECTION('ref_axis',(1.,-5.00596043936352E-16,-3.34404360992165E-15));
#42301=DIRECTION('center_axis',(1.,-5.00596043936352E-16,-3.34404360992165E-15));
#42302=DIRECTION('ref_axis',(-5.00596043931499E-16,-1.,1.45117688885522E-12));
#42303=DIRECTION('',(-5.00596043931499E-16,-1.,1.45117688885522E-12));
#42304=DIRECTION('',(-3.34404360992238E-15,-1.45117688885522E-12,-1.));
#42305=DIRECTION('',(5.00596043931499E-16,1.,-1.45117688885522E-12));
#42306=DIRECTION('center_axis',(-3.34404360992238E-15,-1.45117688885522E-12,
-1.));
#42307=DIRECTION('ref_axis',(-1.72629723500711E-14,1.,-1.45117688885522E-12));
#42308=DIRECTION('center_axis',(-3.34404360992238E-15,-1.45117688885522E-12,
-1.));
#42309=DIRECTION('ref_axis',(-1.72629723500711E-14,1.,-1.45117688885522E-12));
#42310=DIRECTION('',(-3.34404360992238E-15,-1.45117688885522E-12,-1.));
#42311=DIRECTION('center_axis',(3.34404360992238E-15,1.45117688885522E-12,
1.));
#42312=DIRECTION('ref_axis',(-1.72629723500711E-14,1.,-1.45117688885522E-12));
#42313=DIRECTION('center_axis',(5.00596043931499E-16,1.,-1.45117688885522E-12));
#42314=DIRECTION('ref_axis',(1.,-5.00596043936352E-16,-3.34404360992165E-15));
#42315=DIRECTION('',(1.,-5.00596043936352E-16,-3.34404360992165E-15));
#42316=DIRECTION('',(-3.34404360992238E-15,-1.45117688885522E-12,-1.));
#42317=DIRECTION('',(-1.,5.00596043936352E-16,3.34404360992165E-15));
#42318=DIRECTION('center_axis',(-3.34404360992238E-15,-1.45117688885522E-12,
-1.));
#42319=DIRECTION('ref_axis',(-1.,5.00596043936352E-16,3.34404360992165E-15));
#42320=DIRECTION('center_axis',(-3.34404360992238E-15,-1.45117688885522E-12,
-1.));
#42321=DIRECTION('ref_axis',(-1.,5.00596043936352E-16,3.34404360992165E-15));
#42322=DIRECTION('',(-3.34404360992238E-15,-1.45117688885522E-12,-1.));
#42323=DIRECTION('center_axis',(3.34404360992238E-15,1.45117688885522E-12,
1.));
#42324=DIRECTION('ref_axis',(-1.,5.00596043936352E-16,3.34404360992165E-15));
#42325=DIRECTION('center_axis',(-1.,5.00596043936352E-16,3.34404360992165E-15));
#42326=DIRECTION('ref_axis',(5.00596043931499E-16,1.,-1.45117688885522E-12));
#42327=DIRECTION('',(5.00596043931499E-16,1.,-1.45117688885522E-12));
#42328=DIRECTION('',(-5.00596043931499E-16,-1.,1.45117688885522E-12));
#42329=DIRECTION('center_axis',(-3.34404360992238E-15,-1.45117688885522E-12,
-1.));
#42330=DIRECTION('ref_axis',(1.,-2.49924255013345E-12,-3.34404360629554E-15));
#42331=DIRECTION('center_axis',(3.34404360992238E-15,1.45117688885522E-12,
1.));
#42332=DIRECTION('ref_axis',(1.,-2.49924255013345E-12,-3.34404360629554E-15));
#42333=DIRECTION('',(-3.34404360992238E-15,-1.45117688885522E-12,-1.));
#42334=DIRECTION('center_axis',(-3.34404360992238E-15,-1.45117688885522E-12,
-1.));
#42335=DIRECTION('ref_axis',(1.,-2.49924255013345E-12,-3.34404360629554E-15));
#42336=DIRECTION('',(-3.34404360992238E-15,-1.45117688885522E-12,-1.));
#42337=DIRECTION('center_axis',(-1.,5.00596043936352E-16,3.34404360992165E-15));
#42338=DIRECTION('ref_axis',(5.00596043931499E-16,1.,-1.45117688885522E-12));
#42339=DIRECTION('',(-5.00596043931499E-16,-1.,1.45117688885522E-12));
#42340=DIRECTION('',(5.00596043931499E-16,1.,-1.45117688885522E-12));
#42341=DIRECTION('',(-3.34404360992238E-15,-1.45117688885522E-12,-1.));
#42342=DIRECTION('center_axis',(-3.34404360992238E-15,-1.45117688885522E-12,
-1.));
#42343=DIRECTION('ref_axis',(9.41969720926E-13,1.,-1.45117688885522E-12));
#42344=DIRECTION('center_axis',(3.34404360992238E-15,1.45117688885522E-12,
1.));
#42345=DIRECTION('ref_axis',(9.41969720926E-13,1.,-1.45117688885522E-12));
#42346=DIRECTION('center_axis',(-3.34404360992238E-15,-1.45117688885522E-12,
-1.));
#42347=DIRECTION('ref_axis',(9.41969720926E-13,1.,-1.45117688885522E-12));
#42348=DIRECTION('',(-3.34404360992238E-15,-1.45117688885522E-12,-1.));
#42349=DIRECTION('center_axis',(-5.00596043931499E-16,-1.,1.45117688885522E-12));
#42350=DIRECTION('ref_axis',(-1.,5.00596043936352E-16,3.34404360992165E-15));
#42351=DIRECTION('',(1.,-5.00596043936352E-16,-3.34404360992165E-15));
#42352=DIRECTION('',(-1.,5.00596043936352E-16,3.34404360992165E-15));
#42353=DIRECTION('',(-3.34404360992238E-15,-1.45117688885522E-12,-1.));
#42354=DIRECTION('center_axis',(-3.34404360992238E-15,-1.45117688885522E-12,
-1.));
#42355=DIRECTION('ref_axis',(-1.,2.35121281351676E-12,3.34404360651035E-15));
#42356=DIRECTION('center_axis',(3.34404360992238E-15,1.45117688885522E-12,
1.));
#42357=DIRECTION('ref_axis',(-1.,2.35121281351676E-12,3.34404360651035E-15));
#42358=DIRECTION('center_axis',(-3.34404360992238E-15,-1.45117688885522E-12,
-1.));
#42359=DIRECTION('ref_axis',(-1.,2.35121281351676E-12,3.34404360651035E-15));
#42360=DIRECTION('',(-3.34404360992238E-15,-1.45117688885522E-12,-1.));
#42361=DIRECTION('center_axis',(1.,-5.00596043936352E-16,-3.34404360992165E-15));
#42362=DIRECTION('ref_axis',(-5.00596043931499E-16,-1.,1.45117688885522E-12));
#42363=DIRECTION('',(5.00596043931499E-16,1.,-1.45117688885522E-12));
#42364=DIRECTION('',(-5.00596043931499E-16,-1.,1.45117688885522E-12));
#42365=DIRECTION('',(-3.34404360992238E-15,-1.45117688885522E-12,-1.));
#42366=DIRECTION('center_axis',(-3.34404360992238E-15,-1.45117688885522E-12,
-1.));
#42367=DIRECTION('ref_axis',(2.15629266646105E-12,-1.,1.45117688885521E-12));
#42368=DIRECTION('center_axis',(3.34404360992238E-15,1.45117688885522E-12,
1.));
#42369=DIRECTION('ref_axis',(2.15629266646105E-12,-1.,1.45117688885521E-12));
#42370=DIRECTION('center_axis',(-3.34404360992238E-15,-1.45117688885522E-12,
-1.));
#42371=DIRECTION('ref_axis',(2.15629266646105E-12,-1.,1.45117688885521E-12));
#42372=DIRECTION('',(-3.34404360992238E-15,-1.45117688885522E-12,-1.));
#42373=DIRECTION('center_axis',(5.00596043931499E-16,1.,-1.45117688885522E-12));
#42374=DIRECTION('ref_axis',(1.,-5.00596043936352E-16,-3.34404360992165E-15));
#42375=DIRECTION('',(-1.,5.00596043936352E-16,3.34404360992165E-15));
#42376=DIRECTION('',(1.,-5.00596043936352E-16,-3.34404360992165E-15));
#42377=DIRECTION('center_axis',(-3.34404360992238E-15,-1.45117688885522E-12,
-1.));
#42378=DIRECTION('ref_axis',(-1.,5.00596043936352E-16,3.34404360992165E-15));
#42379=DIRECTION('center_axis',(-3.34404360992238E-15,-1.45117688885522E-12,
-1.));
#42380=DIRECTION('ref_axis',(-1.,5.00596043936352E-16,3.34404360992165E-15));
#42381=DIRECTION('center_axis',(-3.34404360992238E-15,-1.45117688885522E-12,
-1.));
#42382=DIRECTION('ref_axis',(-5.00596043931499E-16,-1.,1.45117688885522E-12));
#42383=DIRECTION('center_axis',(-3.34404360992238E-15,-1.45117688885522E-12,
-1.));
#42384=DIRECTION('ref_axis',(-5.00596043931499E-16,-1.,1.45117688885522E-12));
#42385=DIRECTION('',(-3.34404360992238E-15,-1.45117688885522E-12,-1.));
#42386=DIRECTION('center_axis',(3.34404360992238E-15,1.45117688885522E-12,
1.));
#42387=DIRECTION('ref_axis',(-5.00596043931499E-16,-1.,1.45117688885522E-12));
#42388=DIRECTION('',(-3.34404360992238E-15,-1.45117688885522E-12,-1.));
#42389=DIRECTION('center_axis',(-2.72104209318181E-15,-1.,1.45117688885522E-12));
#42390=DIRECTION('ref_axis',(-1.,2.72104209318666E-15,3.34404360991843E-15));
#42391=DIRECTION('',(-1.,2.72104209318666E-15,3.34404360991843E-15));
#42392=DIRECTION('',(-3.34404360992238E-15,-1.45117688885522E-12,-1.));
#42393=DIRECTION('',(1.,-2.72104209318666E-15,-3.34404360991843E-15));
#42394=DIRECTION('center_axis',(-3.34404360992238E-15,-1.45117688885522E-12,
-1.));
#42395=DIRECTION('ref_axis',(1.,-5.00596043936352E-16,-3.34404360992165E-15));
#42396=DIRECTION('center_axis',(-3.34404360992238E-15,-1.45117688885522E-12,
-1.));
#42397=DIRECTION('ref_axis',(1.,-5.00596043936352E-16,-3.34404360992165E-15));
#42398=DIRECTION('',(-3.34404360992238E-15,-1.45117688885522E-12,-1.));
#42399=DIRECTION('center_axis',(3.34404360992238E-15,1.45117688885522E-12,
1.));
#42400=DIRECTION('ref_axis',(1.,-5.00596043936352E-16,-3.34404360992165E-15));
#42401=DIRECTION('center_axis',(1.,-5.00596043936352E-16,-3.34404360992165E-15));
#42402=DIRECTION('ref_axis',(-5.00596043931499E-16,-1.,1.45117688885522E-12));
#42403=DIRECTION('',(-5.00596043931499E-16,-1.,1.45117688885522E-12));
#42404=DIRECTION('',(-3.34404360992238E-15,-1.45117688885522E-12,-1.));
#42405=DIRECTION('',(5.00596043931499E-16,1.,-1.45117688885522E-12));
#42406=DIRECTION('center_axis',(-3.34404360992238E-15,-1.45117688885522E-12,
-1.));
#42407=DIRECTION('ref_axis',(-1.72629723500711E-14,1.,-1.45117688885522E-12));
#42408=DIRECTION('center_axis',(-3.34404360992238E-15,-1.45117688885522E-12,
-1.));
#42409=DIRECTION('ref_axis',(-1.72629723500711E-14,1.,-1.45117688885522E-12));
#42410=DIRECTION('',(-3.34404360992238E-15,-1.45117688885522E-12,-1.));
#42411=DIRECTION('center_axis',(3.34404360992238E-15,1.45117688885522E-12,
1.));
#42412=DIRECTION('ref_axis',(-1.72629723500711E-14,1.,-1.45117688885522E-12));
#42413=DIRECTION('center_axis',(5.00596043931499E-16,1.,-1.45117688885522E-12));
#42414=DIRECTION('ref_axis',(1.,-5.00596043936352E-16,-3.34404360992165E-15));
#42415=DIRECTION('',(1.,-5.00596043936352E-16,-3.34404360992165E-15));
#42416=DIRECTION('',(-3.34404360992238E-15,-1.45117688885522E-12,-1.));
#42417=DIRECTION('',(-1.,5.00596043936352E-16,3.34404360992165E-15));
#42418=DIRECTION('center_axis',(-3.34404360992238E-15,-1.45117688885522E-12,
-1.));
#42419=DIRECTION('ref_axis',(-1.,5.00596043936352E-16,3.34404360992165E-15));
#42420=DIRECTION('center_axis',(-3.34404360992238E-15,-1.45117688885522E-12,
-1.));
#42421=DIRECTION('ref_axis',(-1.,5.00596043936352E-16,3.34404360992165E-15));
#42422=DIRECTION('',(-3.34404360992238E-15,-1.45117688885522E-12,-1.));
#42423=DIRECTION('center_axis',(3.34404360992238E-15,1.45117688885522E-12,
1.));
#42424=DIRECTION('ref_axis',(-1.,5.00596043936352E-16,3.34404360992165E-15));
#42425=DIRECTION('center_axis',(-1.,5.00596043936352E-16,3.34404360992165E-15));
#42426=DIRECTION('ref_axis',(5.00596043931499E-16,1.,-1.45117688885522E-12));
#42427=DIRECTION('',(5.00596043931499E-16,1.,-1.45117688885522E-12));
#42428=DIRECTION('',(-5.00596043931499E-16,-1.,1.45117688885522E-12));
#42429=DIRECTION('center_axis',(-3.34404360992238E-15,-1.45117688885522E-12,
-1.));
#42430=DIRECTION('ref_axis',(1.,-2.49924255013345E-12,-3.34404360629554E-15));
#42431=DIRECTION('center_axis',(3.34404360992238E-15,1.45117688885522E-12,
1.));
#42432=DIRECTION('ref_axis',(1.,-2.49924255013345E-12,-3.34404360629554E-15));
#42433=DIRECTION('',(-3.34404360992238E-15,-1.45117688885522E-12,-1.));
#42434=DIRECTION('center_axis',(-3.34404360992238E-15,-1.45117688885522E-12,
-1.));
#42435=DIRECTION('ref_axis',(1.,-2.49924255013345E-12,-3.34404360629554E-15));
#42436=DIRECTION('',(-3.34404360992238E-15,-1.45117688885522E-12,-1.));
#42437=DIRECTION('center_axis',(-1.,5.00596043936352E-16,3.34404360992165E-15));
#42438=DIRECTION('ref_axis',(5.00596043931499E-16,1.,-1.45117688885522E-12));
#42439=DIRECTION('',(-5.00596043931499E-16,-1.,1.45117688885522E-12));
#42440=DIRECTION('',(5.00596043931499E-16,1.,-1.45117688885522E-12));
#42441=DIRECTION('',(-3.34404360992238E-15,-1.45117688885522E-12,-1.));
#42442=DIRECTION('center_axis',(-3.34404360992238E-15,-1.45117688885522E-12,
-1.));
#42443=DIRECTION('ref_axis',(9.41969720926E-13,1.,-1.45117688885522E-12));
#42444=DIRECTION('center_axis',(3.34404360992238E-15,1.45117688885522E-12,
1.));
#42445=DIRECTION('ref_axis',(9.41969720926E-13,1.,-1.45117688885522E-12));
#42446=DIRECTION('center_axis',(-3.34404360992238E-15,-1.45117688885522E-12,
-1.));
#42447=DIRECTION('ref_axis',(9.41969720926E-13,1.,-1.45117688885522E-12));
#42448=DIRECTION('',(-3.34404360992238E-15,-1.45117688885522E-12,-1.));
#42449=DIRECTION('center_axis',(-5.00596043931499E-16,-1.,1.45117688885522E-12));
#42450=DIRECTION('ref_axis',(-1.,5.00596043936352E-16,3.34404360992165E-15));
#42451=DIRECTION('',(1.,-5.00596043936352E-16,-3.34404360992165E-15));
#42452=DIRECTION('',(-1.,5.00596043936352E-16,3.34404360992165E-15));
#42453=DIRECTION('',(-3.34404360992238E-15,-1.45117688885522E-12,-1.));
#42454=DIRECTION('center_axis',(-3.34404360992238E-15,-1.45117688885522E-12,
-1.));
#42455=DIRECTION('ref_axis',(-1.,2.35121281351676E-12,3.34404360651035E-15));
#42456=DIRECTION('center_axis',(3.34404360992238E-15,1.45117688885522E-12,
1.));
#42457=DIRECTION('ref_axis',(-1.,2.35121281351676E-12,3.34404360651035E-15));
#42458=DIRECTION('center_axis',(-3.34404360992238E-15,-1.45117688885522E-12,
-1.));
#42459=DIRECTION('ref_axis',(-1.,2.35121281351676E-12,3.34404360651035E-15));
#42460=DIRECTION('',(-3.34404360992238E-15,-1.45117688885522E-12,-1.));
#42461=DIRECTION('center_axis',(1.,-5.00596043936352E-16,-3.34404360992165E-15));
#42462=DIRECTION('ref_axis',(-5.00596043931499E-16,-1.,1.45117688885522E-12));
#42463=DIRECTION('',(5.00596043931499E-16,1.,-1.45117688885522E-12));
#42464=DIRECTION('',(-5.00596043931499E-16,-1.,1.45117688885522E-12));
#42465=DIRECTION('',(-3.34404360992238E-15,-1.45117688885522E-12,-1.));
#42466=DIRECTION('center_axis',(-3.34404360992238E-15,-1.45117688885522E-12,
-1.));
#42467=DIRECTION('ref_axis',(2.15629266646105E-12,-1.,1.45117688885521E-12));
#42468=DIRECTION('center_axis',(3.34404360992238E-15,1.45117688885522E-12,
1.));
#42469=DIRECTION('ref_axis',(2.15629266646105E-12,-1.,1.45117688885521E-12));
#42470=DIRECTION('center_axis',(-3.34404360992238E-15,-1.45117688885522E-12,
-1.));
#42471=DIRECTION('ref_axis',(2.15629266646105E-12,-1.,1.45117688885521E-12));
#42472=DIRECTION('',(-3.34404360992238E-15,-1.45117688885522E-12,-1.));
#42473=DIRECTION('center_axis',(5.00596043931499E-16,1.,-1.45117688885522E-12));
#42474=DIRECTION('ref_axis',(1.,-5.00596043936352E-16,-3.34404360992165E-15));
#42475=DIRECTION('',(-1.,5.00596043936352E-16,3.34404360992165E-15));
#42476=DIRECTION('',(1.,-5.00596043936352E-16,-3.34404360992165E-15));
#42477=DIRECTION('center_axis',(-3.34404360992238E-15,-1.45117688885522E-12,
-1.));
#42478=DIRECTION('ref_axis',(-1.,5.00596043936352E-16,3.34404360992165E-15));
#42479=DIRECTION('center_axis',(-3.34404360992238E-15,-1.45117688885522E-12,
-1.));
#42480=DIRECTION('ref_axis',(-1.,5.00596043936352E-16,3.34404360992165E-15));
#42481=DIRECTION('center_axis',(-3.34404360992238E-15,-1.45117688885522E-12,
-1.));
#42482=DIRECTION('ref_axis',(-5.00596043931499E-16,-1.,1.45117688885522E-12));
#42483=DIRECTION('center_axis',(-3.34404360992238E-15,-1.45117688885522E-12,
-1.));
#42484=DIRECTION('ref_axis',(-5.00596043931499E-16,-1.,1.45117688885522E-12));
#42485=DIRECTION('',(-3.34404360992238E-15,-1.45117688885522E-12,-1.));
#42486=DIRECTION('center_axis',(3.34404360992238E-15,1.45117688885522E-12,
1.));
#42487=DIRECTION('ref_axis',(-5.00596043931499E-16,-1.,1.45117688885522E-12));
#42488=DIRECTION('',(-3.34404360992238E-15,-1.45117688885522E-12,-1.));
#42489=DIRECTION('center_axis',(-2.72104209318181E-15,-1.,1.45117688885522E-12));
#42490=DIRECTION('ref_axis',(-1.,2.72104209318666E-15,3.34404360991843E-15));
#42491=DIRECTION('',(-1.,2.72104209318666E-15,3.34404360991843E-15));
#42492=DIRECTION('',(-3.34404360992238E-15,-1.45117688885522E-12,-1.));
#42493=DIRECTION('',(1.,-2.72104209318666E-15,-3.34404360991843E-15));
#42494=DIRECTION('center_axis',(-3.34404360992238E-15,-1.45117688885522E-12,
-1.));
#42495=DIRECTION('ref_axis',(1.,-5.00596043936352E-16,-3.34404360992165E-15));
#42496=DIRECTION('center_axis',(-3.34404360992238E-15,-1.45117688885522E-12,
-1.));
#42497=DIRECTION('ref_axis',(1.,-5.00596043936352E-16,-3.34404360992165E-15));
#42498=DIRECTION('',(-3.34404360992238E-15,-1.45117688885522E-12,-1.));
#42499=DIRECTION('center_axis',(3.34404360992238E-15,1.45117688885522E-12,
1.));
#42500=DIRECTION('ref_axis',(1.,-5.00596043936352E-16,-3.34404360992165E-15));
#42501=DIRECTION('center_axis',(1.,-5.00596043936352E-16,-3.34404360992165E-15));
#42502=DIRECTION('ref_axis',(-5.00596043931499E-16,-1.,1.45117688885522E-12));
#42503=DIRECTION('',(-5.00596043931499E-16,-1.,1.45117688885522E-12));
#42504=DIRECTION('',(-3.34404360992238E-15,-1.45117688885522E-12,-1.));
#42505=DIRECTION('',(5.00596043931499E-16,1.,-1.45117688885522E-12));
#42506=DIRECTION('center_axis',(-3.34404360992238E-15,-1.45117688885522E-12,
-1.));
#42507=DIRECTION('ref_axis',(-1.72629723500711E-14,1.,-1.45117688885522E-12));
#42508=DIRECTION('center_axis',(-3.34404360992238E-15,-1.45117688885522E-12,
-1.));
#42509=DIRECTION('ref_axis',(-1.72629723500711E-14,1.,-1.45117688885522E-12));
#42510=DIRECTION('',(-3.34404360992238E-15,-1.45117688885522E-12,-1.));
#42511=DIRECTION('center_axis',(3.34404360992238E-15,1.45117688885522E-12,
1.));
#42512=DIRECTION('ref_axis',(-1.72629723500711E-14,1.,-1.45117688885522E-12));
#42513=DIRECTION('center_axis',(5.00596043931499E-16,1.,-1.45117688885522E-12));
#42514=DIRECTION('ref_axis',(1.,-5.00596043936352E-16,-3.34404360992165E-15));
#42515=DIRECTION('',(1.,-5.00596043936352E-16,-3.34404360992165E-15));
#42516=DIRECTION('',(-3.34404360992238E-15,-1.45117688885522E-12,-1.));
#42517=DIRECTION('',(-1.,5.00596043936352E-16,3.34404360992165E-15));
#42518=DIRECTION('center_axis',(-3.34404360992238E-15,-1.45117688885522E-12,
-1.));
#42519=DIRECTION('ref_axis',(-1.,5.00596043936352E-16,3.34404360992165E-15));
#42520=DIRECTION('center_axis',(-3.34404360992238E-15,-1.45117688885522E-12,
-1.));
#42521=DIRECTION('ref_axis',(-1.,5.00596043936352E-16,3.34404360992165E-15));
#42522=DIRECTION('',(-3.34404360992238E-15,-1.45117688885522E-12,-1.));
#42523=DIRECTION('center_axis',(3.34404360992238E-15,1.45117688885522E-12,
1.));
#42524=DIRECTION('ref_axis',(-1.,5.00596043936352E-16,3.34404360992165E-15));
#42525=DIRECTION('center_axis',(-1.,5.00596043936352E-16,3.34404360992165E-15));
#42526=DIRECTION('ref_axis',(5.00596043931499E-16,1.,-1.45117688885522E-12));
#42527=DIRECTION('',(5.00596043931499E-16,1.,-1.45117688885522E-12));
#42528=DIRECTION('',(-5.00596043931499E-16,-1.,1.45117688885522E-12));
#42529=DIRECTION('center_axis',(-3.34404360992238E-15,-1.45117688885522E-12,
-1.));
#42530=DIRECTION('ref_axis',(1.,-2.49924255013345E-12,-3.34404360629554E-15));
#42531=DIRECTION('center_axis',(3.34404360992238E-15,1.45117688885522E-12,
1.));
#42532=DIRECTION('ref_axis',(1.,-2.49924255013345E-12,-3.34404360629554E-15));
#42533=DIRECTION('',(-3.34404360992238E-15,-1.45117688885522E-12,-1.));
#42534=DIRECTION('center_axis',(-3.34404360992238E-15,-1.45117688885522E-12,
-1.));
#42535=DIRECTION('ref_axis',(1.,-2.49924255013345E-12,-3.34404360629554E-15));
#42536=DIRECTION('',(-3.34404360992238E-15,-1.45117688885522E-12,-1.));
#42537=DIRECTION('center_axis',(-1.,5.00596043936352E-16,3.34404360992165E-15));
#42538=DIRECTION('ref_axis',(5.00596043931499E-16,1.,-1.45117688885522E-12));
#42539=DIRECTION('',(-5.00596043931499E-16,-1.,1.45117688885522E-12));
#42540=DIRECTION('',(5.00596043931499E-16,1.,-1.45117688885522E-12));
#42541=DIRECTION('',(-3.34404360992238E-15,-1.45117688885522E-12,-1.));
#42542=DIRECTION('center_axis',(-3.34404360992238E-15,-1.45117688885522E-12,
-1.));
#42543=DIRECTION('ref_axis',(9.41969720926E-13,1.,-1.45117688885522E-12));
#42544=DIRECTION('center_axis',(3.34404360992238E-15,1.45117688885522E-12,
1.));
#42545=DIRECTION('ref_axis',(9.41969720926E-13,1.,-1.45117688885522E-12));
#42546=DIRECTION('center_axis',(-3.34404360992238E-15,-1.45117688885522E-12,
-1.));
#42547=DIRECTION('ref_axis',(9.41969720926E-13,1.,-1.45117688885522E-12));
#42548=DIRECTION('',(-3.34404360992238E-15,-1.45117688885522E-12,-1.));
#42549=DIRECTION('center_axis',(-5.00596043931499E-16,-1.,1.45117688885522E-12));
#42550=DIRECTION('ref_axis',(-1.,5.00596043936352E-16,3.34404360992165E-15));
#42551=DIRECTION('',(1.,-5.00596043936352E-16,-3.34404360992165E-15));
#42552=DIRECTION('',(-1.,5.00596043936352E-16,3.34404360992165E-15));
#42553=DIRECTION('',(-3.34404360992238E-15,-1.45117688885522E-12,-1.));
#42554=DIRECTION('center_axis',(-3.34404360992238E-15,-1.45117688885522E-12,
-1.));
#42555=DIRECTION('ref_axis',(-1.,2.35121281351676E-12,3.34404360651035E-15));
#42556=DIRECTION('center_axis',(3.34404360992238E-15,1.45117688885522E-12,
1.));
#42557=DIRECTION('ref_axis',(-1.,2.35121281351676E-12,3.34404360651035E-15));
#42558=DIRECTION('center_axis',(-3.34404360992238E-15,-1.45117688885522E-12,
-1.));
#42559=DIRECTION('ref_axis',(-1.,2.35121281351676E-12,3.34404360651035E-15));
#42560=DIRECTION('',(-3.34404360992238E-15,-1.45117688885522E-12,-1.));
#42561=DIRECTION('center_axis',(1.,-5.00596043936352E-16,-3.34404360992165E-15));
#42562=DIRECTION('ref_axis',(-5.00596043931499E-16,-1.,1.45117688885522E-12));
#42563=DIRECTION('',(5.00596043931499E-16,1.,-1.45117688885522E-12));
#42564=DIRECTION('',(-5.00596043931499E-16,-1.,1.45117688885522E-12));
#42565=DIRECTION('',(-3.34404360992238E-15,-1.45117688885522E-12,-1.));
#42566=DIRECTION('center_axis',(-3.34404360992238E-15,-1.45117688885522E-12,
-1.));
#42567=DIRECTION('ref_axis',(2.15629266646105E-12,-1.,1.45117688885521E-12));
#42568=DIRECTION('center_axis',(3.34404360992238E-15,1.45117688885522E-12,
1.));
#42569=DIRECTION('ref_axis',(2.15629266646105E-12,-1.,1.45117688885521E-12));
#42570=DIRECTION('center_axis',(-3.34404360992238E-15,-1.45117688885522E-12,
-1.));
#42571=DIRECTION('ref_axis',(2.15629266646105E-12,-1.,1.45117688885521E-12));
#42572=DIRECTION('',(-3.34404360992238E-15,-1.45117688885522E-12,-1.));
#42573=DIRECTION('center_axis',(5.00596043931499E-16,1.,-1.45117688885522E-12));
#42574=DIRECTION('ref_axis',(1.,-5.00596043936352E-16,-3.34404360992165E-15));
#42575=DIRECTION('',(-1.,5.00596043936352E-16,3.34404360992165E-15));
#42576=DIRECTION('',(1.,-5.00596043936352E-16,-3.34404360992165E-15));
#42577=DIRECTION('center_axis',(-3.34404360992238E-15,-1.45117688885522E-12,
-1.));
#42578=DIRECTION('ref_axis',(-1.,5.00596043936352E-16,3.34404360992165E-15));
#42579=DIRECTION('center_axis',(-3.34404360992238E-15,-1.45117688885522E-12,
-1.));
#42580=DIRECTION('ref_axis',(-1.,5.00596043936352E-16,3.34404360992165E-15));
#42581=DIRECTION('axis',(0.,0.,1.));
#42582=DIRECTION('refdir',(1.,0.,0.));
#42583=DIRECTION('axis',(0.,0.,1.));
#42584=DIRECTION('refdir',(1.,0.,0.));
#42585=DIRECTION('center_axis',(5.07060489460067E-16,1.,1.05904684225915E-15));
#42586=DIRECTION('ref_axis',(-5.46077161851015E-15,1.05904684225915E-15,
-1.));
#42587=DIRECTION('center_axis',(4.41572679712592E-16,1.,1.05904684225915E-15));
#42588=DIRECTION('ref_axis',(-5.46077161851015E-15,1.05904684225915E-15,
-1.));
#42589=DIRECTION('',(5.07060489460067E-16,1.,1.05904684225915E-15));
#42590=DIRECTION('center_axis',(-5.07060489460067E-16,-1.,-1.05904684225915E-15));
#42591=DIRECTION('ref_axis',(-5.46077161851015E-15,1.05904684225915E-15,
-1.));
#42592=DIRECTION('center_axis',(5.07060489460067E-16,1.,1.05904684225915E-15));
#42593=DIRECTION('ref_axis',(-5.46077161851015E-15,1.05904684225915E-15,
-1.));
#42594=DIRECTION('center_axis',(4.92735031077807E-16,1.,1.05904684225915E-15));
#42595=DIRECTION('ref_axis',(-5.46077161851015E-15,1.05904684225915E-15,
-1.));
#42596=DIRECTION('',(5.07060489460067E-16,1.,1.05904684225915E-15));
#42597=DIRECTION('center_axis',(-4.41572679712592E-16,-1.,-1.05904684225915E-15));
#42598=DIRECTION('ref_axis',(-5.46077161851015E-15,1.05904684225915E-15,
-1.));
#42599=DIRECTION('center_axis',(5.07060489460067E-16,1.,1.05904684225915E-15));
#42600=DIRECTION('ref_axis',(-5.46077161851015E-15,1.05904684225915E-15,
-1.));
#42601=DIRECTION('center_axis',(4.41572679712592E-16,1.,1.05904684225915E-15));
#42602=DIRECTION('ref_axis',(-5.46077161851015E-15,1.05904684225915E-15,
-1.));
#42603=DIRECTION('',(5.07060489460067E-16,1.,1.05904684225915E-15));
#42604=DIRECTION('center_axis',(-5.07060489460067E-16,-1.,-1.05904684225915E-15));
#42605=DIRECTION('ref_axis',(-5.46077161851015E-15,1.05904684225915E-15,
-1.));
#42606=DIRECTION('center_axis',(5.07060489460067E-16,1.,1.05904684225915E-15));
#42607=DIRECTION('ref_axis',(-5.46077161851015E-15,1.05904684225915E-15,
-1.));
#42608=DIRECTION('center_axis',(4.92735031077807E-16,1.,1.05904684225915E-15));
#42609=DIRECTION('ref_axis',(-5.46077161851015E-15,1.05904684225915E-15,
-1.));
#42610=DIRECTION('',(5.07060489460067E-16,1.,1.05904684225915E-15));
#42611=DIRECTION('center_axis',(-4.41572679712592E-16,-1.,-1.05904684225915E-15));
#42612=DIRECTION('ref_axis',(-5.46077161851015E-15,1.05904684225915E-15,
-1.));
#42613=DIRECTION('center_axis',(5.07060489460067E-16,1.,1.05904684225915E-15));
#42614=DIRECTION('ref_axis',(-5.46077161851015E-15,1.05904684225915E-15,
-1.));
#42615=DIRECTION('center_axis',(4.41572679712592E-16,1.,1.05904684225915E-15));
#42616=DIRECTION('ref_axis',(-5.46077161851015E-15,1.05904684225915E-15,
-1.));
#42617=DIRECTION('',(5.07060489460067E-16,1.,1.05904684225915E-15));
#42618=DIRECTION('center_axis',(-5.07060489460067E-16,-1.,-1.05904684225915E-15));
#42619=DIRECTION('ref_axis',(-5.46077161851015E-15,1.05904684225915E-15,
-1.));
#42620=DIRECTION('center_axis',(5.07060489460067E-16,1.,1.05904684225915E-15));
#42621=DIRECTION('ref_axis',(-5.46077161851015E-15,1.05904684225915E-15,
-1.));
#42622=DIRECTION('center_axis',(4.92735031077807E-16,1.,1.05904684225915E-15));
#42623=DIRECTION('ref_axis',(-5.46077161851015E-15,1.05904684225915E-15,
-1.));
#42624=DIRECTION('',(5.07060489460067E-16,1.,1.05904684225915E-15));
#42625=DIRECTION('center_axis',(-4.41572679712592E-16,-1.,-1.05904684225915E-15));
#42626=DIRECTION('ref_axis',(-5.46077161851015E-15,1.05904684225915E-15,
-1.));
#42627=DIRECTION('center_axis',(5.07060489460067E-16,1.,1.05904684225915E-15));
#42628=DIRECTION('ref_axis',(-5.46077161851015E-15,1.05904684225915E-15,
-1.));
#42629=DIRECTION('center_axis',(4.41572679712592E-16,1.,1.05904684225915E-15));
#42630=DIRECTION('ref_axis',(-5.46077161851015E-15,1.05904684225915E-15,
-1.));
#42631=DIRECTION('',(5.07060489460067E-16,1.,1.05904684225915E-15));
#42632=DIRECTION('center_axis',(-5.07060489460067E-16,-1.,-1.05904684225915E-15));
#42633=DIRECTION('ref_axis',(-5.46077161851015E-15,1.05904684225915E-15,
-1.));
#42634=DIRECTION('center_axis',(5.07060489460067E-16,1.,1.05904684225915E-15));
#42635=DIRECTION('ref_axis',(-5.46077161851015E-15,1.05904684225915E-15,
-1.));
#42636=DIRECTION('center_axis',(4.92735031077807E-16,1.,1.05904684225915E-15));
#42637=DIRECTION('ref_axis',(-5.46077161851015E-15,1.05904684225915E-15,
-1.));
#42638=DIRECTION('',(5.07060489460067E-16,1.,1.05904684225915E-15));
#42639=DIRECTION('center_axis',(-4.41572679712592E-16,-1.,-1.05904684225915E-15));
#42640=DIRECTION('ref_axis',(-5.46077161851015E-15,1.05904684225915E-15,
-1.));
#42641=DIRECTION('center_axis',(5.07060489460067E-16,1.,1.05904684225915E-15));
#42642=DIRECTION('ref_axis',(-5.46077161851015E-15,1.05904684225915E-15,
-1.));
#42643=DIRECTION('center_axis',(4.41572679712592E-16,1.,1.05904684225915E-15));
#42644=DIRECTION('ref_axis',(-5.46077161851015E-15,1.05904684225915E-15,
-1.));
#42645=DIRECTION('',(5.07060489460067E-16,1.,1.05904684225915E-15));
#42646=DIRECTION('center_axis',(-5.07060489460067E-16,-1.,-1.05904684225915E-15));
#42647=DIRECTION('ref_axis',(-5.46077161851015E-15,1.05904684225915E-15,
-1.));
#42648=DIRECTION('center_axis',(5.07060489460067E-16,1.,1.05904684225915E-15));
#42649=DIRECTION('ref_axis',(-5.46077161851015E-15,1.05904684225915E-15,
-1.));
#42650=DIRECTION('center_axis',(4.92735031077807E-16,1.,1.05904684225915E-15));
#42651=DIRECTION('ref_axis',(-5.46077161851015E-15,1.05904684225915E-15,
-1.));
#42652=DIRECTION('',(5.07060489460067E-16,1.,1.05904684225915E-15));
#42653=DIRECTION('center_axis',(-4.41572679712592E-16,-1.,-1.05904684225915E-15));
#42654=DIRECTION('ref_axis',(-5.46077161851015E-15,1.05904684225915E-15,
-1.));
#42655=DIRECTION('center_axis',(5.07060489460067E-16,1.,1.05904684225915E-15));
#42656=DIRECTION('ref_axis',(-5.46077161851015E-15,1.05904684225915E-15,
-1.));
#42657=DIRECTION('center_axis',(4.41572679712592E-16,1.,1.05904684225915E-15));
#42658=DIRECTION('ref_axis',(-5.46077161851015E-15,1.05904684225915E-15,
-1.));
#42659=DIRECTION('',(5.07060489460067E-16,1.,1.05904684225915E-15));
#42660=DIRECTION('center_axis',(-5.07060489460067E-16,-1.,-1.05904684225915E-15));
#42661=DIRECTION('ref_axis',(-5.46077161851015E-15,1.05904684225915E-15,
-1.));
#42662=DIRECTION('center_axis',(5.07060489460067E-16,1.,1.05904684225915E-15));
#42663=DIRECTION('ref_axis',(-5.46077161851015E-15,1.05904684225915E-15,
-1.));
#42664=DIRECTION('center_axis',(4.92735031077807E-16,1.,1.05904684225915E-15));
#42665=DIRECTION('ref_axis',(-5.46077161851015E-15,1.05904684225915E-15,
-1.));
#42666=DIRECTION('',(5.07060489460067E-16,1.,1.05904684225915E-15));
#42667=DIRECTION('center_axis',(-4.41572679712592E-16,-1.,-1.05904684225915E-15));
#42668=DIRECTION('ref_axis',(-5.46077161851015E-15,1.05904684225915E-15,
-1.));
#42669=DIRECTION('center_axis',(5.07060489460067E-16,1.,1.05904684225915E-15));
#42670=DIRECTION('ref_axis',(-5.46077161851015E-15,1.05904684225915E-15,
-1.));
#42671=DIRECTION('center_axis',(4.41572679712592E-16,1.,1.05904684225915E-15));
#42672=DIRECTION('ref_axis',(-5.46077161851015E-15,1.05904684225915E-15,
-1.));
#42673=DIRECTION('',(5.07060489460067E-16,1.,1.05904684225915E-15));
#42674=DIRECTION('center_axis',(-5.07060489460067E-16,-1.,-1.05904684225915E-15));
#42675=DIRECTION('ref_axis',(-5.46077161851015E-15,1.05904684225915E-15,
-1.));
#42676=DIRECTION('center_axis',(5.07060489460067E-16,1.,1.05904684225915E-15));
#42677=DIRECTION('ref_axis',(-5.46077161851015E-15,1.05904684225915E-15,
-1.));
#42678=DIRECTION('center_axis',(4.92735031077807E-16,1.,1.05904684225915E-15));
#42679=DIRECTION('ref_axis',(-5.46077161851015E-15,1.05904684225915E-15,
-1.));
#42680=DIRECTION('',(5.07060489460067E-16,1.,1.05904684225915E-15));
#42681=DIRECTION('center_axis',(-4.41572679712592E-16,-1.,-1.05904684225915E-15));
#42682=DIRECTION('ref_axis',(-5.46077161851015E-15,1.05904684225915E-15,
-1.));
#42683=DIRECTION('center_axis',(5.07060489460067E-16,1.,1.05904684225915E-15));
#42684=DIRECTION('ref_axis',(-5.46077161851015E-15,1.05904684225915E-15,
-1.));
#42685=DIRECTION('center_axis',(4.41572679712592E-16,1.,1.05904684225915E-15));
#42686=DIRECTION('ref_axis',(-5.46077161851015E-15,1.05904684225915E-15,
-1.));
#42687=DIRECTION('',(5.07060489460067E-16,1.,1.05904684225915E-15));
#42688=DIRECTION('center_axis',(-5.07060489460067E-16,-1.,-1.05904684225915E-15));
#42689=DIRECTION('ref_axis',(-5.46077161851015E-15,1.05904684225915E-15,
-1.));
#42690=DIRECTION('center_axis',(5.07060489460067E-16,1.,1.05904684225915E-15));
#42691=DIRECTION('ref_axis',(-5.46077161851015E-15,1.05904684225915E-15,
-1.));
#42692=DIRECTION('center_axis',(4.92735031077807E-16,1.,1.05904684225915E-15));
#42693=DIRECTION('ref_axis',(-5.46077161851015E-15,1.05904684225915E-15,
-1.));
#42694=DIRECTION('',(5.07060489460067E-16,1.,1.05904684225915E-15));
#42695=DIRECTION('center_axis',(-4.41572679712592E-16,-1.,-1.05904684225915E-15));
#42696=DIRECTION('ref_axis',(-5.46077161851015E-15,1.05904684225915E-15,
-1.));
#42697=DIRECTION('center_axis',(-4.41572679712592E-16,-1.,-1.05904684225915E-15));
#42698=DIRECTION('ref_axis',(-1.,4.41572679712586E-16,5.46077161851015E-15));
#42699=DIRECTION('',(5.46077161851015E-15,-1.05904684225915E-15,1.));
#42700=DIRECTION('',(-1.,4.41572679712586E-16,5.46077161851015E-15));
#42701=DIRECTION('',(-5.46077161851015E-15,1.05904684225915E-15,-1.));
#42702=DIRECTION('',(1.,-4.41572679712586E-16,-5.46077161851015E-15));
#42703=DIRECTION('center_axis',(1.,-3.7813136401972E-16,-5.46077161851015E-15));
#42704=DIRECTION('ref_axis',(-3.78131364019726E-16,-1.,-1.05904684225915E-15));
#42705=DIRECTION('',(-3.78131364019726E-16,-1.,-1.05904684225915E-15));
#42706=DIRECTION('',(-5.46077161851015E-15,1.05904684225915E-15,-1.));
#42707=DIRECTION('',(3.78131364019726E-16,1.,1.05904684225915E-15));
#42708=DIRECTION('center_axis',(4.41572679712592E-16,1.,1.05904684225915E-15));
#42709=DIRECTION('ref_axis',(1.,-4.41572679712586E-16,-5.46077161851015E-15));
#42710=DIRECTION('',(1.,-4.41572679712586E-16,-5.46077161851015E-15));
#42711=DIRECTION('',(-5.46077161851015E-15,1.05904684225915E-15,-1.));
#42712=DIRECTION('',(-1.,4.41572679712586E-16,5.46077161851015E-15));
#42713=DIRECTION('center_axis',(-1.,3.7813136401972E-16,5.46077161851015E-15));
#42714=DIRECTION('ref_axis',(3.78131364019726E-16,1.,1.05904684225915E-15));
#42715=DIRECTION('',(3.78131364019726E-16,1.,1.05904684225915E-15));
#42716=DIRECTION('',(-3.78131364019726E-16,-1.,-1.05904684225915E-15));
#42717=DIRECTION('center_axis',(5.46077161851015E-15,-1.05904684225915E-15,
1.));
#42718=DIRECTION('ref_axis',(3.78131364019726E-16,1.,1.05904684225915E-15));
#42719=DIRECTION('',(-3.78131364019726E-16,-1.,-1.05904684225915E-15));
#42720=DIRECTION('',(1.,-4.92735031077801E-16,-5.46077161851015E-15));
#42721=DIRECTION('',(5.6511629448291E-16,1.,1.05904684225915E-15));
#42722=DIRECTION('',(-1.,5.07060489460061E-16,5.46077161851015E-15));
#42723=DIRECTION('center_axis',(-4.92735031077807E-16,-1.,-1.05904684225915E-15));
#42724=DIRECTION('ref_axis',(-1.,4.92735031077801E-16,5.46077161851015E-15));
#42725=DIRECTION('',(5.46077161851015E-15,-1.05904684225915E-15,1.));
#42726=DIRECTION('',(-1.,4.92735031077801E-16,5.46077161851015E-15));
#42727=DIRECTION('',(-5.46077161851015E-15,1.05904684225915E-15,-1.));
#42728=DIRECTION('center_axis',(1.,-5.65116294482904E-16,-5.46077161851015E-15));
#42729=DIRECTION('ref_axis',(-5.6511629448291E-16,-1.,-1.05904684225915E-15));
#42730=DIRECTION('',(-5.6511629448291E-16,-1.,-1.05904684225915E-15));
#42731=DIRECTION('',(-5.46077161851015E-15,1.05904684225915E-15,-1.));
#42732=DIRECTION('center_axis',(5.07060489460067E-16,1.,1.05904684225915E-15));
#42733=DIRECTION('ref_axis',(1.,-5.07060489460061E-16,-5.46077161851015E-15));
#42734=DIRECTION('',(1.,-5.07060489460061E-16,-5.46077161851015E-15));
#42735=DIRECTION('',(-5.46077161851015E-15,1.05904684225915E-15,-1.));
#42736=DIRECTION('center_axis',(-1.,3.7813136401972E-16,5.46077161851015E-15));
#42737=DIRECTION('ref_axis',(3.78131364019726E-16,1.,1.05904684225915E-15));
#42738=DIRECTION('',(3.78131364019726E-16,1.,1.05904684225915E-15));
#42739=DIRECTION('center_axis',(-5.46077161851015E-15,1.05904684225915E-15,
-1.));
#42740=DIRECTION('ref_axis',(-3.78131364019726E-16,-1.,-1.05904684225915E-15));
#42741=DIRECTION('axis',(0.,0.,1.));
#42742=DIRECTION('refdir',(1.,0.,0.));
#42743=DIRECTION('center_axis',(1.,-5.00596043934459E-16,-4.24079044878475E-15));
#42744=DIRECTION('ref_axis',(4.24079044878475E-15,-3.31747701864093E-15,
1.));
#42745=DIRECTION('',(-4.24079044878475E-15,3.31747701864093E-15,-1.));
#42746=DIRECTION('',(-5.00596043934473E-16,-1.,-3.31747701864093E-15));
#42747=DIRECTION('',(4.24079044878475E-15,-3.31747701864093E-15,1.));
#42748=DIRECTION('',(5.00596043934473E-16,1.,3.31747701864093E-15));
#42749=DIRECTION('center_axis',(-1.,5.00596043934459E-16,4.24079044878475E-15));
#42750=DIRECTION('ref_axis',(-5.00596043934473E-16,-1.,-3.31747701864093E-15));
#42751=DIRECTION('center_axis',(-1.,5.00596043934459E-16,4.24079044878475E-15));
#42752=DIRECTION('ref_axis',(-5.00596043934473E-16,-1.,-3.31747701864093E-15));
#42753=DIRECTION('center_axis',(-1.,5.00596043934459E-16,4.24079044878475E-15));
#42754=DIRECTION('ref_axis',(-5.00596043934473E-16,-1.,-3.31747701864093E-15));
#42755=DIRECTION('center_axis',(-1.,5.0059604393446E-16,3.87506992302587E-15));
#42756=DIRECTION('ref_axis',(-3.87506992302587E-15,3.31747701864093E-15,
-1.));
#42757=DIRECTION('',(3.87506992302587E-15,-3.31747701864093E-15,1.));
#42758=DIRECTION('',(-5.00596043934473E-16,-1.,-3.31747701864093E-15));
#42759=DIRECTION('',(-3.87506992302587E-15,3.31747701864093E-15,-1.));
#42760=DIRECTION('',(5.00596043934473E-16,1.,3.31747701864093E-15));
#42761=DIRECTION('center_axis',(1.,-5.0059604393446E-16,-3.87506992302587E-15));
#42762=DIRECTION('ref_axis',(-5.00596043934473E-16,-1.,-3.31747701864093E-15));
#42763=DIRECTION('center_axis',(1.,-5.0059604393446E-16,-3.87506992302587E-15));
#42764=DIRECTION('ref_axis',(-5.00596043934473E-16,-1.,-3.31747701864093E-15));
#42765=DIRECTION('center_axis',(1.,-5.0059604393446E-16,-3.87506992302587E-15));
#42766=DIRECTION('ref_axis',(-5.00596043934473E-16,-1.,-3.31747701864093E-15));
#42767=DIRECTION('center_axis',(3.82282413363175E-15,-3.31747701864093E-15,
1.));
#42768=DIRECTION('ref_axis',(1.,-5.00596043934461E-16,-3.82282413363175E-15));
#42769=DIRECTION('',(-1.,5.0059604393446E-16,3.82282413363175E-15));
#42770=DIRECTION('',(1.,-5.0059604393446E-16,-3.82282413363175E-15));
#42771=DIRECTION('center_axis',(1.,-5.0059604393446E-16,-3.82282413363175E-15));
#42772=DIRECTION('ref_axis',(-5.00596043934473E-16,-1.,-3.31747701864093E-15));
#42773=DIRECTION('',(0.515038074910054,0.857167300702112,9.79705557818207E-16));
#42774=DIRECTION('center_axis',(-1.,5.0059604393446E-16,3.82282413363175E-15));
#42775=DIRECTION('ref_axis',(-5.00596043934473E-16,-1.,-3.31747701864093E-15));
#42776=DIRECTION('center_axis',(-1.,5.0059604393446E-16,3.82282413363175E-15));
#42777=DIRECTION('ref_axis',(-5.00596043934473E-16,-1.,-3.31747701864093E-15));
#42778=DIRECTION('',(-1.,5.0059604393446E-16,3.82282413363175E-15));
#42779=DIRECTION('center_axis',(1.,-5.0059604393446E-16,-3.82282413363175E-15));
#42780=DIRECTION('ref_axis',(-5.00596043934473E-16,-1.,-3.31747701864093E-15));
#42781=DIRECTION('',(0.515038074910054,0.857167300702112,9.79705557818207E-16));
#42782=DIRECTION('center_axis',(-1.,5.0059604393446E-16,3.82282413363175E-15));
#42783=DIRECTION('ref_axis',(-5.00596043934473E-16,-1.,-3.31747701864093E-15));
#42784=DIRECTION('center_axis',(-1.,5.0059604393446E-16,3.82282413363175E-15));
#42785=DIRECTION('ref_axis',(-5.00596043934473E-16,-1.,-3.31747701864093E-15));
#42786=DIRECTION('',(-1.,5.0059604393446E-16,3.82282413363175E-15));
#42787=DIRECTION('center_axis',(1.,-5.0059604393446E-16,-3.82282413363175E-15));
#42788=DIRECTION('ref_axis',(-5.00596043934473E-16,-1.,-3.31747701864093E-15));
#42789=DIRECTION('',(0.515038074910054,0.857167300702112,9.79705557818207E-16));
#42790=DIRECTION('center_axis',(-1.,5.0059604393446E-16,3.82282413363175E-15));
#42791=DIRECTION('ref_axis',(-5.00596043934473E-16,-1.,-3.31747701864093E-15));
#42792=DIRECTION('center_axis',(-1.,5.0059604393446E-16,3.82282413363175E-15));
#42793=DIRECTION('ref_axis',(-5.00596043934473E-16,-1.,-3.31747701864093E-15));
#42794=DIRECTION('',(-1.,5.0059604393446E-16,3.82282413363175E-15));
#42795=DIRECTION('center_axis',(-1.,5.0059604393446E-16,3.82282413363175E-15));
#42796=DIRECTION('ref_axis',(-5.00596043934473E-16,-1.,-3.31747701864093E-15));
#42797=DIRECTION('',(-0.515038074910054,0.857167300702113,4.70756008460127E-15));
#42798=DIRECTION('center_axis',(-1.,5.0059604393446E-16,3.82282413363175E-15));
#42799=DIRECTION('ref_axis',(-5.00596043934473E-16,-1.,-3.31747701864093E-15));
#42800=DIRECTION('center_axis',(-1.,5.0059604393446E-16,3.82282413363175E-15));
#42801=DIRECTION('ref_axis',(-5.00596043934473E-16,-1.,-3.31747701864093E-15));
#42802=DIRECTION('',(-1.,5.0059604393446E-16,3.82282413363175E-15));
#42803=DIRECTION('center_axis',(-1.,5.0059604393446E-16,3.82282413363175E-15));
#42804=DIRECTION('ref_axis',(-5.00596043934473E-16,-1.,-3.31747701864093E-15));
#42805=DIRECTION('',(-0.515038074910054,0.857167300702113,4.70756008460127E-15));
#42806=DIRECTION('center_axis',(-1.,5.0059604393446E-16,3.82282413363175E-15));
#42807=DIRECTION('ref_axis',(-5.00596043934473E-16,-1.,-3.31747701864093E-15));
#42808=DIRECTION('center_axis',(-1.,5.0059604393446E-16,3.82282413363175E-15));
#42809=DIRECTION('ref_axis',(-5.00596043934473E-16,-1.,-3.31747701864093E-15));
#42810=DIRECTION('',(-1.,5.0059604393446E-16,3.82282413363175E-15));
#42811=DIRECTION('center_axis',(-1.,5.0059604393446E-16,3.82282413363175E-15));
#42812=DIRECTION('ref_axis',(-5.00596043934473E-16,-1.,-3.31747701864093E-15));
#42813=DIRECTION('',(-0.515038074910054,0.857167300702113,4.70756008460127E-15));
#42814=DIRECTION('center_axis',(-1.,5.0059604393446E-16,3.82282413363175E-15));
#42815=DIRECTION('ref_axis',(-5.00596043934473E-16,-1.,-3.31747701864093E-15));
#42816=DIRECTION('center_axis',(-1.,5.0059604393446E-16,3.82282413363175E-15));
#42817=DIRECTION('ref_axis',(-5.00596043934473E-16,-1.,-3.31747701864093E-15));
#42818=DIRECTION('',(-1.,5.0059604393446E-16,3.82282413363175E-15));
#42819=DIRECTION('center_axis',(-5.00596043934473E-16,-1.,-3.31747701864093E-15));
#42820=DIRECTION('ref_axis',(-1.,5.0059604393446E-16,3.82282413363175E-15));
#42821=DIRECTION('center_axis',(-5.00596043934473E-16,-1.,-3.31747701864093E-15));
#42822=DIRECTION('ref_axis',(-1.,5.0059604393446E-16,3.82282413363175E-15));
#42823=DIRECTION('',(-5.00596043934473E-16,-1.,-3.31747701864093E-15));
#42824=DIRECTION('center_axis',(5.00596043934473E-16,1.,3.31747701864093E-15));
#42825=DIRECTION('ref_axis',(-1.,5.0059604393446E-16,3.82282413363175E-15));
#42826=DIRECTION('center_axis',(-5.00596043934473E-16,-1.,-3.31747701864093E-15));
#42827=DIRECTION('ref_axis',(-1.,5.0059604393446E-16,3.82282413363175E-15));
#42828=DIRECTION('center_axis',(-5.00596043934473E-16,-1.,-3.31747701864093E-15));
#42829=DIRECTION('ref_axis',(-1.,5.0059604393446E-16,3.82282413363175E-15));
#42830=DIRECTION('',(-5.00596043934473E-16,-1.,-3.31747701864093E-15));
#42831=DIRECTION('center_axis',(5.00596043934473E-16,1.,3.31747701864093E-15));
#42832=DIRECTION('ref_axis',(-1.,5.0059604393446E-16,3.82282413363175E-15));
#42833=DIRECTION('center_axis',(-5.00596043934473E-16,-1.,-3.31747701864093E-15));
#42834=DIRECTION('ref_axis',(-1.,5.0059604393446E-16,3.82282413363175E-15));
#42835=DIRECTION('center_axis',(-5.00596043934473E-16,-1.,-3.31747701864093E-15));
#42836=DIRECTION('ref_axis',(-1.,5.0059604393446E-16,3.82282413363175E-15));
#42837=DIRECTION('',(-5.00596043934473E-16,-1.,-3.31747701864093E-15));
#42838=DIRECTION('center_axis',(5.00596043934473E-16,1.,3.31747701864093E-15));
#42839=DIRECTION('ref_axis',(-1.,5.0059604393446E-16,3.82282413363175E-15));
#42840=DIRECTION('center_axis',(-5.00596043934473E-16,-1.,-3.31747701864093E-15));
#42841=DIRECTION('ref_axis',(-1.,5.0059604393446E-16,3.82282413363175E-15));
#42842=DIRECTION('center_axis',(-5.00596043934473E-16,-1.,-3.31747701864093E-15));
#42843=DIRECTION('ref_axis',(-1.,5.0059604393446E-16,3.82282413363175E-15));
#42844=DIRECTION('',(-5.00596043934473E-16,-1.,-3.31747701864093E-15));
#42845=DIRECTION('center_axis',(5.00596043934473E-16,1.,3.31747701864093E-15));
#42846=DIRECTION('ref_axis',(-1.,5.0059604393446E-16,3.82282413363175E-15));
#42847=DIRECTION('center_axis',(-5.00596043934473E-16,-1.,-3.31747701864093E-15));
#42848=DIRECTION('ref_axis',(-1.,5.0059604393446E-16,3.82282413363175E-15));
#42849=DIRECTION('center_axis',(-5.00596043934473E-16,-1.,-3.31747701864093E-15));
#42850=DIRECTION('ref_axis',(-1.,5.0059604393446E-16,3.82282413363175E-15));
#42851=DIRECTION('',(-5.00596043934473E-16,-1.,-3.31747701864093E-15));
#42852=DIRECTION('center_axis',(5.00596043934473E-16,1.,3.31747701864093E-15));
#42853=DIRECTION('ref_axis',(-1.,5.0059604393446E-16,3.82282413363175E-15));
#42854=DIRECTION('center_axis',(-5.00596043934473E-16,-1.,-3.31747701864093E-15));
#42855=DIRECTION('ref_axis',(-1.,5.0059604393446E-16,3.82282413363175E-15));
#42856=DIRECTION('center_axis',(-5.00596043934473E-16,-1.,-3.31747701864093E-15));
#42857=DIRECTION('ref_axis',(-1.,5.0059604393446E-16,3.82282413363175E-15));
#42858=DIRECTION('',(-5.00596043934473E-16,-1.,-3.31747701864093E-15));
#42859=DIRECTION('center_axis',(5.00596043934473E-16,1.,3.31747701864093E-15));
#42860=DIRECTION('ref_axis',(-1.,5.0059604393446E-16,3.82282413363175E-15));
#42861=DIRECTION('center_axis',(-5.00596043934473E-16,-1.,-3.31747701864093E-15));
#42862=DIRECTION('ref_axis',(-1.,5.0059604393446E-16,3.82282413363175E-15));
#42863=DIRECTION('center_axis',(-5.00596043934473E-16,-1.,-3.31747701864093E-15));
#42864=DIRECTION('ref_axis',(-1.,5.0059604393446E-16,3.82282413363175E-15));
#42865=DIRECTION('',(-5.00596043934473E-16,-1.,-3.31747701864093E-15));
#42866=DIRECTION('center_axis',(5.00596043934473E-16,1.,3.31747701864093E-15));
#42867=DIRECTION('ref_axis',(-1.,5.0059604393446E-16,3.82282413363175E-15));
#42868=DIRECTION('center_axis',(-5.00596043934473E-16,-1.,-3.31747701864093E-15));
#42869=DIRECTION('ref_axis',(-1.,5.0059604393446E-16,3.82282413363175E-15));
#42870=DIRECTION('center_axis',(-5.00596043934473E-16,-1.,-3.31747701864093E-15));
#42871=DIRECTION('ref_axis',(-1.,5.0059604393446E-16,3.82282413363175E-15));
#42872=DIRECTION('',(-5.00596043934473E-16,-1.,-3.31747701864093E-15));
#42873=DIRECTION('center_axis',(5.00596043934473E-16,1.,3.31747701864093E-15));
#42874=DIRECTION('ref_axis',(-1.,5.0059604393446E-16,3.82282413363175E-15));
#42875=DIRECTION('center_axis',(5.00596043934473E-16,1.,3.31747701864093E-15));
#42876=DIRECTION('ref_axis',(1.,-5.0059604393446E-16,-3.82282413363175E-15));
#42877=DIRECTION('center_axis',(5.00596043934473E-16,1.,3.31747701864093E-15));
#42878=DIRECTION('ref_axis',(1.,-5.0059604393446E-16,-3.82282413363175E-15));
#42879=DIRECTION('',(5.00596043934473E-16,1.,3.31747701864093E-15));
#42880=DIRECTION('center_axis',(-5.00596043934473E-16,-1.,-3.31747701864093E-15));
#42881=DIRECTION('ref_axis',(1.,-5.0059604393446E-16,-3.82282413363175E-15));
#42882=DIRECTION('center_axis',(5.00596043934473E-16,1.,3.31747701864093E-15));
#42883=DIRECTION('ref_axis',(1.,-5.0059604393446E-16,-3.82282413363175E-15));
#42884=DIRECTION('center_axis',(5.00596043934473E-16,1.,3.31747701864093E-15));
#42885=DIRECTION('ref_axis',(1.,-5.0059604393446E-16,-3.82282413363175E-15));
#42886=DIRECTION('',(5.00596043934473E-16,1.,3.31747701864093E-15));
#42887=DIRECTION('center_axis',(-5.00596043934473E-16,-1.,-3.31747701864093E-15));
#42888=DIRECTION('ref_axis',(1.,-5.0059604393446E-16,-3.82282413363175E-15));
#42889=DIRECTION('center_axis',(-5.00596043934473E-16,-1.,-3.31747701864093E-15));
#42890=DIRECTION('ref_axis',(1.,-5.00596043934461E-16,-3.82282413363175E-15));
#42891=DIRECTION('',(1.,-5.0059604393446E-16,-3.82282413363175E-15));
#42892=DIRECTION('center_axis',(-3.82282413363175E-15,3.31747701864093E-15,
-1.));
#42893=DIRECTION('ref_axis',(-1.,5.00596043934461E-16,3.82282413363175E-15));
#42894=DIRECTION('',(-1.,5.0059604393446E-16,3.82282413363175E-15));
#42895=DIRECTION('center_axis',(5.00596043934473E-16,1.,3.31747701864093E-15));
#42896=DIRECTION('ref_axis',(-1.,5.00596043934461E-16,3.82282413363175E-15));
#42897=DIRECTION('axis',(0.,0.,1.));
#42898=DIRECTION('refdir',(1.,0.,0.));
#42899=DIRECTION('center_axis',(-1.,5.00596043934458E-16,3.99753460294061E-15));
#42900=DIRECTION('ref_axis',(-3.99753460294061E-15,2.1738969570699E-15,
-1.));
#42901=DIRECTION('',(3.99753460294061E-15,-2.1738969570699E-15,1.));
#42902=DIRECTION('',(-5.00596043934467E-16,-1.,-2.1738969570699E-15));
#42903=DIRECTION('',(-3.99753460294061E-15,2.1738969570699E-15,-1.));
#42904=DIRECTION('',(5.00596043934467E-16,1.,2.1738969570699E-15));
#42905=DIRECTION('center_axis',(1.,-5.00596043934458E-16,-3.99753460294061E-15));
#42906=DIRECTION('ref_axis',(-5.00596043934467E-16,-1.,-2.1738969570699E-15));
#42907=DIRECTION('center_axis',(1.,-5.00596043934458E-16,-3.99753460294061E-15));
#42908=DIRECTION('ref_axis',(-5.00596043934467E-16,-1.,-2.1738969570699E-15));
#42909=DIRECTION('center_axis',(1.,-5.00596043934458E-16,-3.99753460294061E-15));
#42910=DIRECTION('ref_axis',(-5.00596043934467E-16,-1.,-2.1738969570699E-15));
#42911=DIRECTION('center_axis',(1.,-5.00596043934457E-16,-4.37631657604802E-15));
#42912=DIRECTION('ref_axis',(4.37631657604802E-15,-2.1738969570699E-15,
1.));
#42913=DIRECTION('',(-4.37631657604802E-15,2.1738969570699E-15,-1.));
#42914=DIRECTION('',(-5.00596043934467E-16,-1.,-2.1738969570699E-15));
#42915=DIRECTION('',(4.37631657604802E-15,-2.1738969570699E-15,1.));
#42916=DIRECTION('',(5.00596043934467E-16,1.,2.1738969570699E-15));
#42917=DIRECTION('center_axis',(-1.,5.00596043934457E-16,4.37631657604802E-15));
#42918=DIRECTION('ref_axis',(-5.00596043934467E-16,-1.,-2.1738969570699E-15));
#42919=DIRECTION('center_axis',(-1.,5.00596043934457E-16,4.37631657604802E-15));
#42920=DIRECTION('ref_axis',(-5.00596043934467E-16,-1.,-2.1738969570699E-15));
#42921=DIRECTION('center_axis',(-1.,5.00596043934457E-16,4.37631657604802E-15));
#42922=DIRECTION('ref_axis',(-5.00596043934467E-16,-1.,-2.1738969570699E-15));
#42923=DIRECTION('center_axis',(-5.21224920635402E-15,2.1738969570699E-15,
-1.));
#42924=DIRECTION('ref_axis',(-1.,5.00596043934456E-16,5.21224920635402E-15));
#42925=DIRECTION('',(1.,-5.00596043934456E-16,-5.21224920635402E-15));
#42926=DIRECTION('',(-1.,5.00596043934456E-16,5.21224920635402E-15));
#42927=DIRECTION('center_axis',(1.,-5.00596043934456E-16,-5.21224920635402E-15));
#42928=DIRECTION('ref_axis',(-5.00596043934467E-16,-1.,-2.1738969570699E-15));
#42929=DIRECTION('',(0.515038074910054,0.857167300702112,-7.16140691382028E-16));
#42930=DIRECTION('center_axis',(-1.,5.00596043934456E-16,5.21224920635402E-15));
#42931=DIRECTION('ref_axis',(-5.00596043934467E-16,-1.,-2.1738969570699E-15));
#42932=DIRECTION('center_axis',(-1.,5.00596043934456E-16,5.21224920635402E-15));
#42933=DIRECTION('ref_axis',(-5.00596043934467E-16,-1.,-2.1738969570699E-15));
#42934=DIRECTION('',(-1.,5.00596043934456E-16,5.21224920635402E-15));
#42935=DIRECTION('center_axis',(1.,-5.00596043934456E-16,-5.21224920635402E-15));
#42936=DIRECTION('ref_axis',(-5.00596043934467E-16,-1.,-2.1738969570699E-15));
#42937=DIRECTION('',(0.515038074910054,0.857167300702112,-7.16140691382028E-16));
#42938=DIRECTION('center_axis',(-1.,5.00596043934456E-16,5.21224920635402E-15));
#42939=DIRECTION('ref_axis',(-5.00596043934467E-16,-1.,-2.1738969570699E-15));
#42940=DIRECTION('center_axis',(-1.,5.00596043934456E-16,5.21224920635402E-15));
#42941=DIRECTION('ref_axis',(-5.00596043934467E-16,-1.,-2.1738969570699E-15));
#42942=DIRECTION('',(-1.,5.00596043934456E-16,5.21224920635402E-15));
#42943=DIRECTION('center_axis',(1.,-5.00596043934456E-16,-5.21224920635402E-15));
#42944=DIRECTION('ref_axis',(-5.00596043934467E-16,-1.,-2.1738969570699E-15));
#42945=DIRECTION('',(0.515038074910054,0.857167300702112,-7.16140691382028E-16));
#42946=DIRECTION('center_axis',(-1.,5.00596043934456E-16,5.21224920635402E-15));
#42947=DIRECTION('ref_axis',(-5.00596043934467E-16,-1.,-2.1738969570699E-15));
#42948=DIRECTION('center_axis',(-1.,5.00596043934456E-16,5.21224920635402E-15));
#42949=DIRECTION('ref_axis',(-5.00596043934467E-16,-1.,-2.1738969570699E-15));
#42950=DIRECTION('',(-1.,5.00596043934456E-16,5.21224920635402E-15));
#42951=DIRECTION('center_axis',(-1.,5.00596043934456E-16,5.21224920635402E-15));
#42952=DIRECTION('ref_axis',(-5.00596043934467E-16,-1.,-2.1738969570699E-15));
#42953=DIRECTION('',(-0.515038074910054,0.857167300702113,4.44292746477431E-15));
#42954=DIRECTION('center_axis',(-1.,5.00596043934456E-16,5.21224920635402E-15));
#42955=DIRECTION('ref_axis',(-5.00596043934467E-16,-1.,-2.1738969570699E-15));
#42956=DIRECTION('center_axis',(-1.,5.00596043934456E-16,5.21224920635402E-15));
#42957=DIRECTION('ref_axis',(-5.00596043934467E-16,-1.,-2.1738969570699E-15));
#42958=DIRECTION('',(-1.,5.00596043934456E-16,5.21224920635402E-15));
#42959=DIRECTION('center_axis',(-1.,5.00596043934456E-16,5.21224920635402E-15));
#42960=DIRECTION('ref_axis',(-5.00596043934467E-16,-1.,-2.1738969570699E-15));
#42961=DIRECTION('',(-0.515038074910054,0.857167300702113,4.44292746477431E-15));
#42962=DIRECTION('center_axis',(-1.,5.00596043934456E-16,5.21224920635402E-15));
#42963=DIRECTION('ref_axis',(-5.00596043934467E-16,-1.,-2.1738969570699E-15));
#42964=DIRECTION('center_axis',(-1.,5.00596043934456E-16,5.21224920635402E-15));
#42965=DIRECTION('ref_axis',(-5.00596043934467E-16,-1.,-2.1738969570699E-15));
#42966=DIRECTION('',(-1.,5.00596043934456E-16,5.21224920635402E-15));
#42967=DIRECTION('center_axis',(-1.,5.00596043934456E-16,5.21224920635402E-15));
#42968=DIRECTION('ref_axis',(-5.00596043934467E-16,-1.,-2.1738969570699E-15));
#42969=DIRECTION('',(-0.515038074910054,0.857167300702113,4.44292746477431E-15));
#42970=DIRECTION('center_axis',(-1.,5.00596043934456E-16,5.21224920635402E-15));
#42971=DIRECTION('ref_axis',(-5.00596043934467E-16,-1.,-2.1738969570699E-15));
#42972=DIRECTION('center_axis',(-1.,5.00596043934456E-16,5.21224920635402E-15));
#42973=DIRECTION('ref_axis',(-5.00596043934467E-16,-1.,-2.1738969570699E-15));
#42974=DIRECTION('',(-1.,5.00596043934456E-16,5.21224920635402E-15));
#42975=DIRECTION('center_axis',(-5.00596043934467E-16,-1.,-2.1738969570699E-15));
#42976=DIRECTION('ref_axis',(-1.,5.00596043934456E-16,5.21224920635402E-15));
#42977=DIRECTION('center_axis',(-5.00596043934467E-16,-1.,-2.1738969570699E-15));
#42978=DIRECTION('ref_axis',(-1.,5.00596043934456E-16,5.21224920635402E-15));
#42979=DIRECTION('',(-5.00596043934467E-16,-1.,-2.1738969570699E-15));
#42980=DIRECTION('center_axis',(5.00596043934467E-16,1.,2.1738969570699E-15));
#42981=DIRECTION('ref_axis',(-1.,5.00596043934456E-16,5.21224920635402E-15));
#42982=DIRECTION('center_axis',(-5.00596043934467E-16,-1.,-2.1738969570699E-15));
#42983=DIRECTION('ref_axis',(-1.,5.00596043934456E-16,5.21224920635402E-15));
#42984=DIRECTION('center_axis',(-5.00596043934467E-16,-1.,-2.1738969570699E-15));
#42985=DIRECTION('ref_axis',(-1.,5.00596043934456E-16,5.21224920635402E-15));
#42986=DIRECTION('',(-5.00596043934467E-16,-1.,-2.1738969570699E-15));
#42987=DIRECTION('center_axis',(5.00596043934467E-16,1.,2.1738969570699E-15));
#42988=DIRECTION('ref_axis',(-1.,5.00596043934456E-16,5.21224920635402E-15));
#42989=DIRECTION('center_axis',(-5.00596043934467E-16,-1.,-2.1738969570699E-15));
#42990=DIRECTION('ref_axis',(-1.,5.00596043934456E-16,5.21224920635402E-15));
#42991=DIRECTION('center_axis',(-5.00596043934467E-16,-1.,-2.1738969570699E-15));
#42992=DIRECTION('ref_axis',(-1.,5.00596043934456E-16,5.21224920635402E-15));
#42993=DIRECTION('',(-5.00596043934467E-16,-1.,-2.1738969570699E-15));
#42994=DIRECTION('center_axis',(5.00596043934467E-16,1.,2.1738969570699E-15));
#42995=DIRECTION('ref_axis',(-1.,5.00596043934456E-16,5.21224920635402E-15));
#42996=DIRECTION('center_axis',(-5.00596043934467E-16,-1.,-2.1738969570699E-15));
#42997=DIRECTION('ref_axis',(-1.,5.00596043934456E-16,5.21224920635402E-15));
#42998=DIRECTION('center_axis',(-5.00596043934467E-16,-1.,-2.1738969570699E-15));
#42999=DIRECTION('ref_axis',(-1.,5.00596043934456E-16,5.21224920635402E-15));
#43000=DIRECTION('',(-5.00596043934467E-16,-1.,-2.1738969570699E-15));
#43001=DIRECTION('center_axis',(5.00596043934467E-16,1.,2.1738969570699E-15));
#43002=DIRECTION('ref_axis',(-1.,5.00596043934456E-16,5.21224920635402E-15));
#43003=DIRECTION('center_axis',(-5.00596043934467E-16,-1.,-2.1738969570699E-15));
#43004=DIRECTION('ref_axis',(-1.,5.00596043934456E-16,5.21224920635402E-15));
#43005=DIRECTION('center_axis',(-5.00596043934467E-16,-1.,-2.1738969570699E-15));
#43006=DIRECTION('ref_axis',(-1.,5.00596043934456E-16,5.21224920635402E-15));
#43007=DIRECTION('',(-5.00596043934467E-16,-1.,-2.1738969570699E-15));
#43008=DIRECTION('center_axis',(5.00596043934467E-16,1.,2.1738969570699E-15));
#43009=DIRECTION('ref_axis',(-1.,5.00596043934456E-16,5.21224920635402E-15));
#43010=DIRECTION('center_axis',(-5.00596043934467E-16,-1.,-2.1738969570699E-15));
#43011=DIRECTION('ref_axis',(-1.,5.00596043934456E-16,5.21224920635402E-15));
#43012=DIRECTION('center_axis',(-5.00596043934467E-16,-1.,-2.1738969570699E-15));
#43013=DIRECTION('ref_axis',(-1.,5.00596043934456E-16,5.21224920635402E-15));
#43014=DIRECTION('',(-5.00596043934467E-16,-1.,-2.1738969570699E-15));
#43015=DIRECTION('center_axis',(5.00596043934467E-16,1.,2.1738969570699E-15));
#43016=DIRECTION('ref_axis',(-1.,5.00596043934456E-16,5.21224920635402E-15));
#43017=DIRECTION('center_axis',(-5.00596043934467E-16,-1.,-2.1738969570699E-15));
#43018=DIRECTION('ref_axis',(-1.,5.00596043934456E-16,5.21224920635402E-15));
#43019=DIRECTION('center_axis',(-5.00596043934467E-16,-1.,-2.1738969570699E-15));
#43020=DIRECTION('ref_axis',(-1.,5.00596043934456E-16,5.21224920635402E-15));
#43021=DIRECTION('',(-5.00596043934467E-16,-1.,-2.1738969570699E-15));
#43022=DIRECTION('center_axis',(5.00596043934467E-16,1.,2.1738969570699E-15));
#43023=DIRECTION('ref_axis',(-1.,5.00596043934456E-16,5.21224920635402E-15));
#43024=DIRECTION('center_axis',(-5.00596043934467E-16,-1.,-2.1738969570699E-15));
#43025=DIRECTION('ref_axis',(-1.,5.00596043934456E-16,5.21224920635402E-15));
#43026=DIRECTION('center_axis',(-5.00596043934467E-16,-1.,-2.1738969570699E-15));
#43027=DIRECTION('ref_axis',(-1.,5.00596043934456E-16,5.21224920635402E-15));
#43028=DIRECTION('',(-5.00596043934467E-16,-1.,-2.1738969570699E-15));
#43029=DIRECTION('center_axis',(5.00596043934467E-16,1.,2.1738969570699E-15));
#43030=DIRECTION('ref_axis',(-1.,5.00596043934456E-16,5.21224920635402E-15));
#43031=DIRECTION('center_axis',(5.00596043934467E-16,1.,2.1738969570699E-15));
#43032=DIRECTION('ref_axis',(1.,-5.00596043934456E-16,-5.21224920635402E-15));
#43033=DIRECTION('center_axis',(5.00596043934467E-16,1.,2.1738969570699E-15));
#43034=DIRECTION('ref_axis',(1.,-5.00596043934456E-16,-5.21224920635402E-15));
#43035=DIRECTION('',(5.00596043934467E-16,1.,2.1738969570699E-15));
#43036=DIRECTION('center_axis',(-5.00596043934467E-16,-1.,-2.1738969570699E-15));
#43037=DIRECTION('ref_axis',(1.,-5.00596043934456E-16,-5.21224920635402E-15));
#43038=DIRECTION('center_axis',(5.00596043934467E-16,1.,2.1738969570699E-15));
#43039=DIRECTION('ref_axis',(1.,-5.00596043934456E-16,-5.21224920635402E-15));
#43040=DIRECTION('center_axis',(5.00596043934467E-16,1.,2.1738969570699E-15));
#43041=DIRECTION('ref_axis',(1.,-5.00596043934456E-16,-5.21224920635402E-15));
#43042=DIRECTION('',(5.00596043934467E-16,1.,2.1738969570699E-15));
#43043=DIRECTION('center_axis',(-5.00596043934467E-16,-1.,-2.1738969570699E-15));
#43044=DIRECTION('ref_axis',(1.,-5.00596043934456E-16,-5.21224920635402E-15));
#43045=DIRECTION('center_axis',(-5.00596043934467E-16,-1.,-2.1738969570699E-15));
#43046=DIRECTION('ref_axis',(1.,-5.00596043934456E-16,-5.21224920635402E-15));
#43047=DIRECTION('',(-1.,5.00596043934456E-16,5.21224920635402E-15));
#43048=DIRECTION('center_axis',(5.21224920635402E-15,-2.1738969570699E-15,
1.));
#43049=DIRECTION('ref_axis',(1.,-5.00596043934456E-16,-5.21224920635402E-15));
#43050=DIRECTION('',(1.,-5.00596043934456E-16,-5.21224920635402E-15));
#43051=DIRECTION('center_axis',(5.00596043934467E-16,1.,2.1738969570699E-15));
#43052=DIRECTION('ref_axis',(-1.,5.00596043934456E-16,5.21224920635402E-15));
#43053=DIRECTION('axis',(0.,0.,1.));
#43054=DIRECTION('refdir',(1.,0.,0.));
#43055=DIRECTION('center_axis',(1.,-5.0059604393446E-16,-3.87506992302588E-15));
#43056=DIRECTION('ref_axis',(-3.87506992302588E-15,3.31747701864093E-15,
-1.));
#43057=DIRECTION('center_axis',(1.,-5.0059604393446E-16,-3.87506992302588E-15));
#43058=DIRECTION('ref_axis',(-3.87506992302588E-15,3.31747701864093E-15,
-1.));
#43059=DIRECTION('',(1.,-5.0059604393446E-16,-3.87506992302588E-15));
#43060=DIRECTION('center_axis',(-1.,5.0059604393446E-16,3.87506992302588E-15));
#43061=DIRECTION('ref_axis',(-3.87506992302588E-15,3.31747701864093E-15,
-1.));
#43062=DIRECTION('center_axis',(1.,-5.0059604393446E-16,-3.87506992302588E-15));
#43063=DIRECTION('ref_axis',(-3.87506992302588E-15,3.31747701864093E-15,
-1.));
#43064=DIRECTION('center_axis',(1.,-5.0059604393446E-16,-3.87506992302588E-15));
#43065=DIRECTION('ref_axis',(-3.87506992302588E-15,3.31747701864093E-15,
-1.));
#43066=DIRECTION('',(1.,-5.0059604393446E-16,-3.87506992302588E-15));
#43067=DIRECTION('center_axis',(-1.,5.0059604393446E-16,3.87506992302588E-15));
#43068=DIRECTION('ref_axis',(-3.87506992302588E-15,3.31747701864093E-15,
-1.));
#43069=DIRECTION('center_axis',(1.,-5.0059604393446E-16,-3.87506992302588E-15));
#43070=DIRECTION('ref_axis',(-3.87506992302588E-15,3.31747701864093E-15,
-1.));
#43071=DIRECTION('center_axis',(1.,-5.0059604393446E-16,-3.87506992302588E-15));
#43072=DIRECTION('ref_axis',(-3.87506992302588E-15,3.31747701864093E-15,
-1.));
#43073=DIRECTION('',(1.,-5.0059604393446E-16,-3.87506992302588E-15));
#43074=DIRECTION('center_axis',(-1.,5.0059604393446E-16,3.87506992302588E-15));
#43075=DIRECTION('ref_axis',(-3.87506992302588E-15,3.31747701864093E-15,
-1.));
#43076=DIRECTION('center_axis',(1.,-5.0059604393446E-16,-3.87506992302588E-15));
#43077=DIRECTION('ref_axis',(-3.87506992302588E-15,3.31747701864093E-15,
-1.));
#43078=DIRECTION('center_axis',(1.,-5.0059604393446E-16,-3.87506992302588E-15));
#43079=DIRECTION('ref_axis',(-3.87506992302588E-15,3.31747701864093E-15,
-1.));
#43080=DIRECTION('',(1.,-5.0059604393446E-16,-3.87506992302588E-15));
#43081=DIRECTION('center_axis',(-1.,5.0059604393446E-16,3.87506992302588E-15));
#43082=DIRECTION('ref_axis',(-3.87506992302588E-15,3.31747701864093E-15,
-1.));
#43083=DIRECTION('center_axis',(1.,-5.0059604393446E-16,-3.87506992302588E-15));
#43084=DIRECTION('ref_axis',(-3.87506992302588E-15,3.31747701864093E-15,
-1.));
#43085=DIRECTION('center_axis',(1.,-5.0059604393446E-16,-3.87506992302588E-15));
#43086=DIRECTION('ref_axis',(-3.87506992302588E-15,3.31747701864093E-15,
-1.));
#43087=DIRECTION('',(1.,-5.0059604393446E-16,-3.87506992302588E-15));
#43088=DIRECTION('center_axis',(-1.,5.0059604393446E-16,3.87506992302588E-15));
#43089=DIRECTION('ref_axis',(-3.87506992302588E-15,3.31747701864093E-15,
-1.));
#43090=DIRECTION('center_axis',(1.,-5.0059604393446E-16,-3.87506992302588E-15));
#43091=DIRECTION('ref_axis',(-3.87506992302588E-15,3.31747701864093E-15,
-1.));
#43092=DIRECTION('center_axis',(1.,-5.0059604393446E-16,-3.87506992302588E-15));
#43093=DIRECTION('ref_axis',(-3.87506992302588E-15,3.31747701864093E-15,
-1.));
#43094=DIRECTION('',(1.,-5.0059604393446E-16,-3.87506992302588E-15));
#43095=DIRECTION('center_axis',(-1.,5.0059604393446E-16,3.87506992302588E-15));
#43096=DIRECTION('ref_axis',(-3.87506992302588E-15,3.31747701864093E-15,
-1.));
#43097=DIRECTION('center_axis',(-3.87506992302588E-15,3.64045098944098E-15,
-1.));
#43098=DIRECTION('ref_axis',(5.00596043934474E-16,1.,3.64045098944098E-15));
#43099=DIRECTION('',(5.00596043934474E-16,1.,3.64045098944098E-15));
#43100=DIRECTION('',(1.,-5.0059604393446E-16,-3.87506992302588E-15));
#43101=DIRECTION('',(5.00596043934474E-16,1.,3.64045098944098E-15));
#43102=DIRECTION('',(1.,-5.0059604393446E-16,-3.87506992302588E-15));
#43103=DIRECTION('center_axis',(-5.00596043934474E-16,-1.,-3.52646017621743E-15));
#43104=DIRECTION('ref_axis',(-3.87506992302588E-15,3.52646017621743E-15,
-1.));
#43105=DIRECTION('',(-3.87506992302588E-15,3.52646017621743E-15,-1.));
#43106=DIRECTION('',(-3.87506992302588E-15,3.52646017621743E-15,-1.));
#43107=DIRECTION('',(1.,-5.0059604393446E-16,-3.87506992302588E-15));
#43108=DIRECTION('center_axis',(3.87506992302588E-15,-3.60968124063133E-15,
1.));
#43109=DIRECTION('ref_axis',(-5.00596043934474E-16,-1.,-3.60968124063133E-15));
#43110=DIRECTION('',(-5.00596043934474E-16,-1.,-3.60968124063133E-15));
#43111=DIRECTION('',(-5.00596043934474E-16,-1.,-3.60968124063133E-15));
#43112=DIRECTION('',(1.,-5.0059604393446E-16,-3.87506992302588E-15));
#43113=DIRECTION('center_axis',(5.00596043934474E-16,1.,3.4742143868233E-15));
#43114=DIRECTION('ref_axis',(3.87506992302588E-15,-3.47421438682331E-15,
1.));
#43115=DIRECTION('',(3.87506992302588E-15,-3.47421438682331E-15,1.));
#43116=DIRECTION('',(3.87506992302588E-15,-3.47421438682331E-15,1.));
#43117=DIRECTION('center_axis',(1.,-5.0059604393446E-16,-3.87506992302588E-15));
#43118=DIRECTION('ref_axis',(-3.87506992302588E-15,3.31747701864093E-15,
-1.));
#43119=DIRECTION('center_axis',(1.,-5.0059604393446E-16,-3.87506992302588E-15));
#43120=DIRECTION('ref_axis',(-3.87506992302588E-15,3.31747701864093E-15,
-1.));
#43121=DIRECTION('axis',(0.,0.,1.));
#43122=DIRECTION('refdir',(1.,0.,0.));
#43123=DIRECTION('center_axis',(-1.,-5.4480841862383E-16,3.82282413363175E-15));
#43124=DIRECTION('ref_axis',(-3.82282413363175E-15,3.2203325039861E-15,
-1.));
#43125=DIRECTION('',(3.82282413363175E-15,-3.2203325039861E-15,1.));
#43126=DIRECTION('',(5.44808418623818E-16,-1.,-3.2203325039861E-15));
#43127=DIRECTION('',(-3.82282413363175E-15,3.2203325039861E-15,-1.));
#43128=DIRECTION('',(-5.44808418623818E-16,1.,3.2203325039861E-15));
#43129=DIRECTION('center_axis',(-3.82282413363175E-15,3.2203325039861E-15,
-1.));
#43130=DIRECTION('ref_axis',(5.44808418623818E-16,-1.,-3.2203325039861E-15));
#43131=DIRECTION('',(-1.,-5.4480841862383E-16,3.82282413363175E-15));
#43132=DIRECTION('',(-5.44808418623818E-16,1.,3.2203325039861E-15));
#43133=DIRECTION('',(1.,5.4480841862383E-16,-3.82282413363175E-15));
#43134=DIRECTION('center_axis',(-5.44808418623818E-16,1.,3.2203325039861E-15));
#43135=DIRECTION('ref_axis',(1.,5.4480841862383E-16,-3.82282413363175E-15));
#43136=DIRECTION('',(-1.,-5.4480841862383E-16,3.82282413363175E-15));
#43137=DIRECTION('',(0.707106781186545,2.66235667850046E-15,-0.70710678118655));
#43138=DIRECTION('',(-3.82282413363175E-15,3.2203325039861E-15,-1.));
#43139=DIRECTION('center_axis',(5.44808418623818E-16,-1.,-3.2203325039861E-15));
#43140=DIRECTION('ref_axis',(3.82282413363175E-15,-3.2203325039861E-15,
1.));
#43141=DIRECTION('',(-3.82282413363175E-15,3.2203325039861E-15,-1.));
#43142=DIRECTION('',(-0.70710678118655,1.8918812239876E-15,-0.707106781186545));
#43143=DIRECTION('center_axis',(5.44808418623818E-16,-1.,-3.2203325039861E-15));
#43144=DIRECTION('ref_axis',(3.82282413363175E-15,-3.2203325039861E-15,
1.));
#43145=DIRECTION('',(5.44808418623818E-16,-1.,-3.2203325039861E-15));
#43146=DIRECTION('',(-5.44808418623818E-16,1.,3.2203325039861E-15));
#43147=DIRECTION('center_axis',(-5.44808418623818E-16,1.,3.2203325039861E-15));
#43148=DIRECTION('ref_axis',(3.82282413363175E-15,-3.2203325039861E-15,
1.));
#43149=DIRECTION('center_axis',(5.44808418623818E-16,-1.,-3.2203325039861E-15));
#43150=DIRECTION('ref_axis',(-1.,-5.4480841862383E-16,3.82282413363175E-15));
#43151=DIRECTION('',(0.70710678118655,-1.8918812239876E-15,0.707106781186545));
#43152=DIRECTION('',(3.82282413363175E-15,-3.2203325039861E-15,1.));
#43153=DIRECTION('',(3.82282413363175E-15,-3.2203325039861E-15,1.));
#43154=DIRECTION('',(-0.707106781186545,-2.66235667850046E-15,0.70710678118655));
#43155=DIRECTION('',(1.,5.4480841862383E-16,-3.82282413363175E-15));
#43156=DIRECTION('center_axis',(-1.,-5.4480841862383E-16,3.82282413363175E-15));
#43157=DIRECTION('ref_axis',(3.82282413363175E-15,-3.2203325039861E-15,
1.));
#43158=DIRECTION('',(-5.44808418623818E-16,1.,3.2203325039861E-15));
#43159=DIRECTION('center_axis',(-1.,-5.4480841862383E-16,3.82282413363175E-15));
#43160=DIRECTION('ref_axis',(3.82282413363175E-15,-3.2203325039861E-15,
1.));
#43161=DIRECTION('',(5.44808418623818E-16,-1.,-3.2203325039861E-15));
#43162=DIRECTION('center_axis',(-0.70710678118655,1.8918812239876E-15,-0.707106781186545));
#43163=DIRECTION('ref_axis',(5.44808418623818E-16,-1.,-3.2203325039861E-15));
#43164=DIRECTION('',(5.44808418623818E-16,-1.,-3.2203325039861E-15));
#43165=DIRECTION('center_axis',(-0.707106781186545,-2.66235667850046E-15,
0.70710678118655));
#43166=DIRECTION('ref_axis',(-5.44808418623818E-16,1.,3.2203325039861E-15));
#43167=DIRECTION('center_axis',(-3.82282413363175E-15,3.2203325039861E-15,
-1.));
#43168=DIRECTION('ref_axis',(5.44808418623818E-16,-1.,-3.2203325039861E-15));
#43169=DIRECTION('axis',(0.,0.,1.));
#43170=DIRECTION('refdir',(1.,0.,0.));
#43171=DIRECTION('center_axis',(3.34404360992195E-15,-7.77119338241478E-16,
1.));
#43172=DIRECTION('ref_axis',(-1.67529136546934E-16,-1.,-7.77119338241477E-16));
#43173=DIRECTION('center_axis',(3.34404360992195E-15,-7.77119338241478E-16,
1.));
#43174=DIRECTION('ref_axis',(-1.67529136546934E-16,-1.,-7.77119338241477E-16));
#43175=DIRECTION('',(3.34404360992195E-15,-7.77119338241478E-16,1.));
#43176=DIRECTION('center_axis',(-3.34404360992195E-15,7.77119338241478E-16,
-1.));
#43177=DIRECTION('ref_axis',(-1.67529136546934E-16,-1.,-7.77119338241477E-16));
#43178=DIRECTION('center_axis',(3.34404360992195E-15,-7.77119338241478E-16,
1.));
#43179=DIRECTION('ref_axis',(-1.67529136546934E-16,-1.,-7.77119338241477E-16));
#43180=DIRECTION('center_axis',(3.34404360992195E-15,-7.77119338241478E-16,
1.));
#43181=DIRECTION('ref_axis',(-1.67529136546934E-16,-1.,-7.77119338241477E-16));
#43182=DIRECTION('',(3.34404360992195E-15,-7.77119338241478E-16,1.));
#43183=DIRECTION('center_axis',(-3.34404360992195E-15,7.77119338241478E-16,
-1.));
#43184=DIRECTION('ref_axis',(-1.67529136546934E-16,-1.,-7.77119338241477E-16));
#43185=DIRECTION('center_axis',(3.34404360992195E-15,-7.77119338241478E-16,
1.));
#43186=DIRECTION('ref_axis',(-1.67529136546934E-16,-1.,-7.77119338241477E-16));
#43187=DIRECTION('center_axis',(3.34404360992195E-15,-7.77119338241478E-16,
1.));
#43188=DIRECTION('ref_axis',(-1.67529136546934E-16,-1.,-7.77119338241477E-16));
#43189=DIRECTION('',(3.34404360992195E-15,-7.77119338241478E-16,1.));
#43190=DIRECTION('center_axis',(-3.34404360992195E-15,7.77119338241478E-16,
-1.));
#43191=DIRECTION('ref_axis',(-1.67529136546934E-16,-1.,-7.77119338241477E-16));
#43192=DIRECTION('center_axis',(3.34404360992195E-15,-7.77119338241478E-16,
1.));
#43193=DIRECTION('ref_axis',(-1.67529136546934E-16,-1.,-7.77119338241477E-16));
#43194=DIRECTION('center_axis',(3.34404360992195E-15,-7.77119338241478E-16,
1.));
#43195=DIRECTION('ref_axis',(-1.67529136546934E-16,-1.,-7.77119338241477E-16));
#43196=DIRECTION('',(3.34404360992195E-15,-7.77119338241478E-16,1.));
#43197=DIRECTION('center_axis',(-3.34404360992195E-15,7.77119338241478E-16,
-1.));
#43198=DIRECTION('ref_axis',(-1.67529136546934E-16,-1.,-7.77119338241477E-16));
#43199=DIRECTION('center_axis',(-1.67529136546934E-16,-1.,-7.77119338241477E-16));
#43200=DIRECTION('ref_axis',(-1.,1.67529136546931E-16,3.34404360992195E-15));
#43201=DIRECTION('',(-1.,1.67529136546931E-16,3.34404360992195E-15));
#43202=DIRECTION('',(-3.34404360992195E-15,7.77119338241478E-16,-1.));
#43203=DIRECTION('',(1.,-1.67529136546931E-16,-3.34404360992195E-15));
#43204=DIRECTION('',(-3.34404360992195E-15,7.77119338241478E-16,-1.));
#43205=DIRECTION('center_axis',(1.,-1.67529136546931E-16,-3.34404360992195E-15));
#43206=DIRECTION('ref_axis',(-1.67529136546934E-16,-1.,-7.77119338241477E-16));
#43207=DIRECTION('',(-1.67529136546934E-16,-1.,-7.77119338241477E-16));
#43208=DIRECTION('',(-3.34404360992195E-15,7.77119338241478E-16,-1.));
#43209=DIRECTION('',(1.67529136546934E-16,1.,7.77119338241477E-16));
#43210=DIRECTION('center_axis',(1.67529136546934E-16,1.,7.77119338241477E-16));
#43211=DIRECTION('ref_axis',(1.,-1.67529136546931E-16,-3.34404360992195E-15));
#43212=DIRECTION('',(1.,-1.67529136546931E-16,-3.34404360992195E-15));
#43213=DIRECTION('',(-3.34404360992195E-15,7.77119338241478E-16,-1.));
#43214=DIRECTION('',(-1.,1.67529136546931E-16,3.34404360992195E-15));
#43215=DIRECTION('center_axis',(-1.,1.67529136546931E-16,3.34404360992195E-15));
#43216=DIRECTION('ref_axis',(1.67529136546934E-16,1.,7.77119338241477E-16));
#43217=DIRECTION('',(1.67529136546934E-16,1.,7.77119338241477E-16));
#43218=DIRECTION('',(-1.67529136546934E-16,-1.,-7.77119338241477E-16));
#43219=DIRECTION('center_axis',(-1.67529136546934E-16,-1.,-7.77119338241477E-16));
#43220=DIRECTION('ref_axis',(-1.,1.67529136546931E-16,3.34404360992195E-15));
#43221=DIRECTION('',(-1.,1.67529136546931E-16,3.34404360992195E-15));
#43222=DIRECTION('',(-3.34404360992195E-15,7.77119338241478E-16,-1.));
#43223=DIRECTION('',(-1.,1.67529136546931E-16,3.34404360992195E-15));
#43224=DIRECTION('',(-3.34404360992195E-15,7.77119338241478E-16,-1.));
#43225=DIRECTION('center_axis',(1.,-1.67529136546931E-16,-3.34404360992195E-15));
#43226=DIRECTION('ref_axis',(-1.67529136546934E-16,-1.,-7.77119338241477E-16));
#43227=DIRECTION('',(-1.67529136546934E-16,-1.,-7.77119338241477E-16));
#43228=DIRECTION('',(-1.67529136546934E-16,-1.,-7.77119338241477E-16));
#43229=DIRECTION('',(-3.34404360992195E-15,7.77119338241478E-16,-1.));
#43230=DIRECTION('center_axis',(1.67529136546934E-16,1.,7.77119338241477E-16));
#43231=DIRECTION('ref_axis',(1.,-1.67529136546931E-16,-3.34404360992195E-15));
#43232=DIRECTION('',(1.,-1.67529136546931E-16,-3.34404360992195E-15));
#43233=DIRECTION('',(1.,-1.67529136546931E-16,-3.34404360992195E-15));
#43234=DIRECTION('',(-3.34404360992195E-15,7.77119338241478E-16,-1.));
#43235=DIRECTION('center_axis',(-1.,1.67529136546931E-16,3.34404360992195E-15));
#43236=DIRECTION('ref_axis',(1.67529136546934E-16,1.,7.77119338241477E-16));
#43237=DIRECTION('',(1.67529136546934E-16,1.,7.77119338241477E-16));
#43238=DIRECTION('',(1.67529136546934E-16,1.,7.77119338241477E-16));
#43239=DIRECTION('center_axis',(-3.34404360992195E-15,7.77119338241478E-16,
-1.));
#43240=DIRECTION('ref_axis',(1.67529136546934E-16,1.,7.77119338241477E-16));
#43241=DIRECTION('center_axis',(-3.34404360992195E-15,7.77119338241478E-16,
-1.));
#43242=DIRECTION('ref_axis',(1.67529136546934E-16,1.,7.77119338241477E-16));
#43243=DIRECTION('',(0.,0.,1.));
#43244=DIRECTION('',(1.,0.,0.));
#43245=DIRECTION('',(0.,0.,1.));
#43246=DIRECTION('',(1.,0.,0.));
#43247=DIRECTION('',(0.,0.,1.));
#43248=DIRECTION('',(1.,0.,0.));
#43249=DIRECTION('',(0.,0.,1.));
#43250=DIRECTION('',(1.,0.,0.));
#43251=DIRECTION('',(1.33717928332814E-15,1.43391950699461E-15,1.));
#43252=DIRECTION('',(1.,1.01565841547205E-29,-1.33717928332814E-15));
#43253=DIRECTION('',(0.,0.,1.));
#43254=DIRECTION('',(1.,0.,0.));
#43255=DIRECTION('',(0.,0.,1.));
#43256=DIRECTION('',(1.,1.51868295214834E-32,0.));
#43257=DIRECTION('',(0.,0.,1.));
#43258=DIRECTION('',(1.,1.51868295214834E-32,0.));
#43259=DIRECTION('',(0.,0.,1.));
#43260=DIRECTION('',(1.,1.51868295214834E-32,0.));
#43261=DIRECTION('',(0.,0.,1.));
#43262=DIRECTION('',(1.,1.51868295214834E-32,0.));
#43263=DIRECTION('',(1.01290306638139E-16,6.53780952262704E-15,-1.));
#43264=DIRECTION('',(-1.,-3.17792651283334E-16,-1.0129030663814E-16));
#43265=DIRECTION('',(1.01290306638139E-16,6.53780952262704E-15,-1.));
#43266=DIRECTION('',(-1.,-3.17792651283334E-16,-1.0129030663814E-16));
#43267=DIRECTION('',(1.01290306638139E-16,6.53780952262704E-15,-1.));
#43268=DIRECTION('',(-1.,-3.17792651283334E-16,-1.0129030663814E-16));
#43269=DIRECTION('',(1.01290306638139E-16,6.53780952262704E-15,-1.));
#43270=DIRECTION('',(-1.,-3.17792651283334E-16,-1.0129030663814E-16));
#43271=DIRECTION('',(1.01290306638139E-16,6.53780952262704E-15,-1.));
#43272=DIRECTION('',(-1.,-3.17792651283334E-16,-1.0129030663814E-16));
#43273=DIRECTION('',(0.,0.,1.));
#43274=DIRECTION('',(1.,0.,0.));
#43275=DIRECTION('axis',(0.,0.,1.));
#43276=DIRECTION('refdir',(1.,0.,0.));
#43277=DIRECTION('axis',(0.,0.,1.));
#43278=DIRECTION('refdir',(1.,0.,0.));
#43279=DIRECTION('center_axis',(4.88578146679885E-16,1.,-9.3381869947186E-16));
#43280=DIRECTION('ref_axis',(1.,-4.8857814667989E-16,-5.46077161851014E-15));
#43281=DIRECTION('',(-4.88578146679885E-16,-1.,9.3381869947186E-16));
#43282=DIRECTION('center_axis',(4.88578146679885E-16,1.,-9.3381869947186E-16));
#43283=DIRECTION('ref_axis',(5.46077161851014E-15,9.33818699471857E-16,
1.));
#43284=DIRECTION('',(-4.88578146679885E-16,-1.,9.3381869947186E-16));
#43285=DIRECTION('center_axis',(4.88578146679885E-16,1.,-9.3381869947186E-16));
#43286=DIRECTION('ref_axis',(5.46077161851014E-15,9.33818699471857E-16,
1.));
#43287=DIRECTION('center_axis',(-1.,4.8857814667989E-16,5.46077161851014E-15));
#43288=DIRECTION('ref_axis',(4.88578146679884E-16,1.,-1.0562833793866E-15));
#43289=DIRECTION('',(-1.,4.8857814667989E-16,5.46077161851014E-15));
#43290=DIRECTION('center_axis',(-1.,4.8857814667989E-16,5.46077161851014E-15));
#43291=DIRECTION('ref_axis',(-4.88578146679885E-16,-1.,9.3381869947186E-16));
#43292=DIRECTION('',(-1.,4.8857814667989E-16,5.46077161851014E-15));
#43293=DIRECTION('center_axis',(-5.46077161851014E-15,-1.34090047516775E-15,
-1.));
#43294=DIRECTION('ref_axis',(-4.88578146679883E-16,-1.,1.34090047516775E-15));
#43295=DIRECTION('',(-4.88578146679885E-16,-1.,9.3381869947186E-16));
#43296=DIRECTION('',(-4.88578146679883E-16,-1.,1.34090047516775E-15));
#43297=DIRECTION('',(-1.,4.8857814667989E-16,5.46077161851014E-15));
#43298=DIRECTION('center_axis',(5.46077161851014E-15,1.2668856068594E-15,
1.));
#43299=DIRECTION('ref_axis',(4.88578146679883E-16,1.,-1.26688560685941E-15));
#43300=DIRECTION('',(4.88578146679885E-16,1.,-9.3381869947186E-16));
#43301=DIRECTION('',(-1.,4.8857814667989E-16,5.46077161851014E-15));
#43302=DIRECTION('',(4.88578146679883E-16,1.,-1.26688560685941E-15));
#43303=DIRECTION('center_axis',(-1.,4.8857814667989E-16,5.46077161851014E-15));
#43304=DIRECTION('ref_axis',(-4.88578146679885E-16,-1.,9.3381869947186E-16));
#43305=DIRECTION('center_axis',(-1.,4.8857814667989E-16,5.46077161851014E-15));
#43306=DIRECTION('ref_axis',(-4.88578146679885E-16,-1.,9.3381869947186E-16));
#43307=DIRECTION('center_axis',(-1.,4.14563278371546E-16,5.46077161851014E-15));
#43308=DIRECTION('ref_axis',(5.46077161851014E-15,9.33818699471857E-16,
1.));
#43309=DIRECTION('center_axis',(4.88578146679885E-16,1.,-9.3381869947186E-16));
#43310=DIRECTION('ref_axis',(3.5527136788005E-15,8.88178419700125E-16,1.));
#43311=DIRECTION('center_axis',(-4.88578146679885E-16,-1.,9.3381869947186E-16));
#43312=DIRECTION('ref_axis',(-1.,4.8857814667989E-16,5.27707459863804E-15));
#43313=DIRECTION('center_axis',(-4.88578146679885E-16,-1.,9.3381869947186E-16));
#43314=DIRECTION('ref_axis',(-1.,4.8857814667989E-16,5.27707459863804E-15));
#43315=DIRECTION('center_axis',(1.,-4.88578146679891E-16,-6.66133814775093E-15));
#43316=DIRECTION('ref_axis',(-6.66133814775093E-15,-1.11022302462516E-15,
-1.));
#43317=DIRECTION('center_axis',(4.88578146679885E-16,1.,-9.3381869947186E-16));
#43318=DIRECTION('ref_axis',(-1.,4.8857814667989E-16,5.27707459863804E-15));
#43319=DIRECTION('center_axis',(4.88578146679885E-16,1.,-9.3381869947186E-16));
#43320=DIRECTION('ref_axis',(5.46077161851014E-15,9.33818699471857E-16,
1.));
#43321=DIRECTION('center_axis',(-4.88578146679885E-16,-1.,9.3381869947186E-16));
#43322=DIRECTION('ref_axis',(-1.,4.8857814667989E-16,5.46077161851014E-15));
#43323=DIRECTION('center_axis',(4.88578146679885E-16,1.,-9.3381869947186E-16));
#43324=DIRECTION('ref_axis',(1.,-4.8857814667989E-16,-5.46077161851014E-15));
#43325=DIRECTION('center_axis',(4.88578146679885E-16,1.,-9.3381869947186E-16));
#43326=DIRECTION('ref_axis',(5.46077161851014E-15,9.33818699471857E-16,
1.));
#43327=DIRECTION('',(-4.88578146679885E-16,-1.,9.3381869947186E-16));
#43328=DIRECTION('center_axis',(4.88578146679885E-16,1.,-9.3381869947186E-16));
#43329=DIRECTION('ref_axis',(3.5527136788005E-15,0.,1.));
#43330=DIRECTION('center_axis',(-4.88578146679885E-16,-1.,9.3381869947186E-16));
#43331=DIRECTION('ref_axis',(-1.,4.8857814667989E-16,5.27707459863804E-15));
#43332=DIRECTION('center_axis',(1.,-4.88578146679891E-16,-6.66133814775093E-15));
#43333=DIRECTION('ref_axis',(-6.66133814775093E-15,0.,-1.));
#43334=DIRECTION('center_axis',(4.88578146679885E-16,1.,-9.3381869947186E-16));
#43335=DIRECTION('ref_axis',(-1.,4.8857814667989E-16,5.27707459863804E-15));
#43336=DIRECTION('center_axis',(4.88578146679885E-16,1.,-9.3381869947186E-16));
#43337=DIRECTION('ref_axis',(-1.,4.8857814667989E-16,5.27707459863804E-15));
#43338=DIRECTION('center_axis',(-4.88578146679885E-16,-1.,9.3381869947186E-16));
#43339=DIRECTION('ref_axis',(-5.46077161851014E-15,-9.33818699471857E-16,
-1.));
#43340=DIRECTION('center_axis',(4.88578146679885E-16,1.,-9.3381869947186E-16));
#43341=DIRECTION('ref_axis',(-1.,4.8857814667989E-16,5.46077161851014E-15));
#43342=DIRECTION('center_axis',(4.88578146679885E-16,1.,-9.3381869947186E-16));
#43343=DIRECTION('ref_axis',(1.,-4.8857814667989E-16,-5.46077161851014E-15));
#43344=DIRECTION('',(-4.88578146679885E-16,-1.,9.3381869947186E-16));
#43345=DIRECTION('center_axis',(-4.88578146679885E-16,-1.,9.3381869947186E-16));
#43346=DIRECTION('ref_axis',(-1.,4.8857814667989E-16,5.46077161851014E-15));
#43347=DIRECTION('center_axis',(-4.88578146679885E-16,-1.,9.3381869947186E-16));
#43348=DIRECTION('ref_axis',(-1.,4.8857814667989E-16,5.46077161851014E-15));
#43349=DIRECTION('center_axis',(4.88578146679885E-16,1.,-9.3381869947186E-16));
#43350=DIRECTION('ref_axis',(-1.,4.8857814667989E-16,5.46077161851014E-15));
#43351=DIRECTION('center_axis',(-4.88578146679885E-16,-1.,9.3381869947186E-16));
#43352=DIRECTION('ref_axis',(-1.,4.8857814667989E-16,5.46077161851014E-15));
#43353=DIRECTION('center_axis',(-4.88578146679885E-16,-1.,9.3381869947186E-16));
#43354=DIRECTION('ref_axis',(-1.,4.8857814667989E-16,5.46077161851014E-15));
#43355=DIRECTION('',(-0.707106781186532,-0.707106781186563,4.60825378237839E-15));
#43356=DIRECTION('center_axis',(4.88578146679885E-16,1.,-9.3381869947186E-16));
#43357=DIRECTION('ref_axis',(1.,-4.8857814667989E-16,-5.46077161851014E-15));
#43358=DIRECTION('center_axis',(4.88578146679885E-16,1.,-9.3381869947186E-16));
#43359=DIRECTION('ref_axis',(5.46077161851014E-15,9.33818699471857E-16,
1.));
#43360=DIRECTION('',(-4.88578146679885E-16,-1.,9.3381869947186E-16));
#43361=DIRECTION('center_axis',(4.88578146679885E-16,1.,-9.3381869947186E-16));
#43362=DIRECTION('ref_axis',(5.46077161851014E-15,9.33818699471857E-16,
1.));
#43363=DIRECTION('center_axis',(-4.88578146679885E-16,-1.,9.3381869947186E-16));
#43364=DIRECTION('ref_axis',(-1.,4.8857814667989E-16,5.46077161851014E-15));
#43365=DIRECTION('center_axis',(4.88578146679885E-16,1.,-9.3381869947186E-16));
#43366=DIRECTION('ref_axis',(-1.,4.8857814667989E-16,5.46077161851014E-15));
#43367=DIRECTION('center_axis',(4.88578146679885E-16,1.,-9.3381869947186E-16));
#43368=DIRECTION('ref_axis',(-1.,4.8857814667989E-16,5.46077161851014E-15));
#43369=DIRECTION('',(-0.707106781186548,0.707106781186547,3.11444350154066E-15));
#43370=DIRECTION('center_axis',(4.88578146679885E-16,1.,-9.3381869947186E-16));
#43371=DIRECTION('ref_axis',(1.,-4.8857814667989E-16,-5.46077161851014E-15));
#43372=DIRECTION('',(-4.88578146679885E-16,-1.,9.3381869947186E-16));
#43373=DIRECTION('center_axis',(4.88578146679885E-16,1.,-9.3381869947186E-16));
#43374=DIRECTION('ref_axis',(5.46077161851014E-15,9.33818699471857E-16,
1.));
#43375=DIRECTION('center_axis',(4.88578146679885E-16,1.,-9.3381869947186E-16));
#43376=DIRECTION('ref_axis',(5.46077161851014E-15,9.33818699471857E-16,
1.));
#43377=DIRECTION('center_axis',(4.88578146679885E-16,1.,-9.3381869947186E-16));
#43378=DIRECTION('ref_axis',(-1.,4.8857814667989E-16,5.46077161851014E-15));
#43379=DIRECTION('',(-0.707106781186543,-0.707106781186552,4.60825378237844E-15));
#43380=DIRECTION('center_axis',(4.88578146679885E-16,1.,-9.3381869947186E-16));
#43381=DIRECTION('ref_axis',(-1.,4.8857814667989E-16,5.46077161851014E-15));
#43382=DIRECTION('center_axis',(-4.88578146679885E-16,-1.,9.3381869947186E-16));
#43383=DIRECTION('ref_axis',(-5.46077161851014E-15,-9.33818699471857E-16,
-1.));
#43384=DIRECTION('center_axis',(-1.,4.8857814667989E-16,5.46077161851014E-15));
#43385=DIRECTION('ref_axis',(5.46077161851014E-15,9.33818699471857E-16,
1.));
#43386=DIRECTION('',(-1.,4.8857814667989E-16,5.46077161851014E-15));
#43387=DIRECTION('center_axis',(-1.,4.8857814667989E-16,5.46077161851014E-15));
#43388=DIRECTION('ref_axis',(5.46077161851014E-15,9.33818699471857E-16,
1.));
#43389=DIRECTION('',(-1.,4.8857814667989E-16,5.46077161851014E-15));
#43390=DIRECTION('center_axis',(5.46077161851014E-15,9.33818699471857E-16,
1.));
#43391=DIRECTION('ref_axis',(4.88578146679885E-16,1.,-9.3381869947186E-16));
#43392=DIRECTION('',(4.88578146679885E-16,1.,-9.3381869947186E-16));
#43393=DIRECTION('',(4.88578146679885E-16,1.,-9.3381869947186E-16));
#43394=DIRECTION('',(-1.,4.8857814667989E-16,5.46077161851014E-15));
#43395=DIRECTION('center_axis',(-5.46077161851014E-15,-9.33818699471857E-16,
-1.));
#43396=DIRECTION('ref_axis',(-4.88578146679885E-16,-1.,9.3381869947186E-16));
#43397=DIRECTION('',(-1.,4.8857814667989E-16,5.46077161851014E-15));
#43398=DIRECTION('',(-4.88578146679885E-16,-1.,9.3381869947186E-16));
#43399=DIRECTION('center_axis',(-1.,4.8857814667989E-16,5.46077161851014E-15));
#43400=DIRECTION('ref_axis',(-5.46077161851014E-15,-9.33818699471857E-16,
-1.));
#43401=DIRECTION('center_axis',(-1.,4.8857814667989E-16,5.46077161851014E-15));
#43402=DIRECTION('ref_axis',(-5.46077161851014E-15,-9.33818699471857E-16,
-1.));
#43403=DIRECTION('center_axis',(1.,-4.8857814667989E-16,-5.46077161851014E-15));
#43404=DIRECTION('ref_axis',(-5.46077161851014E-15,-9.33818699471857E-16,
-1.));
#43405=DIRECTION('center_axis',(4.88578146679885E-16,1.,-9.3381869947186E-16));
#43406=DIRECTION('ref_axis',(1.,-4.8857814667989E-16,-5.46077161851014E-15));
#43407=DIRECTION('center_axis',(4.88578146679885E-16,1.,-9.3381869947186E-16));
#43408=DIRECTION('ref_axis',(5.46077161851014E-15,9.33818699471857E-16,
1.));
#43409=DIRECTION('center_axis',(4.88578146679885E-16,1.,-9.3381869947186E-16));
#43410=DIRECTION('ref_axis',(5.46077161851014E-15,9.33818699471857E-16,
1.));
#43411=DIRECTION('center_axis',(-4.88578146679885E-16,-1.,9.3381869947186E-16));
#43412=DIRECTION('ref_axis',(1.,-4.8857814667989E-16,-5.46077161851014E-15));
#43413=DIRECTION('',(0.707106781186543,0.707106781186552,-4.43506257113134E-15));
#43414=DIRECTION('center_axis',(4.88578146679885E-16,1.,-9.3381869947186E-16));
#43415=DIRECTION('ref_axis',(5.46077161851014E-15,9.33818699471857E-16,
1.));
#43416=DIRECTION('center_axis',(4.88578146679885E-16,1.,-9.3381869947186E-16));
#43417=DIRECTION('ref_axis',(5.46077161851014E-15,9.33818699471857E-16,
1.));
#43418=DIRECTION('center_axis',(4.88578146679885E-16,1.,-9.3381869947186E-16));
#43419=DIRECTION('ref_axis',(5.83009424213414E-15,1.45752356053353E-15,
1.));
#43420=DIRECTION('center_axis',(4.88578146679885E-16,1.,-9.3381869947186E-16));
#43421=DIRECTION('ref_axis',(5.46077161851014E-15,9.33818699471858E-16,
1.));
#43422=DIRECTION('center_axis',(1.,-4.8857814667989E-16,-5.46571335200076E-15));
#43423=DIRECTION('ref_axis',(-5.46571335200076E-15,-1.82190445066692E-15,
-1.));
#43424=DIRECTION('center_axis',(-4.88578146679885E-16,-1.,9.3381869947186E-16));
#43425=DIRECTION('ref_axis',(-5.46077161851014E-15,-9.33818699471857E-16,
-1.));
#43426=DIRECTION('center_axis',(4.88578146679885E-16,1.,-9.3381869947186E-16));
#43427=DIRECTION('ref_axis',(5.46077161851014E-15,9.33818699471857E-16,
1.));
#43428=DIRECTION('center_axis',(4.88578146679885E-16,1.,-9.3381869947186E-16));
#43429=DIRECTION('ref_axis',(1.,-4.8857814667989E-16,-5.46077161851014E-15));
#43430=DIRECTION('',(0.707106781186548,-0.707106781186547,-3.28763471278776E-15));
#43431=DIRECTION('center_axis',(-4.88578146679885E-16,-1.,9.3381869947186E-16));
#43432=DIRECTION('ref_axis',(1.,-4.8857814667989E-16,-5.46077161851014E-15));
#43433=DIRECTION('',(0.707106781186549,0.707106781186546,-4.43506257113137E-15));
#43434=DIRECTION('center_axis',(4.88578146679885E-16,1.,-9.3381869947186E-16));
#43435=DIRECTION('ref_axis',(5.46077161851014E-15,9.33818699471857E-16,
1.));
#43436=DIRECTION('center_axis',(4.88578146679885E-16,1.,-9.3381869947186E-16));
#43437=DIRECTION('ref_axis',(5.46077161851014E-15,9.33818699471857E-16,
1.));
#43438=DIRECTION('center_axis',(4.88578146679885E-16,1.,-9.3381869947186E-16));
#43439=DIRECTION('ref_axis',(5.46077161851014E-15,9.33818699471858E-16,
1.));
#43440=DIRECTION('center_axis',(4.88578146679885E-16,1.,-9.3381869947186E-16));
#43441=DIRECTION('ref_axis',(5.83009424213416E-15,7.28761780266769E-16,
1.));
#43442=DIRECTION('center_axis',(1.,-4.8857814667989E-16,-5.46571335200076E-15));
#43443=DIRECTION('ref_axis',(-5.46571335200076E-15,-9.10952225333461E-16,
-1.));
#43444=DIRECTION('axis',(0.,0.,1.));
#43445=DIRECTION('refdir',(1.,0.,0.));
#43446=DIRECTION('center_axis',(4.88578148594761E-16,1.,1.17579033359749E-15));
#43447=DIRECTION('ref_axis',(0.0779446090567885,1.13413118345969E-15,-0.996957691137886));
#43448=DIRECTION('',(-4.88578148594761E-16,-1.,-1.17579033359749E-15));
#43449=DIRECTION('center_axis',(4.88578148594761E-16,1.,1.17579033359749E-15));
#43450=DIRECTION('ref_axis',(0.996957691137886,-5.78738260848463E-16,0.0779446090567885));
#43451=DIRECTION('',(-4.88578148594761E-16,-1.,-1.17579033359749E-15));
#43452=DIRECTION('center_axis',(4.88578148594761E-16,1.,1.17579033359749E-15));
#43453=DIRECTION('ref_axis',(0.996957691137886,-5.78738260848463E-16,0.0779446090567885));
#43454=DIRECTION('center_axis',(-4.88578148594761E-16,-1.,-1.17579033359749E-15));
#43455=DIRECTION('ref_axis',(-0.0779446090567885,-1.13413118345969E-15,
0.996957691137886));
#43456=DIRECTION('center_axis',(4.88578148594761E-16,1.,1.17579033359749E-15));
#43457=DIRECTION('ref_axis',(-0.0779446090567885,-1.13413118345969E-15,
0.996957691137886));
#43458=DIRECTION('center_axis',(4.88578148594761E-16,1.,1.17579033359749E-15));
#43459=DIRECTION('ref_axis',(-0.0779446090567885,-1.13413118345969E-15,
0.996957691137886));
#43460=DIRECTION('',(-0.0551151616209882,0.70710678118656,0.70495554395967));
#43461=DIRECTION('center_axis',(-4.88578148594761E-16,-1.,-1.17579033359749E-15));
#43462=DIRECTION('ref_axis',(-0.0779446090567885,-1.13413118345969E-15,
0.996957691137886));
#43463=DIRECTION('center_axis',(4.88578148594761E-16,1.,1.17579033359749E-15));
#43464=DIRECTION('ref_axis',(0.0779446090567885,1.13413118345969E-15,-0.996957691137886));
#43465=DIRECTION('',(-4.88578148594761E-16,-1.,-1.17579033359749E-15));
#43466=DIRECTION('center_axis',(4.88578148594761E-16,1.,1.17579033359749E-15));
#43467=DIRECTION('ref_axis',(0.996957691137886,-5.78738260848462E-16,0.0779446090567885));
#43468=DIRECTION('',(-4.88578148594761E-16,-1.,-1.17579033359749E-15));
#43469=DIRECTION('',(4.88578148594761E-16,1.,1.17579033359749E-15));
#43470=DIRECTION('center_axis',(4.88578148594761E-16,1.,1.17579033359749E-15));
#43471=DIRECTION('ref_axis',(0.996957691137886,-5.78738260848462E-16,0.0779446090567885));
#43472=DIRECTION('center_axis',(-4.88578148594761E-16,-1.,-1.17579033359749E-15));
#43473=DIRECTION('ref_axis',(-0.0779446090567885,-1.13413118345969E-15,
0.996957691137886));
#43474=DIRECTION('center_axis',(4.88578148594761E-16,1.,1.17579033359749E-15));
#43475=DIRECTION('ref_axis',(-0.0779446090567885,-1.13413118345969E-15,
0.996957691137886));
#43476=DIRECTION('center_axis',(4.88578148594761E-16,1.,1.17579033359749E-15));
#43477=DIRECTION('ref_axis',(-0.0779446090567885,-1.13413118345969E-15,
0.996957691137886));
#43478=DIRECTION('',(-0.0551151616209889,0.707106781186552,0.704955543959679));
#43479=DIRECTION('center_axis',(-4.88578148594761E-16,-1.,-1.17579033359749E-15));
#43480=DIRECTION('ref_axis',(-0.0779446090567885,-1.13413118345969E-15,
0.996957691137886));
#43481=DIRECTION('center_axis',(4.88578148594761E-16,1.,1.17579033359749E-15));
#43482=DIRECTION('ref_axis',(0.0779446090567885,1.13413118345969E-15,-0.996957691137886));
#43483=DIRECTION('',(-4.88578148594761E-16,-1.,-1.17579033359749E-15));
#43484=DIRECTION('center_axis',(-4.88578148594761E-16,-1.,-1.17579033359749E-15));
#43485=DIRECTION('ref_axis',(-0.0779446090567887,-1.13413118345969E-15,
0.996957691137886));
#43486=DIRECTION('center_axis',(-4.88578148594761E-16,-1.,-1.17579033359749E-15));
#43487=DIRECTION('ref_axis',(-0.0779446090567887,-1.13413118345969E-15,
0.996957691137886));
#43488=DIRECTION('center_axis',(4.88578148594761E-16,1.,1.17579033359749E-15));
#43489=DIRECTION('ref_axis',(0.996957691137886,-5.78738260848462E-16,0.0779446090567885));
#43490=DIRECTION('center_axis',(0.996957691137886,-6.86676610464798E-16,
0.0779446090567885));
#43491=DIRECTION('ref_axis',(5.96188116413496E-16,1.,1.18420354606057E-15));
#43492=DIRECTION('',(-0.0779446090567885,-1.13413118345969E-15,0.996957691137886));
#43493=DIRECTION('',(5.96188116413496E-16,1.,1.18420354606057E-15));
#43494=DIRECTION('',(-0.0779446090567885,-1.13413118345969E-15,0.996957691137886));
#43495=DIRECTION('center_axis',(-0.0779446090567885,-1.13413118345969E-15,
0.996957691137886));
#43496=DIRECTION('ref_axis',(-5.18990262561707E-16,1.,1.09701615230207E-15));
#43497=DIRECTION('center_axis',(-0.0779446090567885,-1.13413118345969E-15,
0.996957691137886));
#43498=DIRECTION('ref_axis',(-4.8857814859476E-16,-1.,-1.17579033359749E-15));
#43499=DIRECTION('',(-0.0779446090567885,-1.13413118345969E-15,0.996957691137886));
#43500=DIRECTION('center_axis',(-0.996957691137886,8.41043700732428E-16,
-0.0779446090567885));
#43501=DIRECTION('ref_axis',(-7.50085574314386E-16,-1.,-1.19623562856271E-15));
#43502=DIRECTION('',(-6.19242119716166E-16,-1.,-1.18600596484984E-15));
#43503=DIRECTION('',(-0.0779446090567885,-1.13413118345969E-15,0.996957691137886));
#43504=DIRECTION('center_axis',(-0.0779446090567885,-1.13413118345969E-15,
0.996957691137886));
#43505=DIRECTION('ref_axis',(-4.88578148594761E-16,-1.,-1.17579033359749E-15));
#43506=DIRECTION('center_axis',(-0.0779446090567885,-1.13413118345969E-15,
0.996957691137886));
#43507=DIRECTION('ref_axis',(-4.88578148594761E-16,-1.,-1.17579033359749E-15));
#43508=DIRECTION('center_axis',(-0.0779446090567885,-1.13413118345969E-15,
0.996957691137886));
#43509=DIRECTION('ref_axis',(0.996957691137886,-5.78738260848462E-16,0.0779446090567885));
#43510=DIRECTION('center_axis',(4.88578148594761E-16,1.,1.17579033359749E-15));
#43511=DIRECTION('ref_axis',(-0.0779446090567885,-1.13413118345969E-15,
0.996957691137886));
#43512=DIRECTION('center_axis',(-4.88578148594761E-16,-1.,-1.17579033359749E-15));
#43513=DIRECTION('ref_axis',(-0.0779446090567885,-1.13413118345969E-15,
0.996957691137886));
#43514=DIRECTION('center_axis',(-4.88578148594761E-16,-1.,-1.17579033359749E-15));
#43515=DIRECTION('ref_axis',(-0.0779446090567885,-1.13413118345969E-15,
0.996957691137886));
#43516=DIRECTION('',(-0.0551151616209894,-0.707106781186553,0.704955543959677));
#43517=DIRECTION('center_axis',(4.88578148594761E-16,1.,1.17579033359749E-15));
#43518=DIRECTION('ref_axis',(-0.0779446090567885,-1.13413118345969E-15,
0.996957691137886));
#43519=DIRECTION('center_axis',(-4.88578148594761E-16,-1.,-1.17579033359749E-15));
#43520=DIRECTION('ref_axis',(-0.996957691137886,5.78738260848462E-16,-0.0779446090567885));
#43521=DIRECTION('center_axis',(-4.88578148594761E-16,-1.,-1.17579033359749E-15));
#43522=DIRECTION('ref_axis',(-0.0779446090567887,-1.13413118345969E-15,
0.996957691137886));
#43523=DIRECTION('center_axis',(4.88578148594761E-16,1.,1.17579033359749E-15));
#43524=DIRECTION('ref_axis',(0.0779446090567885,1.13413118345969E-15,-0.996957691137886));
#43525=DIRECTION('center_axis',(4.88578148594761E-16,1.,1.17579033359749E-15));
#43526=DIRECTION('ref_axis',(0.996957691137886,-5.78738260848463E-16,0.0779446090567885));
#43527=DIRECTION('',(-4.88578148594761E-16,-1.,-1.17579033359749E-15));
#43528=DIRECTION('center_axis',(4.88578148594761E-16,1.,1.17579033359749E-15));
#43529=DIRECTION('ref_axis',(0.996957691137886,-5.78738260848463E-16,0.0779446090567885));
#43530=DIRECTION('center_axis',(4.88578148594761E-16,1.,1.17579033359749E-15));
#43531=DIRECTION('ref_axis',(0.996957691137886,0.,0.0779446090567894));
#43532=DIRECTION('center_axis',(0.0779446090567902,1.13413118345969E-15,
-0.996957691137886));
#43533=DIRECTION('ref_axis',(-0.996957691137886,0.,-0.0779446090567902));
#43534=DIRECTION('center_axis',(4.88578148594761E-16,1.,1.17579033359749E-15));
#43535=DIRECTION('ref_axis',(-0.0779446090567887,-1.13413118345969E-15,
0.996957691137886));
#43536=DIRECTION('center_axis',(4.88578148594761E-16,1.,1.17579033359749E-15));
#43537=DIRECTION('ref_axis',(-0.0779446090567887,-1.13413118345969E-15,
0.996957691137886));
#43538=DIRECTION('center_axis',(4.88578148594761E-16,1.,1.17579033359749E-15));
#43539=DIRECTION('ref_axis',(0.0779446090567885,1.13413118345969E-15,-0.996957691137886));
#43540=DIRECTION('',(-4.88578148594761E-16,-1.,-1.17579033359749E-15));
#43541=DIRECTION('center_axis',(-4.88578148594761E-16,-1.,-1.17579033359749E-15));
#43542=DIRECTION('ref_axis',(-0.0779446090567885,-1.13413118345969E-15,
0.996957691137886));
#43543=DIRECTION('center_axis',(-4.88578148594761E-16,-1.,-1.17579033359749E-15));
#43544=DIRECTION('ref_axis',(-0.0779446090567885,-1.13413118345969E-15,
0.996957691137886));
#43545=DIRECTION('center_axis',(4.88578148594761E-16,1.,1.17579033359749E-15));
#43546=DIRECTION('ref_axis',(0.996957691137886,-8.88178419700125E-16,0.0779446090567894));
#43547=DIRECTION('center_axis',(0.0779446090567902,1.13413118345969E-15,
-0.996957691137886));
#43548=DIRECTION('ref_axis',(-0.996957691137886,1.11022302462515E-15,-0.0779446090567902));
#43549=DIRECTION('center_axis',(4.88578148594761E-16,1.,1.17579033359749E-15));
#43550=DIRECTION('ref_axis',(-0.0779446090567887,-1.13413118345969E-15,
0.996957691137886));
#43551=DIRECTION('center_axis',(4.88578148594761E-16,1.,1.17579033359749E-15));
#43552=DIRECTION('ref_axis',(0.996957691137886,-5.78738260848462E-16,0.0779446090567885));
#43553=DIRECTION('center_axis',(-4.88578148594761E-16,-1.,-1.17579033359749E-15));
#43554=DIRECTION('ref_axis',(-0.0779446090567885,-1.13413118345969E-15,
0.996957691137886));
#43555=DIRECTION('center_axis',(-4.88578148594761E-16,-1.,-1.17579033359749E-15));
#43556=DIRECTION('ref_axis',(-0.0779446090567885,-1.13413118345969E-15,
0.996957691137886));
#43557=DIRECTION('center_axis',(4.88578148594761E-16,1.,1.17579033359749E-15));
#43558=DIRECTION('ref_axis',(-0.0779446090567885,-1.13413118345969E-15,
0.996957691137886));
#43559=DIRECTION('center_axis',(4.88578148594761E-16,1.,1.17579033359749E-15));
#43560=DIRECTION('ref_axis',(-0.0779446090567885,-1.13413118345969E-15,
0.996957691137886));
#43561=DIRECTION('',(-0.0551151616209894,0.707106781186545,0.704955543959685));
#43562=DIRECTION('center_axis',(4.88578148594761E-16,1.,1.17579033359749E-15));
#43563=DIRECTION('ref_axis',(0.0779446090567885,1.13413118345969E-15,-0.996957691137886));
#43564=DIRECTION('',(-4.88578148594761E-16,-1.,-1.17579033359749E-15));
#43565=DIRECTION('center_axis',(4.88578148594761E-16,1.,1.17579033359749E-15));
#43566=DIRECTION('ref_axis',(0.996957691137886,-5.78738260848463E-16,0.0779446090567885));
#43567=DIRECTION('center_axis',(4.88578148594761E-16,1.,1.17579033359749E-15));
#43568=DIRECTION('ref_axis',(0.996957691137886,-5.78738260848463E-16,0.0779446090567885));
#43569=DIRECTION('center_axis',(4.88578148594761E-16,1.,1.17579033359749E-15));
#43570=DIRECTION('ref_axis',(-0.0779446090567885,-1.13413118345969E-15,
0.996957691137886));
#43571=DIRECTION('',(-0.0551151616209896,-0.707106781186551,0.70495554395968));
#43572=DIRECTION('center_axis',(4.88578148594761E-16,1.,1.17579033359749E-15));
#43573=DIRECTION('ref_axis',(-0.0779446090567885,-1.13413118345969E-15,
0.996957691137886));
#43574=DIRECTION('center_axis',(-4.88578148594761E-16,-1.,-1.17579033359749E-15));
#43575=DIRECTION('ref_axis',(-0.996957691137886,5.78738260848462E-16,-0.0779446090567885));
#43576=DIRECTION('center_axis',(-0.0779446090567885,-1.13413118345969E-15,
0.996957691137886));
#43577=DIRECTION('ref_axis',(0.996957691137886,-5.78738260848462E-16,0.0779446090567885));
#43578=DIRECTION('',(-0.0779446090567885,-1.13413118345969E-15,0.996957691137886));
#43579=DIRECTION('center_axis',(-0.0779446090567885,-1.13413118345969E-15,
0.996957691137886));
#43580=DIRECTION('ref_axis',(0.996957691137886,-5.78738260848462E-16,0.0779446090567885));
#43581=DIRECTION('',(-0.0779446090567885,-1.13413118345969E-15,0.996957691137886));
#43582=DIRECTION('center_axis',(0.996957691137886,-5.78738260848463E-16,
0.0779446090567885));
#43583=DIRECTION('ref_axis',(4.88578148594761E-16,1.,1.17579033359749E-15));
#43584=DIRECTION('',(4.88578148594761E-16,1.,1.17579033359749E-15));
#43585=DIRECTION('',(4.88578148594761E-16,1.,1.17579033359749E-15));
#43586=DIRECTION('',(-0.0779446090567885,-1.13413118345969E-15,0.996957691137886));
#43587=DIRECTION('center_axis',(-0.996957691137886,5.78738260848463E-16,
-0.0779446090567885));
#43588=DIRECTION('ref_axis',(-4.88578148594761E-16,-1.,-1.17579033359749E-15));
#43589=DIRECTION('',(-0.0779446090567885,-1.13413118345969E-15,0.996957691137886));
#43590=DIRECTION('',(-4.88578148594761E-16,-1.,-1.17579033359749E-15));
#43591=DIRECTION('center_axis',(-0.0779446090567885,-1.13413118345969E-15,
0.996957691137886));
#43592=DIRECTION('ref_axis',(-0.996957691137886,5.78738260848462E-16,-0.0779446090567885));
#43593=DIRECTION('center_axis',(-0.0779446090567885,-1.13413118345969E-15,
0.996957691137886));
#43594=DIRECTION('ref_axis',(-0.996957691137886,5.78738260848462E-16,-0.0779446090567885));
#43595=DIRECTION('center_axis',(0.0779446090567885,1.13413118345969E-15,
-0.996957691137886));
#43596=DIRECTION('ref_axis',(-0.996957691137886,5.78738260848462E-16,-0.0779446090567885));
#43597=DIRECTION('center_axis',(4.88578148594761E-16,1.,1.17579033359749E-15));
#43598=DIRECTION('ref_axis',(0.0779446090567885,1.13413118345969E-15,-0.996957691137886));
#43599=DIRECTION('center_axis',(4.88578148594761E-16,1.,1.17579033359749E-15));
#43600=DIRECTION('ref_axis',(0.996957691137886,-5.78738260848463E-16,0.0779446090567885));
#43601=DIRECTION('center_axis',(4.88578148594761E-16,1.,1.17579033359749E-15));
#43602=DIRECTION('ref_axis',(0.996957691137886,-5.78738260848463E-16,0.0779446090567885));
#43603=DIRECTION('center_axis',(4.88578148594761E-16,1.,1.17579033359749E-15));
#43604=DIRECTION('ref_axis',(0.996957691137886,0.,0.0779446090567891));
#43605=DIRECTION('center_axis',(4.88578148594761E-16,1.,1.17579033359749E-15));
#43606=DIRECTION('ref_axis',(0.996957691137886,-5.78738260848463E-16,0.0779446090567885));
#43607=DIRECTION('center_axis',(0.0779446090567875,1.13413118345969E-15,
-0.996957691137886));
#43608=DIRECTION('ref_axis',(-0.996957691137886,0.,-0.0779446090567875));
#43609=DIRECTION('center_axis',(-4.88578148594761E-16,-1.,-1.17579033359749E-15));
#43610=DIRECTION('ref_axis',(-0.996957691137886,5.78738260848462E-16,-0.0779446090567885));
#43611=DIRECTION('center_axis',(4.88578148594761E-16,1.,1.17579033359749E-15));
#43612=DIRECTION('ref_axis',(0.996957691137886,-5.78738260848463E-16,0.0779446090567885));
#43613=DIRECTION('center_axis',(4.88578148594761E-16,1.,1.17579033359749E-15));
#43614=DIRECTION('ref_axis',(0.0779446090567885,1.13413118345969E-15,-0.996957691137886));
#43615=DIRECTION('',(0.0551151616209892,-0.707106781186546,-0.704955543959685));
#43616=DIRECTION('center_axis',(-4.88578148594761E-16,-1.,-1.17579033359749E-15));
#43617=DIRECTION('ref_axis',(0.0779446090567885,1.13413118345969E-15,-0.996957691137886));
#43618=DIRECTION('',(0.0551151616209901,0.707106781186547,-0.704955543959683));
#43619=DIRECTION('center_axis',(4.88578148594761E-16,1.,1.17579033359749E-15));
#43620=DIRECTION('ref_axis',(0.996957691137886,-5.78738260848463E-16,0.0779446090567885));
#43621=DIRECTION('center_axis',(4.88578148594761E-16,1.,1.17579033359749E-15));
#43622=DIRECTION('ref_axis',(0.996957691137886,-5.78738260848462E-16,0.0779446090567885));
#43623=DIRECTION('center_axis',(4.88578148594761E-16,1.,1.17579033359749E-15));
#43624=DIRECTION('ref_axis',(0.996957691137886,-5.78738260848463E-16,0.0779446090567885));
#43625=DIRECTION('center_axis',(4.88578148594761E-16,1.,1.17579033359749E-15));
#43626=DIRECTION('ref_axis',(0.996957691137886,-7.28761780266769E-16,0.0779446090567891));
#43627=DIRECTION('center_axis',(0.0779446090567878,1.13413118345969E-15,
-0.996957691137886));
#43628=DIRECTION('ref_axis',(-0.996957691137886,9.10952225333462E-16,-0.0779446090567878));
#43629=DIRECTION('axis',(0.,0.,1.));
#43630=DIRECTION('refdir',(1.,0.,0.));
#43631=DIRECTION('center_axis',(-0.996957691137886,1.38453029710175E-15,
-0.0779446090567869));
#43632=DIRECTION('ref_axis',(-0.0779446090567869,-2.95972462712666E-15,
0.996957691137886));
#43633=DIRECTION('',(1.14962354933188E-15,1.,3.05863690339901E-15));
#43634=DIRECTION('',(-0.0779446090567869,-2.95972462712666E-15,0.996957691137886));
#43635=DIRECTION('',(1.14962354933188E-15,1.,3.05863690339901E-15));
#43636=DIRECTION('',(0.0779446090567869,2.95972462712666E-15,-0.996957691137886));
#43637=DIRECTION('center_axis',(0.0779446090567869,2.95972462712666E-15,
-0.996957691137886));
#43638=DIRECTION('ref_axis',(-0.996957691137886,1.38453029710175E-15,-0.0779446090567869));
#43639=DIRECTION('',(-0.996957691137886,1.38453029710175E-15,-0.0779446090567869));
#43640=DIRECTION('',(1.14962354933188E-15,1.,3.05863690339901E-15));
#43641=DIRECTION('',(0.996957691137886,-1.38453029710175E-15,0.0779446090567869));
#43642=DIRECTION('center_axis',(0.996957691137886,-1.38453029710175E-15,
0.0779446090567869));
#43643=DIRECTION('ref_axis',(0.0779446090567869,2.95972462712666E-15,-0.996957691137886));
#43644=DIRECTION('',(-1.14962354933188E-15,-1.,-3.05863690339901E-15));
#43645=DIRECTION('',(-0.0779446090567869,-2.95972462712666E-15,0.996957691137886));
#43646=DIRECTION('',(0.0779446090567869,2.95972462712666E-15,-0.996957691137886));
#43647=DIRECTION('center_axis',(1.14962354933188E-15,1.,3.05863690339901E-15));
#43648=DIRECTION('ref_axis',(0.996957691137886,-1.38453029710175E-15,0.0779446090567869));
#43649=DIRECTION('center_axis',(1.14962354933188E-15,1.,3.05863690339901E-15));
#43650=DIRECTION('ref_axis',(0.996957691137886,-1.38453029710175E-15,0.077944609056787));
#43651=DIRECTION('center_axis',(-1.14962354933188E-15,-1.,-3.05863690339901E-15));
#43652=DIRECTION('ref_axis',(0.996957691137886,-1.38453029710175E-15,0.077944609056787));
#43653=DIRECTION('center_axis',(-1.14962354933188E-15,-1.,-3.05863690339901E-15));
#43654=DIRECTION('ref_axis',(-0.079454779543177,-2.95762384959718E-15,0.99683847137224));
#43655=DIRECTION('center_axis',(1.14962354933188E-15,1.,3.05863690339901E-15));
#43656=DIRECTION('ref_axis',(0.996957691137886,-1.38453029710175E-15,0.077944609056787));
#43657=DIRECTION('center_axis',(-1.14962354933188E-15,-1.,-3.05863690339901E-15));
#43658=DIRECTION('ref_axis',(0.996957691137886,-1.38453029710175E-15,0.077944609056787));
#43659=DIRECTION('center_axis',(-1.14962354933188E-15,-1.,-3.05863690339901E-15));
#43660=DIRECTION('ref_axis',(0.996957691137886,-1.38453029710175E-15,0.077944609056787));
#43661=DIRECTION('',(1.14962354933188E-15,1.,3.05863690339901E-15));
#43662=DIRECTION('center_axis',(1.14962354933188E-15,1.,3.05863690339901E-15));
#43663=DIRECTION('ref_axis',(0.996957691137886,-1.38453029710175E-15,0.0779446090567869));
#43664=DIRECTION('axis',(0.,0.,1.));
#43665=DIRECTION('refdir',(1.,0.,0.));
#43666=DIRECTION('center_axis',(-5.00596043934461E-16,-1.,-1.12027918221652E-15));
#43667=DIRECTION('ref_axis',(-5.46077161851015E-15,1.12027918221652E-15,
-1.));
#43668=DIRECTION('center_axis',(-5.00596043934461E-16,-1.,-1.12027918221652E-15));
#43669=DIRECTION('ref_axis',(-5.46077161851015E-15,1.12027918221652E-15,
-1.));
#43670=DIRECTION('',(-5.00596043934461E-16,-1.,-1.12027918221652E-15));
#43671=DIRECTION('center_axis',(5.00596043934461E-16,1.,1.12027918221652E-15));
#43672=DIRECTION('ref_axis',(-5.46077161851015E-15,1.12027918221652E-15,
-1.));
#43673=DIRECTION('center_axis',(-5.00596043934461E-16,-1.,-1.12027918221652E-15));
#43674=DIRECTION('ref_axis',(-5.46077161851015E-15,1.12027918221652E-15,
-1.));
#43675=DIRECTION('center_axis',(5.00596043934461E-16,1.,1.12027918221652E-15));
#43676=DIRECTION('ref_axis',(-5.46077161851015E-15,1.12027918221652E-15,
-1.));
#43677=DIRECTION('',(5.00596043934461E-16,1.,1.12027918221652E-15));
#43678=DIRECTION('center_axis',(5.00596043934461E-16,1.,1.12027918221652E-15));
#43679=DIRECTION('ref_axis',(-5.46077161851015E-15,1.12027918221652E-15,
-1.));
#43680=DIRECTION('center_axis',(5.00596043934461E-16,1.,1.12027918221652E-15));
#43681=DIRECTION('ref_axis',(-1.,5.00596043934455E-16,5.46077161851015E-15));
#43682=DIRECTION('center_axis',(5.00596043934461E-16,1.,1.12027918221652E-15));
#43683=DIRECTION('ref_axis',(-1.,5.00596043934455E-16,5.46077161851015E-15));
#43684=DIRECTION('',(0.,0.,1.));
#43685=DIRECTION('',(1.,0.,0.));
#43686=DIRECTION('',(0.,0.,1.));
#43687=DIRECTION('',(1.,0.,0.));
#43688=DIRECTION('',(0.,0.,1.));
#43689=DIRECTION('',(1.,0.,0.));
#43690=DIRECTION('',(-0.155414954963802,-5.8307489838191E-15,0.987849275837969));
#43691=DIRECTION('',(-0.987849275837969,-2.51353580688625E-16,-0.155414954963802));
#43692=DIRECTION('',(-0.155414954963802,-5.83074898381911E-15,0.987849275837969));
#43693=DIRECTION('',(-0.987849275837969,-2.51353580688618E-16,-0.155414954963802));
#43694=DIRECTION('',(-0.155414954963801,-5.89104332304954E-15,0.987849275837969));
#43695=DIRECTION('',(-0.987849275837969,-3.08354957615452E-16,-0.155414954963801));
#43696=DIRECTION('',(-0.155414954963802,-5.8307489838191E-15,0.987849275837969));
#43697=DIRECTION('',(-0.987849275837969,-2.51353580688625E-16,-0.155414954963802));
#43698=DIRECTION('',(-0.996957691137886,-2.64433129580477E-15,-0.0779446090567815));
#43699=DIRECTION('',(0.0779446090567815,-2.11868331653527E-15,-0.996957691137886));
#43700=DIRECTION('',(-0.996957691137885,3.51373972301721E-15,0.0779446090567923));
#43701=DIRECTION('',(0.0779446090567924,2.31931285848024E-15,0.996957691137886));
#43702=DIRECTION('',(-0.996957691137885,3.51373972301722E-15,0.0779446090567923));
#43703=DIRECTION('',(0.0779446090567924,2.31931285848024E-15,0.996957691137886));
#43704=DIRECTION('',(-0.996957691137886,3.57403406224764E-15,0.0779446090567909));
#43705=DIRECTION('',(0.0779446090567909,2.37631423540707E-15,0.996957691137886));
#43706=DIRECTION('',(-0.996957691137885,3.51373972301721E-15,0.0779446090567923));
#43707=DIRECTION('',(0.0779446090567924,2.31931285848024E-15,0.996957691137886));
#43708=DIRECTION('',(0.,0.,1.));
#43709=DIRECTION('',(1.,0.,0.));
#43710=DIRECTION('',(0.110937982438767,1.74251121353013E-14,0.993827331105568));
#43711=DIRECTION('',(0.993827331105568,-2.47622772469446E-15,-0.110937982438767));
#43712=DIRECTION('',(1.09215432370203E-14,-2.21663502267315E-15,1.));
#43713=DIRECTION('',(-1.,-1.20178972545062E-17,1.09215432370203E-14));
#43714=DIRECTION('',(3.33066907387546E-16,-1.66230702095476E-30,1.));
#43715=DIRECTION('',(1.,2.99396245797037E-16,-3.33066907387547E-16));
#43716=DIRECTION('axis',(0.,0.,1.));
#43717=DIRECTION('refdir',(1.,0.,0.));
#43718=DIRECTION('axis',(0.,0.,1.));
#43719=DIRECTION('refdir',(1.,0.,0.));
#43720=DIRECTION('center_axis',(3.66113466765132E-16,1.,1.12027918221652E-15));
#43721=DIRECTION('ref_axis',(-5.6843418860808E-15,1.12502599828683E-15,
-1.));
#43722=DIRECTION('center_axis',(-3.66113466765132E-16,-1.,-1.12027918221652E-15));
#43723=DIRECTION('ref_axis',(5.46077161851015E-15,-1.12027918221652E-15,
1.));
#43724=DIRECTION('center_axis',(1.,-3.66113466765125E-16,-5.9211894646675E-15));
#43725=DIRECTION('ref_axis',(5.9211894646675E-15,-1.11022302462516E-15,
1.));
#43726=DIRECTION('center_axis',(3.66113466765132E-16,1.,1.12027918221652E-15));
#43727=DIRECTION('ref_axis',(5.46077161851015E-15,-1.12027918221652E-15,
1.));
#43728=DIRECTION('center_axis',(3.66113466765132E-16,1.,1.12027918221652E-15));
#43729=DIRECTION('ref_axis',(5.46077161851015E-15,-1.12027918221652E-15,
1.));
#43730=DIRECTION('center_axis',(3.66113466765132E-16,1.,1.12027918221652E-15));
#43731=DIRECTION('ref_axis',(5.46077161851015E-15,-1.12027918221652E-15,
1.));
#43732=DIRECTION('',(-3.66113466765132E-16,-1.,-1.12027918221652E-15));
#43733=DIRECTION('center_axis',(-3.66113466765132E-16,-1.,-1.12027918221652E-15));
#43734=DIRECTION('ref_axis',(5.46077161851015E-15,-1.12027918221652E-15,
1.));
#43735=DIRECTION('center_axis',(3.66113466765132E-16,1.,1.12027918221652E-15));
#43736=DIRECTION('ref_axis',(-5.46077161851015E-15,1.12027918221652E-15,
-1.));
#43737=DIRECTION('',(1.,-3.66113466765126E-16,-5.46077161851015E-15));
#43738=DIRECTION('',(5.46077161851015E-15,-1.12027918221652E-15,1.));
#43739=DIRECTION('',(-1.,3.66113466765126E-16,5.46077161851015E-15));
#43740=DIRECTION('center_axis',(-3.66113466765132E-16,-1.,-1.12027918221652E-15));
#43741=DIRECTION('ref_axis',(-0.916515138991166,-1.12563138007831E-16,0.400000000000005));
#43742=DIRECTION('center_axis',(-3.66113466765132E-16,-1.,-1.12027918221652E-15));
#43743=DIRECTION('ref_axis',(5.015595781836E-15,-1.12328447197369E-15,1.));
#43744=DIRECTION('center_axis',(3.66113466765132E-16,1.,1.12027918221652E-15));
#43745=DIRECTION('ref_axis',(5.46077161851015E-15,-1.12027918221652E-15,
1.));
#43746=DIRECTION('center_axis',(-1.,3.66113466765126E-16,5.2245789394125E-15));
#43747=DIRECTION('ref_axis',(-5.2245789394125E-15,1.12654983381082E-15,
-1.));
#43748=DIRECTION('center_axis',(-3.66113466765132E-16,-1.,-1.12027918221652E-15));
#43749=DIRECTION('ref_axis',(5.46077161851015E-15,-1.12027918221652E-15,
1.));
#43750=DIRECTION('center_axis',(3.66113466765132E-16,1.,1.12027918221652E-15));
#43751=DIRECTION('ref_axis',(-0.0850481328578615,-1.08508296912223E-15,
0.996376843918701));
#43752=DIRECTION('center_axis',(3.66113466765132E-16,1.,1.12027918221652E-15));
#43753=DIRECTION('ref_axis',(-0.97746197494357,1.21358115044514E-16,0.211111552358972));
#43754=DIRECTION('center_axis',(3.66113466765132E-16,1.,1.12027918221652E-15));
#43755=DIRECTION('ref_axis',(-0.632741728117551,1.09915790732807E-15,-0.774362902971737));
#43756=DIRECTION('center_axis',(-3.66113466765132E-16,-1.,-1.12027918221652E-15));
#43757=DIRECTION('ref_axis',(5.46077161851015E-15,-1.12027918221652E-15,
1.));
#43758=DIRECTION('center_axis',(3.66113466765132E-16,1.,1.12027918221652E-15));
#43759=DIRECTION('ref_axis',(0.0457327411615766,-1.13585041865483E-15,0.998953710832413));
#43760=DIRECTION('center_axis',(3.66113466765132E-16,1.,1.12027918221652E-15));
#43761=DIRECTION('ref_axis',(-0.941544065183018,-3.26987276389964E-17,0.336889853392226));
#43762=DIRECTION('center_axis',(3.66113466765132E-16,1.,1.12027918221652E-15));
#43763=DIRECTION('ref_axis',(-0.728403176040296,1.03423609619734E-15,-0.685148752559916));
#43764=DIRECTION('center_axis',(-3.66113466765132E-16,-1.,-1.12027918221652E-15));
#43765=DIRECTION('ref_axis',(5.46077161851015E-15,-1.12027918221652E-15,
1.));
#43766=DIRECTION('center_axis',(3.66113466765132E-16,1.,1.12027918221652E-15));
#43767=DIRECTION('ref_axis',(0.175731115300229,-1.16718315260702E-15,0.984438202791489));
#43768=DIRECTION('center_axis',(3.66113466765132E-16,1.,1.12027918221652E-15));
#43769=DIRECTION('ref_axis',(-0.889516075421853,-1.86196086026804E-16,0.456903875630427));
#43770=DIRECTION('center_axis',(3.66113466765132E-16,1.,1.12027918221652E-15));
#43771=DIRECTION('ref_axis',(-0.811601443669479,9.51618218716255E-16,-0.584211517032673));
#43772=DIRECTION('center_axis',(-3.66113466765132E-16,-1.,-1.12027918221652E-15));
#43773=DIRECTION('ref_axis',(5.46077161851015E-15,-1.12027918221652E-15,
1.));
#43774=DIRECTION('center_axis',(3.66113466765132E-16,1.,1.12027918221652E-15));
#43775=DIRECTION('ref_axis',(0.302722681334224,-1.1785450592138E-15,0.95307868416297));
#43776=DIRECTION('center_axis',(3.66113466765132E-16,1.,1.12027918221652E-15));
#43777=DIRECTION('ref_axis',(-0.822268218989772,-3.36507577759385E-16,0.569100145878903));
#43778=DIRECTION('center_axis',(3.66113466765132E-16,1.,1.12027918221652E-15));
#43779=DIRECTION('ref_axis',(-0.880912985579045,8.52717889674523E-16,-0.473278260474969));
#43780=DIRECTION('center_axis',(-3.66113466765132E-16,-1.,-1.12027918221652E-15));
#43781=DIRECTION('ref_axis',(5.46077161851015E-15,-1.12027918221652E-15,
1.));
#43782=DIRECTION('center_axis',(3.66113466765132E-16,1.,1.12027918221652E-15));
#43783=DIRECTION('ref_axis',(0.424534578360008,-1.16974173310301E-15,0.905411725005089));
#43784=DIRECTION('center_axis',(3.66113466765132E-16,1.,1.12027918221652E-15));
#43785=DIRECTION('ref_axis',(-0.740951125354955,-4.81061331538975E-16,0.671558954847023));
#43786=DIRECTION('center_axis',(3.66113466765132E-16,1.,1.12027918221652E-15));
#43787=DIRECTION('ref_axis',(-0.935151862070134,7.39227321122395E-16,-0.354247081663014));
#43788=DIRECTION('center_axis',(-3.66113466765132E-16,-1.,-1.12027918221652E-15));
#43789=DIRECTION('ref_axis',(5.46077161851015E-15,-1.12027918221652E-15,
1.));
#43790=DIRECTION('center_axis',(3.66113466765132E-16,1.,1.12027918221652E-15));
#43791=DIRECTION('ref_axis',(0.53908257104683,-1.14092380162514E-15,0.842252920204816));
#43792=DIRECTION('center_axis',(3.66113466765132E-16,1.,1.12027918221652E-15));
#43793=DIRECTION('ref_axis',(-0.646956152534853,-6.17383992560537E-16,0.762527203906392));
#43794=DIRECTION('center_axis',(3.66113466765132E-16,1.,1.12027918221652E-15));
#43795=DIRECTION('ref_axis',(-0.973390030928123,6.13088368153331E-16,-0.229154637067959));
#43796=DIRECTION('center_axis',(-3.66113466765132E-16,-1.,-1.12027918221652E-15));
#43797=DIRECTION('ref_axis',(5.46077161851015E-15,-1.12027918221652E-15,
1.));
#43798=DIRECTION('center_axis',(3.66113466765132E-16,1.,1.12027918221652E-15));
#43799=DIRECTION('ref_axis',(0.644406711481115,-1.09258434757764E-15,0.764682934423213));
#43800=DIRECTION('center_axis',(3.66113466765132E-16,1.,1.12027918221652E-15));
#43801=DIRECTION('ref_axis',(-0.541891580574746,-7.43143042298206E-16,0.840448401094442));
#43802=DIRECTION('center_axis',(3.66113466765132E-16,1.,1.12027918221652E-15));
#43803=DIRECTION('ref_axis',(-0.994973226482231,4.76459303224952E-16,-0.100141293099001));
#43804=DIRECTION('center_axis',(-3.66113466765132E-16,-1.,-1.12027918221652E-15));
#43805=DIRECTION('ref_axis',(5.46077161851015E-15,-1.12027918221652E-15,
1.));
#43806=DIRECTION('center_axis',(3.66113466765132E-16,1.,1.12027918221652E-15));
#43807=DIRECTION('ref_axis',(0.738704874418665,-1.02555047242146E-15,0.674029011623465));
#43808=DIRECTION('center_axis',(3.66113466765132E-16,1.,1.12027918221652E-15));
#43809=DIRECTION('ref_axis',(-0.427555093430276,-8.56186708543976E-16,0.903989293123446));
#43810=DIRECTION('center_axis',(3.66113466765132E-16,1.,1.12027918221652E-15));
#43811=DIRECTION('ref_axis',(-0.999532154272533,3.3167788751892E-16,0.0305854961592914));
#43812=DIRECTION('center_axis',(-3.66113466765132E-16,-1.,-1.12027918221652E-15));
#43813=DIRECTION('ref_axis',(5.46077161851015E-15,-1.12027918221652E-15,
1.));
#43814=DIRECTION('center_axis',(3.66113466765132E-16,1.,1.12027918221652E-15));
#43815=DIRECTION('ref_axis',(0.820363592147227,-9.40969144345853E-16,0.571842265558692));
#43816=DIRECTION('center_axis',(3.66113466765132E-16,1.,1.12027918221652E-15));
#43817=DIRECTION('ref_axis',(-0.305903020096547,-9.54580782826758E-16,0.952062677713926));
#43818=DIRECTION('center_axis',(3.66113466765132E-16,1.,1.12027918221652E-15));
#43819=DIRECTION('ref_axis',(-0.986988809780564,1.81221371198957E-16,0.160788959098396));
#43820=DIRECTION('center_axis',(-3.66113466765132E-16,-1.,-1.12027918221652E-15));
#43821=DIRECTION('ref_axis',(5.46077161851015E-15,-1.12027918221652E-15,
1.));
#43822=DIRECTION('center_axis',(3.66113466765132E-16,1.,1.12027918221652E-15));
#43823=DIRECTION('ref_axis',(0.887985661366392,-8.40287573324551E-16,0.459871139785583));
#43824=DIRECTION('center_axis',(3.66113466765132E-16,1.,1.12027918221652E-15));
#43825=DIRECTION('ref_axis',(-0.179016861276626,-1.03664171525558E-15,0.983846005927078));
#43826=DIRECTION('center_axis',(3.66113466765132E-16,1.,1.12027918221652E-15));
#43827=DIRECTION('ref_axis',(-0.957557813108254,2.76641069737215E-17,0.288241278368207));
#43828=DIRECTION('center_axis',(-3.66113466765132E-16,-1.,-1.12027918221652E-15));
#43829=DIRECTION('ref_axis',(5.46077161851015E-15,-1.12027918221652E-15,
1.));
#43830=DIRECTION('center_axis',(3.66113466765132E-16,1.,1.12027918221652E-15));
#43831=DIRECTION('ref_axis',(0.940414049723441,-7.25228448951937E-16,0.340031491310375));
#43832=DIRECTION('center_axis',(3.66113466765132E-16,1.,1.12027918221652E-15));
#43833=DIRECTION('ref_axis',(-0.0490676743274118,-1.100965420525E-15,0.998795456205173));
#43834=DIRECTION('center_axis',(3.66113466765132E-16,1.,1.12027918221652E-15));
#43835=DIRECTION('ref_axis',(-0.91174273676848,-1.26366497791772E-16,0.410761709449557));
#43836=DIRECTION('center_axis',(-3.66113466765132E-16,-1.,-1.12027918221652E-15));
#43837=DIRECTION('ref_axis',(5.46077161851015E-15,-1.12027918221652E-15,
1.));
#43838=DIRECTION('center_axis',(3.66113466765132E-16,1.,1.12027918221652E-15));
#43839=DIRECTION('ref_axis',(0.976751692957689,-5.97760464746442E-16,0.214373809744306));
#43840=DIRECTION('center_axis',(3.66113466765132E-16,1.,1.12027918221652E-15));
#43841=DIRECTION('ref_axis',(0.0817210741336744,-1.14645130220395E-15,0.99665523930918));
#43842=DIRECTION('center_axis',(3.66113466765132E-16,1.,1.12027918221652E-15));
#43843=DIRECTION('ref_axis',(-0.850327489419754,-2.78234936744637E-16,0.526253893797564));
#43844=DIRECTION('center_axis',(-3.66113466765132E-16,-1.,-1.12027918221652E-15));
#43845=DIRECTION('ref_axis',(5.46077161851015E-15,-1.12027918221652E-15,
1.));
#43846=DIRECTION('center_axis',(3.66113466765132E-16,1.,1.12027918221652E-15));
#43847=DIRECTION('ref_axis',(0.996376843918701,-4.60064633258624E-16,0.0850481328578616));
#43848=DIRECTION('center_axis',(3.66113466765132E-16,1.,1.12027918221652E-15));
#43849=DIRECTION('ref_axis',(0.211111552358972,-1.17232108424584E-15,0.97746197494357));
#43850=DIRECTION('center_axis',(3.66113466765132E-16,1.,1.12027918221652E-15));
#43851=DIRECTION('ref_axis',(-0.774362902971737,-4.25342698788503E-16,0.632741728117551));
#43852=DIRECTION('center_axis',(-3.66113466765132E-16,-1.,-1.12027918221652E-15));
#43853=DIRECTION('ref_axis',(5.46077161851015E-15,-1.12027918221652E-15,
1.));
#43854=DIRECTION('center_axis',(3.66113466765132E-16,1.,1.12027918221652E-15));
#43855=DIRECTION('ref_axis',(0.998953710832413,-3.14496968341737E-16,-0.0457327411615765));
#43856=DIRECTION('center_axis',(3.66113466765132E-16,1.,1.12027918221652E-15));
#43857=DIRECTION('ref_axis',(0.336889853392226,-1.17813212750748E-15,0.941544065183018));
#43858=DIRECTION('center_axis',(3.66113466765132E-16,1.,1.12027918221652E-15));
#43859=DIRECTION('ref_axis',(-0.685148752559916,-5.65172729328823E-16,0.728403176040296));
#43860=DIRECTION('center_axis',(-3.66113466765132E-16,-1.,-1.12027918221652E-15));
#43861=DIRECTION('ref_axis',(5.46077161851015E-15,-1.12027918221652E-15,
1.));
#43862=DIRECTION('center_axis',(3.66113466765132E-16,1.,1.12027918221652E-15));
#43863=DIRECTION('ref_axis',(0.98443820279149,-1.63548173101491E-16,-0.175731115300228));
#43864=DIRECTION('center_axis',(3.66113466765132E-16,1.,1.12027918221652E-15));
#43865=DIRECTION('ref_axis',(0.456903875630426,-1.16378500342752E-15,0.889516075421853));
#43866=DIRECTION('center_axis',(3.66113466765132E-16,1.,1.12027918221652E-15));
#43867=DIRECTION('ref_axis',(-0.584211517032673,-6.95332497774842E-16,0.811601443669479));
#43868=DIRECTION('center_axis',(-3.66113466765132E-16,-1.,-1.12027918221652E-15));
#43869=DIRECTION('ref_axis',(5.46077161851015E-15,-1.12027918221652E-15,
1.));
#43870=DIRECTION('center_axis',(3.66113466765132E-16,1.,1.12027918221652E-15));
#43871=DIRECTION('ref_axis',(0.95307868416297,-9.80102327535809E-18,-0.302722681334224));
#43872=DIRECTION('center_axis',(3.66113466765132E-16,1.,1.12027918221652E-15));
#43873=DIRECTION('ref_axis',(0.569100145878903,-1.12952519527676E-15,0.822268218989772));
#43874=DIRECTION('center_axis',(3.66113466765132E-16,1.,1.12027918221652E-15));
#43875=DIRECTION('ref_axis',(-0.473278260474969,-8.13594934401345E-16,0.880912985579045));
#43876=DIRECTION('center_axis',(-3.66113466765132E-16,-1.,-1.12027918221652E-15));
#43877=DIRECTION('ref_axis',(5.46077161851015E-15,-1.12027918221652E-15,
1.));
#43878=DIRECTION('center_axis',(3.66113466765132E-16,1.,1.12027918221652E-15));
#43879=DIRECTION('ref_axis',(0.905411725005089,1.44113824776374E-16,-0.424534578360008));
#43880=DIRECTION('center_axis',(3.66113466765132E-16,1.,1.12027918221652E-15));
#43881=DIRECTION('ref_axis',(0.671558954847023,-1.07593889787127E-15,0.740951125354955));
#43882=DIRECTION('center_axis',(3.66113466765132E-16,1.,1.12027918221652E-15));
#43883=DIRECTION('ref_axis',(-0.354247081663014,-9.17936536129109E-16,0.935151862070134));
#43884=DIRECTION('center_axis',(-3.66113466765132E-16,-1.,-1.12027918221652E-15));
#43885=DIRECTION('ref_axis',(5.46077161851015E-15,-1.12027918221652E-15,
1.));
#43886=DIRECTION('center_axis',(3.66113466765132E-16,1.,1.12027918221652E-15));
#43887=DIRECTION('ref_axis',(0.842252920204816,2.9556284533028E-16,-0.53908257104683));
#43888=DIRECTION('center_axis',(3.66113466765132E-16,1.,1.12027918221652E-15));
#43889=DIRECTION('ref_axis',(0.762527203906392,-1.00394298761658E-15,0.646956152534853));
#43890=DIRECTION('center_axis',(3.66113466765132E-16,1.,1.12027918221652E-15));
#43891=DIRECTION('ref_axis',(-0.229154637067958,-1.00657198922362E-15,0.973390030928123));
#43892=DIRECTION('center_axis',(-3.66113466765132E-16,-1.,-1.12027918221652E-15));
#43893=DIRECTION('ref_axis',(5.46077161851015E-15,-1.12027918221652E-15,
1.));
#43894=DIRECTION('center_axis',(3.66113466765132E-16,1.,1.12027918221652E-15));
#43895=DIRECTION('ref_axis',(0.764682934423213,4.41954703655085E-16,-0.644406711481115));
#43896=DIRECTION('center_axis',(3.66113466765132E-16,1.,1.12027918221652E-15));
#43897=DIRECTION('ref_axis',(0.840448401094441,-9.14769334498193E-16,0.541891580574747));
#43898=DIRECTION('center_axis',(3.66113466765132E-16,1.,1.12027918221652E-15));
#43899=DIRECTION('ref_axis',(-0.100141293099002,-1.07798471650803E-15,0.994973226482231));
#43900=DIRECTION('center_axis',(-3.66113466765132E-16,-1.,-1.12027918221652E-15));
#43901=DIRECTION('ref_axis',(5.46077161851015E-15,-1.12027918221652E-15,
1.));
#43902=DIRECTION('center_axis',(3.66113466765132E-16,1.,1.12027918221652E-15));
#43903=DIRECTION('ref_axis',(0.674029011623465,5.80784594467357E-16,-0.738704874418665));
#43904=DIRECTION('center_axis',(3.66113466765132E-16,1.,1.12027918221652E-15));
#43905=DIRECTION('ref_axis',(0.903989293123446,-8.09943724444564E-16,0.427555093430276));
#43906=DIRECTION('center_axis',(3.66113466765132E-16,1.,1.12027918221652E-15));
#43907=DIRECTION('ref_axis',(0.0305854961592909,-1.13095282641916E-15,0.999532154272533));
#43908=DIRECTION('center_axis',(-3.66113466765132E-16,-1.,-1.12027918221652E-15));
#43909=DIRECTION('ref_axis',(5.46077161851015E-15,-1.12027918221652E-15,
1.));
#43910=DIRECTION('center_axis',(3.66113466765132E-16,1.,1.12027918221652E-15));
#43911=DIRECTION('ref_axis',(0.571842265558692,7.09677099844383E-16,-0.820363592147227));
#43912=DIRECTION('center_axis',(3.66113466765132E-16,1.,1.12027918221652E-15));
#43913=DIRECTION('ref_axis',(0.952062677713926,-6.91259752706864E-16,0.305903020096547));
#43914=DIRECTION('center_axis',(3.66113466765132E-16,1.,1.12027918221652E-15));
#43915=DIRECTION('ref_axis',(0.160788959098396,-1.1645700199109E-15,0.986988809780564));
#43916=DIRECTION('center_axis',(-3.66113466765132E-16,-1.,-1.12027918221652E-15));
#43917=DIRECTION('ref_axis',(5.46077161851015E-15,-1.12027918221652E-15,
1.));
#43918=DIRECTION('center_axis',(3.66113466765132E-16,1.,1.12027918221652E-15));
#43919=DIRECTION('ref_axis',(0.459871139785583,8.26426833283406E-16,-0.887985661366392));
#43920=DIRECTION('center_axis',(3.66113466765132E-16,1.,1.12027918221652E-15));
#43921=DIRECTION('ref_axis',(0.983846005927078,-5.60748134946939E-16,0.179016861276626));
#43922=DIRECTION('center_axis',(3.66113466765132E-16,1.,1.12027918221652E-15));
#43923=DIRECTION('ref_axis',(0.288241278368206,-1.17826109748215E-15,0.957557813108254));
#43924=DIRECTION('center_axis',(-3.66113466765132E-16,-1.,-1.12027918221652E-15));
#43925=DIRECTION('ref_axis',(5.46077161851015E-15,-1.12027918221652E-15,
1.));
#43926=DIRECTION('center_axis',(3.66113466765132E-16,1.,1.12027918221652E-15));
#43927=DIRECTION('ref_axis',(0.340031491310375,9.29036174476144E-16,-0.940414049723441));
#43928=DIRECTION('center_axis',(3.66113466765132E-16,1.,1.12027918221652E-15));
#43929=DIRECTION('ref_axis',(0.998795456205173,-4.20641961129317E-16,0.0490676743274118));
#43930=DIRECTION('center_axis',(3.66113466765132E-16,1.,1.12027918221652E-15));
#43931=DIRECTION('ref_axis',(0.410761709449557,-1.17179180099979E-15,0.91174273676848));
#43932=DIRECTION('center_axis',(-3.66113466765132E-16,-1.,-1.12027918221652E-15));
#43933=DIRECTION('ref_axis',(5.46077161851015E-15,-1.12027918221652E-15,
1.));
#43934=DIRECTION('center_axis',(3.66113466765132E-16,1.,1.12027918221652E-15));
#43935=DIRECTION('ref_axis',(0.214373809744306,1.01574944914611E-15,-0.976751692957689));
#43936=DIRECTION('center_axis',(3.66113466765132E-16,1.,1.12027918221652E-15));
#43937=DIRECTION('ref_axis',(0.99665523930918,-2.73338486732788E-16,-0.0817210741336743));
#43938=DIRECTION('center_axis',(3.66113466765132E-16,1.,1.12027918221652E-15));
#43939=DIRECTION('ref_axis',(0.526253893797564,-1.14527282192027E-15,0.850327489419754));
#43940=DIRECTION('center_axis',(-3.66113466765132E-16,-1.,-1.12027918221652E-15));
#43941=DIRECTION('ref_axis',(5.46077161851015E-15,-1.12027918221652E-15,
1.));
#43942=DIRECTION('center_axis',(3.66113466765132E-16,1.,1.12027918221652E-15));
#43943=DIRECTION('ref_axis',(0.0850481328578621,1.08508296912223E-15,-0.996376843918701));
#43944=DIRECTION('center_axis',(3.66113466765132E-16,1.,1.12027918221652E-15));
#43945=DIRECTION('ref_axis',(0.977461974943571,-1.21358115044515E-16,-0.211111552358971));
#43946=DIRECTION('center_axis',(3.66113466765132E-16,1.,1.12027918221652E-15));
#43947=DIRECTION('ref_axis',(0.63274172811755,-1.09915790732807E-15,0.774362902971737));
#43948=DIRECTION('center_axis',(-3.66113466765132E-16,-1.,-1.12027918221652E-15));
#43949=DIRECTION('ref_axis',(5.46077161851015E-15,-1.12027918221652E-15,
1.));
#43950=DIRECTION('center_axis',(3.66113466765132E-16,1.,1.12027918221652E-15));
#43951=DIRECTION('ref_axis',(-0.0457327411615761,1.13585041865483E-15,-0.998953710832413));
#43952=DIRECTION('center_axis',(3.66113466765132E-16,1.,1.12027918221652E-15));
#43953=DIRECTION('ref_axis',(0.941544065183019,3.2698727638996E-17,-0.336889853392226));
#43954=DIRECTION('center_axis',(3.66113466765132E-16,1.,1.12027918221652E-15));
#43955=DIRECTION('ref_axis',(0.728403176040296,-1.03423609619734E-15,0.685148752559917));
#43956=DIRECTION('center_axis',(-3.66113466765132E-16,-1.,-1.12027918221652E-15));
#43957=DIRECTION('ref_axis',(5.46077161851015E-15,-1.12027918221652E-15,
1.));
#43958=DIRECTION('center_axis',(3.66113466765132E-16,1.,1.12027918221652E-15));
#43959=DIRECTION('ref_axis',(-0.175731115300228,1.16718315260702E-15,-0.98443820279149));
#43960=DIRECTION('center_axis',(3.66113466765132E-16,1.,1.12027918221652E-15));
#43961=DIRECTION('ref_axis',(0.889516075421853,1.86196086026803E-16,-0.456903875630426));
#43962=DIRECTION('center_axis',(3.66113466765132E-16,1.,1.12027918221652E-15));
#43963=DIRECTION('ref_axis',(0.811601443669479,-9.51618218716256E-16,0.584211517032674));
#43964=DIRECTION('center_axis',(-3.66113466765132E-16,-1.,-1.12027918221652E-15));
#43965=DIRECTION('ref_axis',(5.46077161851015E-15,-1.12027918221652E-15,
1.));
#43966=DIRECTION('center_axis',(3.66113466765132E-16,1.,1.12027918221652E-15));
#43967=DIRECTION('ref_axis',(-0.302722681334224,1.1785450592138E-15,-0.95307868416297));
#43968=DIRECTION('center_axis',(3.66113466765132E-16,1.,1.12027918221652E-15));
#43969=DIRECTION('ref_axis',(0.822268218989772,3.36507577759385E-16,-0.569100145878903));
#43970=DIRECTION('center_axis',(3.66113466765132E-16,1.,1.12027918221652E-15));
#43971=DIRECTION('ref_axis',(0.880912985579045,-8.52717889674523E-16,0.473278260474969));
#43972=DIRECTION('center_axis',(-3.66113466765132E-16,-1.,-1.12027918221652E-15));
#43973=DIRECTION('ref_axis',(5.46077161851015E-15,-1.12027918221652E-15,
1.));
#43974=DIRECTION('center_axis',(3.66113466765132E-16,1.,1.12027918221652E-15));
#43975=DIRECTION('ref_axis',(-0.424534578360008,1.16974173310301E-15,-0.905411725005089));
#43976=DIRECTION('center_axis',(3.66113466765132E-16,1.,1.12027918221652E-15));
#43977=DIRECTION('ref_axis',(0.740951125354955,4.81061331538975E-16,-0.671558954847023));
#43978=DIRECTION('center_axis',(3.66113466765132E-16,1.,1.12027918221652E-15));
#43979=DIRECTION('ref_axis',(0.935151862070134,-7.39227321122395E-16,0.354247081663014));
#43980=DIRECTION('center_axis',(-3.66113466765132E-16,-1.,-1.12027918221652E-15));
#43981=DIRECTION('ref_axis',(5.46077161851015E-15,-1.12027918221652E-15,
1.));
#43982=DIRECTION('center_axis',(3.66113466765132E-16,1.,1.12027918221652E-15));
#43983=DIRECTION('ref_axis',(-0.53908257104683,1.14092380162514E-15,-0.842252920204816));
#43984=DIRECTION('center_axis',(3.66113466765132E-16,1.,1.12027918221652E-15));
#43985=DIRECTION('ref_axis',(0.646956152534853,6.17383992560536E-16,-0.762527203906392));
#43986=DIRECTION('center_axis',(3.66113466765132E-16,1.,1.12027918221652E-15));
#43987=DIRECTION('ref_axis',(0.973390030928123,-6.13088368153331E-16,0.229154637067959));
#43988=DIRECTION('center_axis',(-3.66113466765132E-16,-1.,-1.12027918221652E-15));
#43989=DIRECTION('ref_axis',(5.46077161851015E-15,-1.12027918221652E-15,
1.));
#43990=DIRECTION('center_axis',(3.66113466765132E-16,1.,1.12027918221652E-15));
#43991=DIRECTION('ref_axis',(-0.644406711481115,1.09258434757764E-15,-0.764682934423213));
#43992=DIRECTION('center_axis',(3.66113466765132E-16,1.,1.12027918221652E-15));
#43993=DIRECTION('ref_axis',(0.541891580574746,7.43143042298206E-16,-0.840448401094442));
#43994=DIRECTION('center_axis',(3.66113466765132E-16,1.,1.12027918221652E-15));
#43995=DIRECTION('ref_axis',(0.994973226482231,-4.76459303224953E-16,0.100141293099002));
#43996=DIRECTION('center_axis',(-3.66113466765132E-16,-1.,-1.12027918221652E-15));
#43997=DIRECTION('ref_axis',(5.46077161851015E-15,-1.12027918221652E-15,
1.));
#43998=DIRECTION('center_axis',(3.66113466765132E-16,1.,1.12027918221652E-15));
#43999=DIRECTION('ref_axis',(-0.738704874418665,1.02555047242146E-15,-0.674029011623465));
#44000=DIRECTION('center_axis',(3.66113466765132E-16,1.,1.12027918221652E-15));
#44001=DIRECTION('ref_axis',(0.427555093430276,8.56186708543976E-16,-0.903989293123446));
#44002=DIRECTION('center_axis',(3.66113466765132E-16,1.,1.12027918221652E-15));
#44003=DIRECTION('ref_axis',(0.999532154272533,-3.31677887518921E-16,-0.0305854961592909));
#44004=DIRECTION('center_axis',(-3.66113466765132E-16,-1.,-1.12027918221652E-15));
#44005=DIRECTION('ref_axis',(5.46077161851015E-15,-1.12027918221652E-15,
1.));
#44006=DIRECTION('center_axis',(3.66113466765132E-16,1.,1.12027918221652E-15));
#44007=DIRECTION('ref_axis',(-0.820363592147226,9.40969144345854E-16,-0.571842265558694));
#44008=DIRECTION('center_axis',(3.66113466765132E-16,1.,1.12027918221652E-15));
#44009=DIRECTION('ref_axis',(0.305903020096548,9.54580782826757E-16,-0.952062677713926));
#44010=DIRECTION('center_axis',(3.66113466765132E-16,1.,1.12027918221652E-15));
#44011=DIRECTION('ref_axis',(0.986988809780564,-1.81221371198957E-16,-0.160788959098396));
#44012=DIRECTION('center_axis',(-3.66113466765132E-16,-1.,-1.12027918221652E-15));
#44013=DIRECTION('ref_axis',(5.46077161851015E-15,-1.12027918221652E-15,
1.));
#44014=DIRECTION('center_axis',(3.66113466765132E-16,1.,1.12027918221652E-15));
#44015=DIRECTION('ref_axis',(-0.887985661366392,8.40287573324551E-16,-0.459871139785583));
#44016=DIRECTION('center_axis',(3.66113466765132E-16,1.,1.12027918221652E-15));
#44017=DIRECTION('ref_axis',(0.179016861276627,1.03664171525558E-15,-0.983846005927078));
#44018=DIRECTION('center_axis',(3.66113466765132E-16,1.,1.12027918221652E-15));
#44019=DIRECTION('ref_axis',(0.957557813108254,-2.76641069737229E-17,-0.288241278368206));
#44020=DIRECTION('center_axis',(-3.66113466765132E-16,-1.,-1.12027918221652E-15));
#44021=DIRECTION('ref_axis',(5.46077161851015E-15,-1.12027918221652E-15,
1.));
#44022=DIRECTION('center_axis',(3.66113466765132E-16,1.,1.12027918221652E-15));
#44023=DIRECTION('ref_axis',(-0.940414049723441,7.25228448951937E-16,-0.340031491310375));
#44024=DIRECTION('center_axis',(3.66113466765132E-16,1.,1.12027918221652E-15));
#44025=DIRECTION('ref_axis',(0.0490676743274116,1.100965420525E-15,-0.998795456205173));
#44026=DIRECTION('center_axis',(3.66113466765132E-16,1.,1.12027918221652E-15));
#44027=DIRECTION('ref_axis',(0.91174273676848,1.26366497791772E-16,-0.410761709449557));
#44028=DIRECTION('center_axis',(-3.66113466765132E-16,-1.,-1.12027918221652E-15));
#44029=DIRECTION('ref_axis',(5.46077161851015E-15,-1.12027918221652E-15,
1.));
#44030=DIRECTION('center_axis',(3.66113466765132E-16,1.,1.12027918221652E-15));
#44031=DIRECTION('ref_axis',(-0.976751692957689,5.97760464746442E-16,-0.214373809744306));
#44032=DIRECTION('center_axis',(3.66113466765132E-16,1.,1.12027918221652E-15));
#44033=DIRECTION('ref_axis',(-0.081721074133674,1.14645130220395E-15,-0.99665523930918));
#44034=DIRECTION('center_axis',(3.66113466765132E-16,1.,1.12027918221652E-15));
#44035=DIRECTION('ref_axis',(0.850327489419755,2.78234936744635E-16,-0.526253893797563));
#44036=DIRECTION('center_axis',(-3.66113466765132E-16,-1.,-1.12027918221652E-15));
#44037=DIRECTION('ref_axis',(5.46077161851015E-15,-1.12027918221652E-15,
1.));
#44038=DIRECTION('center_axis',(3.66113466765132E-16,1.,1.12027918221652E-15));
#44039=DIRECTION('ref_axis',(-0.996376843918701,4.60064633258625E-16,-0.0850481328578625));
#44040=DIRECTION('center_axis',(3.66113466765132E-16,1.,1.12027918221652E-15));
#44041=DIRECTION('ref_axis',(-0.211111552358971,1.17232108424584E-15,-0.977461974943571));
#44042=DIRECTION('center_axis',(3.66113466765132E-16,1.,1.12027918221652E-15));
#44043=DIRECTION('ref_axis',(0.774362902971737,4.25342698788503E-16,-0.63274172811755));
#44044=DIRECTION('center_axis',(-3.66113466765132E-16,-1.,-1.12027918221652E-15));
#44045=DIRECTION('ref_axis',(5.46077161851015E-15,-1.12027918221652E-15,
1.));
#44046=DIRECTION('center_axis',(3.66113466765132E-16,1.,1.12027918221652E-15));
#44047=DIRECTION('ref_axis',(-0.998953710832413,3.14496968341738E-16,0.045732741161576));
#44048=DIRECTION('center_axis',(3.66113466765132E-16,1.,1.12027918221652E-15));
#44049=DIRECTION('ref_axis',(-0.336889853392226,1.17813212750748E-15,-0.941544065183019));
#44050=DIRECTION('center_axis',(3.66113466765132E-16,1.,1.12027918221652E-15));
#44051=DIRECTION('ref_axis',(0.685148752559917,5.65172729328822E-16,-0.728403176040296));
#44052=DIRECTION('center_axis',(-3.66113466765132E-16,-1.,-1.12027918221652E-15));
#44053=DIRECTION('ref_axis',(5.46077161851015E-15,-1.12027918221652E-15,
1.));
#44054=DIRECTION('center_axis',(3.66113466765132E-16,1.,1.12027918221652E-15));
#44055=DIRECTION('ref_axis',(-0.98443820279149,1.63548173101491E-16,0.175731115300228));
#44056=DIRECTION('center_axis',(3.66113466765132E-16,1.,1.12027918221652E-15));
#44057=DIRECTION('ref_axis',(-0.456903875630426,1.16378500342752E-15,-0.889516075421853));
#44058=DIRECTION('center_axis',(3.66113466765132E-16,1.,1.12027918221652E-15));
#44059=DIRECTION('ref_axis',(0.584211517032674,6.95332497774842E-16,-0.811601443669479));
#44060=DIRECTION('center_axis',(-3.66113466765132E-16,-1.,-1.12027918221652E-15));
#44061=DIRECTION('ref_axis',(5.46077161851015E-15,-1.12027918221652E-15,
1.));
#44062=DIRECTION('center_axis',(3.66113466765132E-16,1.,1.12027918221652E-15));
#44063=DIRECTION('ref_axis',(-0.95307868416297,9.80102327535809E-18,0.302722681334224));
#44064=DIRECTION('center_axis',(3.66113466765132E-16,1.,1.12027918221652E-15));
#44065=DIRECTION('ref_axis',(-0.569100145878903,1.12952519527676E-15,-0.822268218989772));
#44066=DIRECTION('center_axis',(3.66113466765132E-16,1.,1.12027918221652E-15));
#44067=DIRECTION('ref_axis',(0.473278260474969,8.13594934401345E-16,-0.880912985579045));
#44068=DIRECTION('center_axis',(-3.66113466765132E-16,-1.,-1.12027918221652E-15));
#44069=DIRECTION('ref_axis',(5.46077161851015E-15,-1.12027918221652E-15,
1.));
#44070=DIRECTION('center_axis',(3.66113466765132E-16,1.,1.12027918221652E-15));
#44071=DIRECTION('ref_axis',(-0.905411725005089,-1.44113824776374E-16,0.424534578360008));
#44072=DIRECTION('center_axis',(3.66113466765132E-16,1.,1.12027918221652E-15));
#44073=DIRECTION('ref_axis',(-0.671558954847023,1.07593889787127E-15,-0.740951125354955));
#44074=DIRECTION('center_axis',(3.66113466765132E-16,1.,1.12027918221652E-15));
#44075=DIRECTION('ref_axis',(0.354247081663014,9.17936536129109E-16,-0.935151862070134));
#44076=DIRECTION('center_axis',(-3.66113466765132E-16,-1.,-1.12027918221652E-15));
#44077=DIRECTION('ref_axis',(5.46077161851015E-15,-1.12027918221652E-15,
1.));
#44078=DIRECTION('center_axis',(3.66113466765132E-16,1.,1.12027918221652E-15));
#44079=DIRECTION('ref_axis',(-0.842252920204816,-2.9556284533028E-16,0.53908257104683));
#44080=DIRECTION('center_axis',(3.66113466765132E-16,1.,1.12027918221652E-15));
#44081=DIRECTION('ref_axis',(-0.762527203906392,1.00394298761658E-15,-0.646956152534853));
#44082=DIRECTION('center_axis',(3.66113466765132E-16,1.,1.12027918221652E-15));
#44083=DIRECTION('ref_axis',(0.229154637067959,1.00657198922362E-15,-0.973390030928123));
#44084=DIRECTION('center_axis',(-3.66113466765132E-16,-1.,-1.12027918221652E-15));
#44085=DIRECTION('ref_axis',(5.46077161851015E-15,-1.12027918221652E-15,
1.));
#44086=DIRECTION('center_axis',(3.66113466765132E-16,1.,1.12027918221652E-15));
#44087=DIRECTION('ref_axis',(-0.764682934423213,-4.41954703655085E-16,0.644406711481115));
#44088=DIRECTION('center_axis',(3.66113466765132E-16,1.,1.12027918221652E-15));
#44089=DIRECTION('ref_axis',(-0.840448401094441,9.14769334498193E-16,-0.541891580574747));
#44090=DIRECTION('center_axis',(3.66113466765132E-16,1.,1.12027918221652E-15));
#44091=DIRECTION('ref_axis',(0.100141293099002,1.07798471650803E-15,-0.994973226482231));
#44092=DIRECTION('center_axis',(-3.66113466765132E-16,-1.,-1.12027918221652E-15));
#44093=DIRECTION('ref_axis',(5.46077161851015E-15,-1.12027918221652E-15,
1.));
#44094=DIRECTION('center_axis',(3.66113466765132E-16,1.,1.12027918221652E-15));
#44095=DIRECTION('ref_axis',(-0.674029011623465,-5.80784594467357E-16,0.738704874418665));
#44096=DIRECTION('center_axis',(3.66113466765132E-16,1.,1.12027918221652E-15));
#44097=DIRECTION('ref_axis',(-0.903989293123446,8.09943724444565E-16,-0.427555093430277));
#44098=DIRECTION('center_axis',(3.66113466765132E-16,1.,1.12027918221652E-15));
#44099=DIRECTION('ref_axis',(-0.0305854961592907,1.13095282641916E-15,-0.999532154272533));
#44100=DIRECTION('center_axis',(-3.66113466765132E-16,-1.,-1.12027918221652E-15));
#44101=DIRECTION('ref_axis',(5.46077161851015E-15,-1.12027918221652E-15,
1.));
#44102=DIRECTION('center_axis',(3.66113466765132E-16,1.,1.12027918221652E-15));
#44103=DIRECTION('ref_axis',(-0.571842265558694,-7.09677099844381E-16,0.820363592147226));
#44104=DIRECTION('center_axis',(3.66113466765132E-16,1.,1.12027918221652E-15));
#44105=DIRECTION('ref_axis',(-0.952062677713926,6.91259752706865E-16,-0.305903020096548));
#44106=DIRECTION('center_axis',(3.66113466765132E-16,1.,1.12027918221652E-15));
#44107=DIRECTION('ref_axis',(-0.160788959098396,1.1645700199109E-15,-0.986988809780564));
#44108=DIRECTION('center_axis',(-3.66113466765132E-16,-1.,-1.12027918221652E-15));
#44109=DIRECTION('ref_axis',(5.46077161851015E-15,-1.12027918221652E-15,
1.));
#44110=DIRECTION('center_axis',(3.66113466765132E-16,1.,1.12027918221652E-15));
#44111=DIRECTION('ref_axis',(-0.459871139785583,-8.26426833283405E-16,0.887985661366392));
#44112=DIRECTION('center_axis',(3.66113466765132E-16,1.,1.12027918221652E-15));
#44113=DIRECTION('ref_axis',(-0.983846005927078,5.60748134946939E-16,-0.179016861276627));
#44114=DIRECTION('center_axis',(3.66113466765132E-16,1.,1.12027918221652E-15));
#44115=DIRECTION('ref_axis',(-0.288241278368206,1.17826109748215E-15,-0.957557813108254));
#44116=DIRECTION('center_axis',(-3.66113466765132E-16,-1.,-1.12027918221652E-15));
#44117=DIRECTION('ref_axis',(5.46077161851015E-15,-1.12027918221652E-15,
1.));
#44118=DIRECTION('center_axis',(3.66113466765132E-16,1.,1.12027918221652E-15));
#44119=DIRECTION('ref_axis',(-0.340031491310375,-9.29036174476144E-16,0.940414049723441));
#44120=DIRECTION('center_axis',(3.66113466765132E-16,1.,1.12027918221652E-15));
#44121=DIRECTION('ref_axis',(-0.998795456205173,4.20641961129317E-16,-0.0490676743274121));
#44122=DIRECTION('center_axis',(3.66113466765132E-16,1.,1.12027918221652E-15));
#44123=DIRECTION('ref_axis',(-0.410761709449556,1.17179180099979E-15,-0.91174273676848));
#44124=DIRECTION('center_axis',(-3.66113466765132E-16,-1.,-1.12027918221652E-15));
#44125=DIRECTION('ref_axis',(5.46077161851015E-15,-1.12027918221652E-15,
1.));
#44126=DIRECTION('center_axis',(3.66113466765132E-16,1.,1.12027918221652E-15));
#44127=DIRECTION('ref_axis',(-0.214373809744306,-1.01574944914611E-15,0.976751692957689));
#44128=DIRECTION('center_axis',(3.66113466765132E-16,1.,1.12027918221652E-15));
#44129=DIRECTION('ref_axis',(-0.99665523930918,2.73338486732788E-16,0.0817210741336742));
#44130=DIRECTION('center_axis',(3.66113466765132E-16,1.,1.12027918221652E-15));
#44131=DIRECTION('ref_axis',(-0.526253893797564,1.14527282192027E-15,-0.850327489419754));
#44132=DIRECTION('center_axis',(-3.66113466765132E-16,-1.,-1.12027918221652E-15));
#44133=DIRECTION('ref_axis',(5.46077161851015E-15,-1.12027918221652E-15,
1.));
#44134=DIRECTION('center_axis',(1.,-3.66113466765126E-16,-5.46077161851015E-15));
#44135=DIRECTION('ref_axis',(5.46077161851015E-15,-1.12027918221652E-15,
1.));
#44136=DIRECTION('',(-5.46077161851015E-15,1.12027918221652E-15,-1.));
#44137=DIRECTION('',(-3.66113466765132E-16,-1.,-1.12027918221652E-15));
#44138=DIRECTION('',(-3.66113466765132E-16,-1.,-1.12027918221652E-15));
#44139=DIRECTION('center_axis',(-5.46077161851015E-15,1.12027918221652E-15,
-1.));
#44140=DIRECTION('ref_axis',(1.,-3.66113466765126E-16,-5.46077161851015E-15));
#44141=DIRECTION('',(-1.,3.66113466765126E-16,5.46077161851015E-15));
#44142=DIRECTION('',(3.66113466765132E-16,1.,1.12027918221652E-15));
#44143=DIRECTION('center_axis',(-3.66113466765132E-16,-1.,-1.12027918221652E-15));
#44144=DIRECTION('ref_axis',(-1.,3.66113466765124E-16,6.8542715880177E-15));
#44145=DIRECTION('center_axis',(3.66113466765132E-16,1.,1.12027918221652E-15));
#44146=DIRECTION('ref_axis',(5.46077161851015E-15,-1.12027918221652E-15,
1.));
#44147=DIRECTION('',(-3.66113466765132E-16,-1.,-1.12027918221652E-15));
#44148=DIRECTION('center_axis',(5.46077161851015E-15,-1.12027918221652E-15,
1.));
#44149=DIRECTION('ref_axis',(-1.,3.66113466765126E-16,5.46077161851015E-15));
#44150=DIRECTION('',(1.,-3.66113466765126E-16,-5.46077161851015E-15));
#44151=DIRECTION('center_axis',(3.66113466765132E-16,1.,1.12027918221652E-15));
#44152=DIRECTION('ref_axis',(-0.97746197494357,1.21358115044514E-16,0.211111552358972));
#44153=DIRECTION('',(3.66113466765132E-16,1.,1.12027918221652E-15));
#44154=DIRECTION('center_axis',(-3.66113466765132E-16,-1.,-1.12027918221652E-15));
#44155=DIRECTION('ref_axis',(-0.97746197494357,1.21358115044514E-16,0.211111552358972));
#44156=DIRECTION('',(3.66113466765132E-16,1.,1.12027918221652E-15));
#44157=DIRECTION('center_axis',(3.66113466765132E-16,1.,1.12027918221652E-15));
#44158=DIRECTION('ref_axis',(-0.632741728117551,1.09915790732807E-15,-0.774362902971737));
#44159=DIRECTION('center_axis',(-3.66113466765132E-16,-1.,-1.12027918221652E-15));
#44160=DIRECTION('ref_axis',(-0.632741728117551,1.09915790732807E-15,-0.774362902971737));
#44161=DIRECTION('',(-3.66113466765132E-16,-1.,-1.12027918221652E-15));
#44162=DIRECTION('center_axis',(3.66113466765132E-16,1.,1.12027918221652E-15));
#44163=DIRECTION('ref_axis',(-0.0850481328578615,-1.08508296912223E-15,
0.996376843918701));
#44164=DIRECTION('',(3.66113466765132E-16,1.,1.12027918221652E-15));
#44165=DIRECTION('center_axis',(-3.66113466765132E-16,-1.,-1.12027918221652E-15));
#44166=DIRECTION('ref_axis',(-0.0850481328578615,-1.08508296912223E-15,
0.996376843918701));
#44167=DIRECTION('center_axis',(3.66113466765132E-16,1.,1.12027918221652E-15));
#44168=DIRECTION('ref_axis',(-0.941544065183018,-3.26987276389964E-17,0.336889853392226));
#44169=DIRECTION('',(3.66113466765132E-16,1.,1.12027918221652E-15));
#44170=DIRECTION('center_axis',(-3.66113466765132E-16,-1.,-1.12027918221652E-15));
#44171=DIRECTION('ref_axis',(-0.941544065183018,-3.26987276389964E-17,0.336889853392226));
#44172=DIRECTION('',(3.66113466765132E-16,1.,1.12027918221652E-15));
#44173=DIRECTION('center_axis',(3.66113466765132E-16,1.,1.12027918221652E-15));
#44174=DIRECTION('ref_axis',(-0.728403176040296,1.03423609619734E-15,-0.685148752559916));
#44175=DIRECTION('center_axis',(-3.66113466765132E-16,-1.,-1.12027918221652E-15));
#44176=DIRECTION('ref_axis',(-0.728403176040296,1.03423609619734E-15,-0.685148752559916));
#44177=DIRECTION('',(-3.66113466765132E-16,-1.,-1.12027918221652E-15));
#44178=DIRECTION('center_axis',(3.66113466765132E-16,1.,1.12027918221652E-15));
#44179=DIRECTION('ref_axis',(0.0457327411615766,-1.13585041865483E-15,0.998953710832413));
#44180=DIRECTION('',(3.66113466765132E-16,1.,1.12027918221652E-15));
#44181=DIRECTION('center_axis',(-3.66113466765132E-16,-1.,-1.12027918221652E-15));
#44182=DIRECTION('ref_axis',(0.0457327411615766,-1.13585041865483E-15,0.998953710832413));
#44183=DIRECTION('center_axis',(3.66113466765132E-16,1.,1.12027918221652E-15));
#44184=DIRECTION('ref_axis',(-0.889516075421853,-1.86196086026804E-16,0.456903875630427));
#44185=DIRECTION('',(3.66113466765132E-16,1.,1.12027918221652E-15));
#44186=DIRECTION('center_axis',(-3.66113466765132E-16,-1.,-1.12027918221652E-15));
#44187=DIRECTION('ref_axis',(-0.889516075421853,-1.86196086026804E-16,0.456903875630427));
#44188=DIRECTION('',(3.66113466765132E-16,1.,1.12027918221652E-15));
#44189=DIRECTION('center_axis',(3.66113466765132E-16,1.,1.12027918221652E-15));
#44190=DIRECTION('ref_axis',(-0.811601443669479,9.51618218716255E-16,-0.584211517032673));
#44191=DIRECTION('center_axis',(-3.66113466765132E-16,-1.,-1.12027918221652E-15));
#44192=DIRECTION('ref_axis',(-0.811601443669479,9.51618218716255E-16,-0.584211517032673));
#44193=DIRECTION('',(-3.66113466765132E-16,-1.,-1.12027918221652E-15));
#44194=DIRECTION('center_axis',(3.66113466765132E-16,1.,1.12027918221652E-15));
#44195=DIRECTION('ref_axis',(0.175731115300229,-1.16718315260702E-15,0.984438202791489));
#44196=DIRECTION('',(3.66113466765132E-16,1.,1.12027918221652E-15));
#44197=DIRECTION('center_axis',(-3.66113466765132E-16,-1.,-1.12027918221652E-15));
#44198=DIRECTION('ref_axis',(0.175731115300229,-1.16718315260702E-15,0.984438202791489));
#44199=DIRECTION('center_axis',(3.66113466765132E-16,1.,1.12027918221652E-15));
#44200=DIRECTION('ref_axis',(-0.822268218989772,-3.36507577759385E-16,0.569100145878903));
#44201=DIRECTION('',(3.66113466765132E-16,1.,1.12027918221652E-15));
#44202=DIRECTION('center_axis',(-3.66113466765132E-16,-1.,-1.12027918221652E-15));
#44203=DIRECTION('ref_axis',(-0.822268218989772,-3.36507577759385E-16,0.569100145878903));
#44204=DIRECTION('',(3.66113466765132E-16,1.,1.12027918221652E-15));
#44205=DIRECTION('center_axis',(3.66113466765132E-16,1.,1.12027918221652E-15));
#44206=DIRECTION('ref_axis',(-0.880912985579045,8.52717889674523E-16,-0.473278260474969));
#44207=DIRECTION('center_axis',(-3.66113466765132E-16,-1.,-1.12027918221652E-15));
#44208=DIRECTION('ref_axis',(-0.880912985579045,8.52717889674523E-16,-0.473278260474969));
#44209=DIRECTION('',(-3.66113466765132E-16,-1.,-1.12027918221652E-15));
#44210=DIRECTION('center_axis',(3.66113466765132E-16,1.,1.12027918221652E-15));
#44211=DIRECTION('ref_axis',(0.302722681334224,-1.1785450592138E-15,0.95307868416297));
#44212=DIRECTION('',(3.66113466765132E-16,1.,1.12027918221652E-15));
#44213=DIRECTION('center_axis',(-3.66113466765132E-16,-1.,-1.12027918221652E-15));
#44214=DIRECTION('ref_axis',(0.302722681334224,-1.1785450592138E-15,0.95307868416297));
#44215=DIRECTION('center_axis',(3.66113466765132E-16,1.,1.12027918221652E-15));
#44216=DIRECTION('ref_axis',(-0.740951125354955,-4.81061331538975E-16,0.671558954847023));
#44217=DIRECTION('',(3.66113466765132E-16,1.,1.12027918221652E-15));
#44218=DIRECTION('center_axis',(-3.66113466765132E-16,-1.,-1.12027918221652E-15));
#44219=DIRECTION('ref_axis',(-0.740951125354955,-4.81061331538975E-16,0.671558954847023));
#44220=DIRECTION('',(3.66113466765132E-16,1.,1.12027918221652E-15));
#44221=DIRECTION('center_axis',(3.66113466765132E-16,1.,1.12027918221652E-15));
#44222=DIRECTION('ref_axis',(-0.935151862070134,7.39227321122395E-16,-0.354247081663014));
#44223=DIRECTION('center_axis',(-3.66113466765132E-16,-1.,-1.12027918221652E-15));
#44224=DIRECTION('ref_axis',(-0.935151862070134,7.39227321122395E-16,-0.354247081663014));
#44225=DIRECTION('',(-3.66113466765132E-16,-1.,-1.12027918221652E-15));
#44226=DIRECTION('center_axis',(3.66113466765132E-16,1.,1.12027918221652E-15));
#44227=DIRECTION('ref_axis',(0.424534578360008,-1.16974173310301E-15,0.905411725005089));
#44228=DIRECTION('',(3.66113466765132E-16,1.,1.12027918221652E-15));
#44229=DIRECTION('center_axis',(-3.66113466765132E-16,-1.,-1.12027918221652E-15));
#44230=DIRECTION('ref_axis',(0.424534578360008,-1.16974173310301E-15,0.905411725005089));
#44231=DIRECTION('center_axis',(3.66113466765132E-16,1.,1.12027918221652E-15));
#44232=DIRECTION('ref_axis',(-0.646956152534853,-6.17383992560537E-16,0.762527203906392));
#44233=DIRECTION('',(3.66113466765132E-16,1.,1.12027918221652E-15));
#44234=DIRECTION('center_axis',(-3.66113466765132E-16,-1.,-1.12027918221652E-15));
#44235=DIRECTION('ref_axis',(-0.646956152534853,-6.17383992560537E-16,0.762527203906392));
#44236=DIRECTION('',(3.66113466765132E-16,1.,1.12027918221652E-15));
#44237=DIRECTION('center_axis',(3.66113466765132E-16,1.,1.12027918221652E-15));
#44238=DIRECTION('ref_axis',(-0.973390030928123,6.13088368153331E-16,-0.229154637067959));
#44239=DIRECTION('center_axis',(-3.66113466765132E-16,-1.,-1.12027918221652E-15));
#44240=DIRECTION('ref_axis',(-0.973390030928123,6.13088368153331E-16,-0.229154637067959));
#44241=DIRECTION('',(-3.66113466765132E-16,-1.,-1.12027918221652E-15));
#44242=DIRECTION('center_axis',(3.66113466765132E-16,1.,1.12027918221652E-15));
#44243=DIRECTION('ref_axis',(0.53908257104683,-1.14092380162514E-15,0.842252920204816));
#44244=DIRECTION('',(3.66113466765132E-16,1.,1.12027918221652E-15));
#44245=DIRECTION('center_axis',(-3.66113466765132E-16,-1.,-1.12027918221652E-15));
#44246=DIRECTION('ref_axis',(0.53908257104683,-1.14092380162514E-15,0.842252920204816));
#44247=DIRECTION('center_axis',(3.66113466765132E-16,1.,1.12027918221652E-15));
#44248=DIRECTION('ref_axis',(-0.541891580574746,-7.43143042298206E-16,0.840448401094442));
#44249=DIRECTION('',(3.66113466765132E-16,1.,1.12027918221652E-15));
#44250=DIRECTION('center_axis',(-3.66113466765132E-16,-1.,-1.12027918221652E-15));
#44251=DIRECTION('ref_axis',(-0.541891580574746,-7.43143042298206E-16,0.840448401094442));
#44252=DIRECTION('',(3.66113466765132E-16,1.,1.12027918221652E-15));
#44253=DIRECTION('center_axis',(3.66113466765132E-16,1.,1.12027918221652E-15));
#44254=DIRECTION('ref_axis',(-0.994973226482231,4.76459303224952E-16,-0.100141293099001));
#44255=DIRECTION('center_axis',(-3.66113466765132E-16,-1.,-1.12027918221652E-15));
#44256=DIRECTION('ref_axis',(-0.994973226482231,4.76459303224952E-16,-0.100141293099001));
#44257=DIRECTION('',(-3.66113466765132E-16,-1.,-1.12027918221652E-15));
#44258=DIRECTION('center_axis',(3.66113466765132E-16,1.,1.12027918221652E-15));
#44259=DIRECTION('ref_axis',(0.644406711481115,-1.09258434757764E-15,0.764682934423213));
#44260=DIRECTION('',(3.66113466765132E-16,1.,1.12027918221652E-15));
#44261=DIRECTION('center_axis',(-3.66113466765132E-16,-1.,-1.12027918221652E-15));
#44262=DIRECTION('ref_axis',(0.644406711481115,-1.09258434757764E-15,0.764682934423213));
#44263=DIRECTION('center_axis',(3.66113466765132E-16,1.,1.12027918221652E-15));
#44264=DIRECTION('ref_axis',(-0.427555093430276,-8.56186708543976E-16,0.903989293123446));
#44265=DIRECTION('',(3.66113466765132E-16,1.,1.12027918221652E-15));
#44266=DIRECTION('center_axis',(-3.66113466765132E-16,-1.,-1.12027918221652E-15));
#44267=DIRECTION('ref_axis',(-0.427555093430276,-8.56186708543976E-16,0.903989293123446));
#44268=DIRECTION('',(3.66113466765132E-16,1.,1.12027918221652E-15));
#44269=DIRECTION('center_axis',(3.66113466765132E-16,1.,1.12027918221652E-15));
#44270=DIRECTION('ref_axis',(-0.999532154272533,3.3167788751892E-16,0.0305854961592914));
#44271=DIRECTION('center_axis',(-3.66113466765132E-16,-1.,-1.12027918221652E-15));
#44272=DIRECTION('ref_axis',(-0.999532154272533,3.3167788751892E-16,0.0305854961592914));
#44273=DIRECTION('',(-3.66113466765132E-16,-1.,-1.12027918221652E-15));
#44274=DIRECTION('center_axis',(3.66113466765132E-16,1.,1.12027918221652E-15));
#44275=DIRECTION('ref_axis',(0.738704874418665,-1.02555047242146E-15,0.674029011623465));
#44276=DIRECTION('',(3.66113466765132E-16,1.,1.12027918221652E-15));
#44277=DIRECTION('center_axis',(-3.66113466765132E-16,-1.,-1.12027918221652E-15));
#44278=DIRECTION('ref_axis',(0.738704874418665,-1.02555047242146E-15,0.674029011623465));
#44279=DIRECTION('center_axis',(3.66113466765132E-16,1.,1.12027918221652E-15));
#44280=DIRECTION('ref_axis',(-0.305903020096547,-9.54580782826758E-16,0.952062677713926));
#44281=DIRECTION('',(3.66113466765132E-16,1.,1.12027918221652E-15));
#44282=DIRECTION('center_axis',(-3.66113466765132E-16,-1.,-1.12027918221652E-15));
#44283=DIRECTION('ref_axis',(-0.305903020096547,-9.54580782826758E-16,0.952062677713926));
#44284=DIRECTION('',(3.66113466765132E-16,1.,1.12027918221652E-15));
#44285=DIRECTION('center_axis',(3.66113466765132E-16,1.,1.12027918221652E-15));
#44286=DIRECTION('ref_axis',(-0.986988809780564,1.81221371198957E-16,0.160788959098396));
#44287=DIRECTION('center_axis',(-3.66113466765132E-16,-1.,-1.12027918221652E-15));
#44288=DIRECTION('ref_axis',(-0.986988809780564,1.81221371198957E-16,0.160788959098396));
#44289=DIRECTION('',(-3.66113466765132E-16,-1.,-1.12027918221652E-15));
#44290=DIRECTION('center_axis',(3.66113466765132E-16,1.,1.12027918221652E-15));
#44291=DIRECTION('ref_axis',(0.820363592147227,-9.40969144345853E-16,0.571842265558692));
#44292=DIRECTION('',(3.66113466765132E-16,1.,1.12027918221652E-15));
#44293=DIRECTION('center_axis',(-3.66113466765132E-16,-1.,-1.12027918221652E-15));
#44294=DIRECTION('ref_axis',(0.820363592147227,-9.40969144345853E-16,0.571842265558692));
#44295=DIRECTION('center_axis',(3.66113466765132E-16,1.,1.12027918221652E-15));
#44296=DIRECTION('ref_axis',(-0.179016861276626,-1.03664171525558E-15,0.983846005927078));
#44297=DIRECTION('',(3.66113466765132E-16,1.,1.12027918221652E-15));
#44298=DIRECTION('center_axis',(-3.66113466765132E-16,-1.,-1.12027918221652E-15));
#44299=DIRECTION('ref_axis',(-0.179016861276626,-1.03664171525558E-15,0.983846005927078));
#44300=DIRECTION('',(3.66113466765132E-16,1.,1.12027918221652E-15));
#44301=DIRECTION('center_axis',(3.66113466765132E-16,1.,1.12027918221652E-15));
#44302=DIRECTION('ref_axis',(-0.957557813108254,2.76641069737215E-17,0.288241278368207));
#44303=DIRECTION('center_axis',(-3.66113466765132E-16,-1.,-1.12027918221652E-15));
#44304=DIRECTION('ref_axis',(-0.957557813108254,2.76641069737215E-17,0.288241278368207));
#44305=DIRECTION('',(-3.66113466765132E-16,-1.,-1.12027918221652E-15));
#44306=DIRECTION('center_axis',(3.66113466765132E-16,1.,1.12027918221652E-15));
#44307=DIRECTION('ref_axis',(0.887985661366392,-8.40287573324551E-16,0.459871139785583));
#44308=DIRECTION('',(3.66113466765132E-16,1.,1.12027918221652E-15));
#44309=DIRECTION('center_axis',(-3.66113466765132E-16,-1.,-1.12027918221652E-15));
#44310=DIRECTION('ref_axis',(0.887985661366392,-8.40287573324551E-16,0.459871139785583));
#44311=DIRECTION('center_axis',(3.66113466765132E-16,1.,1.12027918221652E-15));
#44312=DIRECTION('ref_axis',(-0.0490676743274118,-1.100965420525E-15,0.998795456205173));
#44313=DIRECTION('',(3.66113466765132E-16,1.,1.12027918221652E-15));
#44314=DIRECTION('center_axis',(-3.66113466765132E-16,-1.,-1.12027918221652E-15));
#44315=DIRECTION('ref_axis',(-0.0490676743274118,-1.100965420525E-15,0.998795456205173));
#44316=DIRECTION('',(3.66113466765132E-16,1.,1.12027918221652E-15));
#44317=DIRECTION('center_axis',(3.66113466765132E-16,1.,1.12027918221652E-15));
#44318=DIRECTION('ref_axis',(-0.91174273676848,-1.26366497791772E-16,0.410761709449557));
#44319=DIRECTION('center_axis',(-3.66113466765132E-16,-1.,-1.12027918221652E-15));
#44320=DIRECTION('ref_axis',(-0.91174273676848,-1.26366497791772E-16,0.410761709449557));
#44321=DIRECTION('',(-3.66113466765132E-16,-1.,-1.12027918221652E-15));
#44322=DIRECTION('center_axis',(3.66113466765132E-16,1.,1.12027918221652E-15));
#44323=DIRECTION('ref_axis',(0.940414049723441,-7.25228448951937E-16,0.340031491310375));
#44324=DIRECTION('',(3.66113466765132E-16,1.,1.12027918221652E-15));
#44325=DIRECTION('center_axis',(-3.66113466765132E-16,-1.,-1.12027918221652E-15));
#44326=DIRECTION('ref_axis',(0.940414049723441,-7.25228448951937E-16,0.340031491310375));
#44327=DIRECTION('center_axis',(3.66113466765132E-16,1.,1.12027918221652E-15));
#44328=DIRECTION('ref_axis',(0.0817210741336744,-1.14645130220395E-15,0.99665523930918));
#44329=DIRECTION('',(3.66113466765132E-16,1.,1.12027918221652E-15));
#44330=DIRECTION('center_axis',(-3.66113466765132E-16,-1.,-1.12027918221652E-15));
#44331=DIRECTION('ref_axis',(0.0817210741336744,-1.14645130220395E-15,0.99665523930918));
#44332=DIRECTION('',(3.66113466765132E-16,1.,1.12027918221652E-15));
#44333=DIRECTION('center_axis',(3.66113466765132E-16,1.,1.12027918221652E-15));
#44334=DIRECTION('ref_axis',(-0.850327489419754,-2.78234936744637E-16,0.526253893797564));
#44335=DIRECTION('center_axis',(-3.66113466765132E-16,-1.,-1.12027918221652E-15));
#44336=DIRECTION('ref_axis',(-0.850327489419754,-2.78234936744637E-16,0.526253893797564));
#44337=DIRECTION('',(-3.66113466765132E-16,-1.,-1.12027918221652E-15));
#44338=DIRECTION('center_axis',(3.66113466765132E-16,1.,1.12027918221652E-15));
#44339=DIRECTION('ref_axis',(0.976751692957689,-5.97760464746442E-16,0.214373809744306));
#44340=DIRECTION('',(3.66113466765132E-16,1.,1.12027918221652E-15));
#44341=DIRECTION('center_axis',(-3.66113466765132E-16,-1.,-1.12027918221652E-15));
#44342=DIRECTION('ref_axis',(0.976751692957689,-5.97760464746442E-16,0.214373809744306));
#44343=DIRECTION('center_axis',(3.66113466765132E-16,1.,1.12027918221652E-15));
#44344=DIRECTION('ref_axis',(0.211111552358972,-1.17232108424584E-15,0.97746197494357));
#44345=DIRECTION('',(3.66113466765132E-16,1.,1.12027918221652E-15));
#44346=DIRECTION('center_axis',(-3.66113466765132E-16,-1.,-1.12027918221652E-15));
#44347=DIRECTION('ref_axis',(0.211111552358972,-1.17232108424584E-15,0.97746197494357));
#44348=DIRECTION('',(3.66113466765132E-16,1.,1.12027918221652E-15));
#44349=DIRECTION('center_axis',(3.66113466765132E-16,1.,1.12027918221652E-15));
#44350=DIRECTION('ref_axis',(-0.774362902971737,-4.25342698788503E-16,0.632741728117551));
#44351=DIRECTION('center_axis',(-3.66113466765132E-16,-1.,-1.12027918221652E-15));
#44352=DIRECTION('ref_axis',(-0.774362902971737,-4.25342698788503E-16,0.632741728117551));
#44353=DIRECTION('',(-3.66113466765132E-16,-1.,-1.12027918221652E-15));
#44354=DIRECTION('center_axis',(3.66113466765132E-16,1.,1.12027918221652E-15));
#44355=DIRECTION('ref_axis',(0.996376843918701,-4.60064633258624E-16,0.0850481328578616));
#44356=DIRECTION('',(3.66113466765132E-16,1.,1.12027918221652E-15));
#44357=DIRECTION('center_axis',(-3.66113466765132E-16,-1.,-1.12027918221652E-15));
#44358=DIRECTION('ref_axis',(0.996376843918701,-4.60064633258624E-16,0.0850481328578616));
#44359=DIRECTION('center_axis',(3.66113466765132E-16,1.,1.12027918221652E-15));
#44360=DIRECTION('ref_axis',(0.336889853392226,-1.17813212750748E-15,0.941544065183018));
#44361=DIRECTION('',(3.66113466765132E-16,1.,1.12027918221652E-15));
#44362=DIRECTION('center_axis',(-3.66113466765132E-16,-1.,-1.12027918221652E-15));
#44363=DIRECTION('ref_axis',(0.336889853392226,-1.17813212750748E-15,0.941544065183018));
#44364=DIRECTION('',(3.66113466765132E-16,1.,1.12027918221652E-15));
#44365=DIRECTION('center_axis',(3.66113466765132E-16,1.,1.12027918221652E-15));
#44366=DIRECTION('ref_axis',(-0.685148752559916,-5.65172729328823E-16,0.728403176040296));
#44367=DIRECTION('center_axis',(-3.66113466765132E-16,-1.,-1.12027918221652E-15));
#44368=DIRECTION('ref_axis',(-0.685148752559916,-5.65172729328823E-16,0.728403176040296));
#44369=DIRECTION('',(-3.66113466765132E-16,-1.,-1.12027918221652E-15));
#44370=DIRECTION('center_axis',(3.66113466765132E-16,1.,1.12027918221652E-15));
#44371=DIRECTION('ref_axis',(0.998953710832413,-3.14496968341737E-16,-0.0457327411615765));
#44372=DIRECTION('',(3.66113466765132E-16,1.,1.12027918221652E-15));
#44373=DIRECTION('center_axis',(-3.66113466765132E-16,-1.,-1.12027918221652E-15));
#44374=DIRECTION('ref_axis',(0.998953710832413,-3.14496968341737E-16,-0.0457327411615765));
#44375=DIRECTION('center_axis',(3.66113466765132E-16,1.,1.12027918221652E-15));
#44376=DIRECTION('ref_axis',(0.456903875630426,-1.16378500342752E-15,0.889516075421853));
#44377=DIRECTION('',(3.66113466765132E-16,1.,1.12027918221652E-15));
#44378=DIRECTION('center_axis',(-3.66113466765132E-16,-1.,-1.12027918221652E-15));
#44379=DIRECTION('ref_axis',(0.456903875630426,-1.16378500342752E-15,0.889516075421853));
#44380=DIRECTION('',(3.66113466765132E-16,1.,1.12027918221652E-15));
#44381=DIRECTION('center_axis',(3.66113466765132E-16,1.,1.12027918221652E-15));
#44382=DIRECTION('ref_axis',(-0.584211517032673,-6.95332497774842E-16,0.811601443669479));
#44383=DIRECTION('center_axis',(-3.66113466765132E-16,-1.,-1.12027918221652E-15));
#44384=DIRECTION('ref_axis',(-0.584211517032673,-6.95332497774842E-16,0.811601443669479));
#44385=DIRECTION('',(-3.66113466765132E-16,-1.,-1.12027918221652E-15));
#44386=DIRECTION('center_axis',(3.66113466765132E-16,1.,1.12027918221652E-15));
#44387=DIRECTION('ref_axis',(0.98443820279149,-1.63548173101491E-16,-0.175731115300228));
#44388=DIRECTION('',(3.66113466765132E-16,1.,1.12027918221652E-15));
#44389=DIRECTION('center_axis',(-3.66113466765132E-16,-1.,-1.12027918221652E-15));
#44390=DIRECTION('ref_axis',(0.98443820279149,-1.63548173101491E-16,-0.175731115300228));
#44391=DIRECTION('center_axis',(3.66113466765132E-16,1.,1.12027918221652E-15));
#44392=DIRECTION('ref_axis',(0.569100145878903,-1.12952519527676E-15,0.822268218989772));
#44393=DIRECTION('',(3.66113466765132E-16,1.,1.12027918221652E-15));
#44394=DIRECTION('center_axis',(-3.66113466765132E-16,-1.,-1.12027918221652E-15));
#44395=DIRECTION('ref_axis',(0.569100145878903,-1.12952519527676E-15,0.822268218989772));
#44396=DIRECTION('',(3.66113466765132E-16,1.,1.12027918221652E-15));
#44397=DIRECTION('center_axis',(3.66113466765132E-16,1.,1.12027918221652E-15));
#44398=DIRECTION('ref_axis',(-0.473278260474969,-8.13594934401345E-16,0.880912985579045));
#44399=DIRECTION('center_axis',(-3.66113466765132E-16,-1.,-1.12027918221652E-15));
#44400=DIRECTION('ref_axis',(-0.473278260474969,-8.13594934401345E-16,0.880912985579045));
#44401=DIRECTION('',(-3.66113466765132E-16,-1.,-1.12027918221652E-15));
#44402=DIRECTION('center_axis',(3.66113466765132E-16,1.,1.12027918221652E-15));
#44403=DIRECTION('ref_axis',(0.95307868416297,-9.80102327535809E-18,-0.302722681334224));
#44404=DIRECTION('',(3.66113466765132E-16,1.,1.12027918221652E-15));
#44405=DIRECTION('center_axis',(-3.66113466765132E-16,-1.,-1.12027918221652E-15));
#44406=DIRECTION('ref_axis',(0.95307868416297,-9.80102327535809E-18,-0.302722681334224));
#44407=DIRECTION('center_axis',(3.66113466765132E-16,1.,1.12027918221652E-15));
#44408=DIRECTION('ref_axis',(0.671558954847023,-1.07593889787127E-15,0.740951125354955));
#44409=DIRECTION('',(3.66113466765132E-16,1.,1.12027918221652E-15));
#44410=DIRECTION('center_axis',(-3.66113466765132E-16,-1.,-1.12027918221652E-15));
#44411=DIRECTION('ref_axis',(0.671558954847023,-1.07593889787127E-15,0.740951125354955));
#44412=DIRECTION('',(3.66113466765132E-16,1.,1.12027918221652E-15));
#44413=DIRECTION('center_axis',(3.66113466765132E-16,1.,1.12027918221652E-15));
#44414=DIRECTION('ref_axis',(-0.354247081663014,-9.17936536129109E-16,0.935151862070134));
#44415=DIRECTION('center_axis',(-3.66113466765132E-16,-1.,-1.12027918221652E-15));
#44416=DIRECTION('ref_axis',(-0.354247081663014,-9.17936536129109E-16,0.935151862070134));
#44417=DIRECTION('',(-3.66113466765132E-16,-1.,-1.12027918221652E-15));
#44418=DIRECTION('center_axis',(3.66113466765132E-16,1.,1.12027918221652E-15));
#44419=DIRECTION('ref_axis',(0.905411725005089,1.44113824776374E-16,-0.424534578360008));
#44420=DIRECTION('',(3.66113466765132E-16,1.,1.12027918221652E-15));
#44421=DIRECTION('center_axis',(-3.66113466765132E-16,-1.,-1.12027918221652E-15));
#44422=DIRECTION('ref_axis',(0.905411725005089,1.44113824776374E-16,-0.424534578360008));
#44423=DIRECTION('center_axis',(3.66113466765132E-16,1.,1.12027918221652E-15));
#44424=DIRECTION('ref_axis',(0.762527203906392,-1.00394298761658E-15,0.646956152534853));
#44425=DIRECTION('',(3.66113466765132E-16,1.,1.12027918221652E-15));
#44426=DIRECTION('center_axis',(-3.66113466765132E-16,-1.,-1.12027918221652E-15));
#44427=DIRECTION('ref_axis',(0.762527203906392,-1.00394298761658E-15,0.646956152534853));
#44428=DIRECTION('',(3.66113466765132E-16,1.,1.12027918221652E-15));
#44429=DIRECTION('center_axis',(3.66113466765132E-16,1.,1.12027918221652E-15));
#44430=DIRECTION('ref_axis',(-0.229154637067958,-1.00657198922362E-15,0.973390030928123));
#44431=DIRECTION('center_axis',(-3.66113466765132E-16,-1.,-1.12027918221652E-15));
#44432=DIRECTION('ref_axis',(-0.229154637067958,-1.00657198922362E-15,0.973390030928123));
#44433=DIRECTION('',(-3.66113466765132E-16,-1.,-1.12027918221652E-15));
#44434=DIRECTION('center_axis',(3.66113466765132E-16,1.,1.12027918221652E-15));
#44435=DIRECTION('ref_axis',(0.842252920204816,2.9556284533028E-16,-0.53908257104683));
#44436=DIRECTION('',(3.66113466765132E-16,1.,1.12027918221652E-15));
#44437=DIRECTION('center_axis',(-3.66113466765132E-16,-1.,-1.12027918221652E-15));
#44438=DIRECTION('ref_axis',(0.842252920204816,2.9556284533028E-16,-0.53908257104683));
#44439=DIRECTION('center_axis',(3.66113466765132E-16,1.,1.12027918221652E-15));
#44440=DIRECTION('ref_axis',(0.840448401094441,-9.14769334498193E-16,0.541891580574747));
#44441=DIRECTION('',(3.66113466765132E-16,1.,1.12027918221652E-15));
#44442=DIRECTION('center_axis',(-3.66113466765132E-16,-1.,-1.12027918221652E-15));
#44443=DIRECTION('ref_axis',(0.840448401094441,-9.14769334498193E-16,0.541891580574747));
#44444=DIRECTION('',(3.66113466765132E-16,1.,1.12027918221652E-15));
#44445=DIRECTION('center_axis',(3.66113466765132E-16,1.,1.12027918221652E-15));
#44446=DIRECTION('ref_axis',(-0.100141293099002,-1.07798471650803E-15,0.994973226482231));
#44447=DIRECTION('center_axis',(-3.66113466765132E-16,-1.,-1.12027918221652E-15));
#44448=DIRECTION('ref_axis',(-0.100141293099002,-1.07798471650803E-15,0.994973226482231));
#44449=DIRECTION('',(-3.66113466765132E-16,-1.,-1.12027918221652E-15));
#44450=DIRECTION('center_axis',(3.66113466765132E-16,1.,1.12027918221652E-15));
#44451=DIRECTION('ref_axis',(0.764682934423213,4.41954703655085E-16,-0.644406711481115));
#44452=DIRECTION('',(3.66113466765132E-16,1.,1.12027918221652E-15));
#44453=DIRECTION('center_axis',(-3.66113466765132E-16,-1.,-1.12027918221652E-15));
#44454=DIRECTION('ref_axis',(0.764682934423213,4.41954703655085E-16,-0.644406711481115));
#44455=DIRECTION('center_axis',(3.66113466765132E-16,1.,1.12027918221652E-15));
#44456=DIRECTION('ref_axis',(0.903989293123446,-8.09943724444564E-16,0.427555093430276));
#44457=DIRECTION('',(3.66113466765132E-16,1.,1.12027918221652E-15));
#44458=DIRECTION('center_axis',(-3.66113466765132E-16,-1.,-1.12027918221652E-15));
#44459=DIRECTION('ref_axis',(0.903989293123446,-8.09943724444564E-16,0.427555093430276));
#44460=DIRECTION('',(3.66113466765132E-16,1.,1.12027918221652E-15));
#44461=DIRECTION('center_axis',(3.66113466765132E-16,1.,1.12027918221652E-15));
#44462=DIRECTION('ref_axis',(0.0305854961592909,-1.13095282641916E-15,0.999532154272533));
#44463=DIRECTION('center_axis',(-3.66113466765132E-16,-1.,-1.12027918221652E-15));
#44464=DIRECTION('ref_axis',(0.0305854961592909,-1.13095282641916E-15,0.999532154272533));
#44465=DIRECTION('',(-3.66113466765132E-16,-1.,-1.12027918221652E-15));
#44466=DIRECTION('center_axis',(3.66113466765132E-16,1.,1.12027918221652E-15));
#44467=DIRECTION('ref_axis',(0.674029011623465,5.80784594467357E-16,-0.738704874418665));
#44468=DIRECTION('',(3.66113466765132E-16,1.,1.12027918221652E-15));
#44469=DIRECTION('center_axis',(-3.66113466765132E-16,-1.,-1.12027918221652E-15));
#44470=DIRECTION('ref_axis',(0.674029011623465,5.80784594467357E-16,-0.738704874418665));
#44471=DIRECTION('center_axis',(3.66113466765132E-16,1.,1.12027918221652E-15));
#44472=DIRECTION('ref_axis',(0.952062677713926,-6.91259752706864E-16,0.305903020096547));
#44473=DIRECTION('',(3.66113466765132E-16,1.,1.12027918221652E-15));
#44474=DIRECTION('center_axis',(-3.66113466765132E-16,-1.,-1.12027918221652E-15));
#44475=DIRECTION('ref_axis',(0.952062677713926,-6.91259752706864E-16,0.305903020096547));
#44476=DIRECTION('',(3.66113466765132E-16,1.,1.12027918221652E-15));
#44477=DIRECTION('center_axis',(3.66113466765132E-16,1.,1.12027918221652E-15));
#44478=DIRECTION('ref_axis',(0.160788959098396,-1.1645700199109E-15,0.986988809780564));
#44479=DIRECTION('center_axis',(-3.66113466765132E-16,-1.,-1.12027918221652E-15));
#44480=DIRECTION('ref_axis',(0.160788959098396,-1.1645700199109E-15,0.986988809780564));
#44481=DIRECTION('',(-3.66113466765132E-16,-1.,-1.12027918221652E-15));
#44482=DIRECTION('center_axis',(3.66113466765132E-16,1.,1.12027918221652E-15));
#44483=DIRECTION('ref_axis',(0.571842265558692,7.09677099844383E-16,-0.820363592147227));
#44484=DIRECTION('',(3.66113466765132E-16,1.,1.12027918221652E-15));
#44485=DIRECTION('center_axis',(-3.66113466765132E-16,-1.,-1.12027918221652E-15));
#44486=DIRECTION('ref_axis',(0.571842265558692,7.09677099844383E-16,-0.820363592147227));
#44487=DIRECTION('center_axis',(3.66113466765132E-16,1.,1.12027918221652E-15));
#44488=DIRECTION('ref_axis',(0.983846005927078,-5.60748134946939E-16,0.179016861276626));
#44489=DIRECTION('',(3.66113466765132E-16,1.,1.12027918221652E-15));
#44490=DIRECTION('center_axis',(-3.66113466765132E-16,-1.,-1.12027918221652E-15));
#44491=DIRECTION('ref_axis',(0.983846005927078,-5.60748134946939E-16,0.179016861276626));
#44492=DIRECTION('',(3.66113466765132E-16,1.,1.12027918221652E-15));
#44493=DIRECTION('center_axis',(3.66113466765132E-16,1.,1.12027918221652E-15));
#44494=DIRECTION('ref_axis',(0.288241278368206,-1.17826109748215E-15,0.957557813108254));
#44495=DIRECTION('center_axis',(-3.66113466765132E-16,-1.,-1.12027918221652E-15));
#44496=DIRECTION('ref_axis',(0.288241278368206,-1.17826109748215E-15,0.957557813108254));
#44497=DIRECTION('',(-3.66113466765132E-16,-1.,-1.12027918221652E-15));
#44498=DIRECTION('center_axis',(3.66113466765132E-16,1.,1.12027918221652E-15));
#44499=DIRECTION('ref_axis',(0.459871139785583,8.26426833283406E-16,-0.887985661366392));
#44500=DIRECTION('',(3.66113466765132E-16,1.,1.12027918221652E-15));
#44501=DIRECTION('center_axis',(-3.66113466765132E-16,-1.,-1.12027918221652E-15));
#44502=DIRECTION('ref_axis',(0.459871139785583,8.26426833283406E-16,-0.887985661366392));
#44503=DIRECTION('center_axis',(3.66113466765132E-16,1.,1.12027918221652E-15));
#44504=DIRECTION('ref_axis',(0.998795456205173,-4.20641961129317E-16,0.0490676743274118));
#44505=DIRECTION('',(3.66113466765132E-16,1.,1.12027918221652E-15));
#44506=DIRECTION('center_axis',(-3.66113466765132E-16,-1.,-1.12027918221652E-15));
#44507=DIRECTION('ref_axis',(0.998795456205173,-4.20641961129317E-16,0.0490676743274118));
#44508=DIRECTION('',(3.66113466765132E-16,1.,1.12027918221652E-15));
#44509=DIRECTION('center_axis',(3.66113466765132E-16,1.,1.12027918221652E-15));
#44510=DIRECTION('ref_axis',(0.410761709449557,-1.17179180099979E-15,0.91174273676848));
#44511=DIRECTION('center_axis',(-3.66113466765132E-16,-1.,-1.12027918221652E-15));
#44512=DIRECTION('ref_axis',(0.410761709449557,-1.17179180099979E-15,0.91174273676848));
#44513=DIRECTION('',(-3.66113466765132E-16,-1.,-1.12027918221652E-15));
#44514=DIRECTION('center_axis',(3.66113466765132E-16,1.,1.12027918221652E-15));
#44515=DIRECTION('ref_axis',(0.340031491310375,9.29036174476144E-16,-0.940414049723441));
#44516=DIRECTION('',(3.66113466765132E-16,1.,1.12027918221652E-15));
#44517=DIRECTION('center_axis',(-3.66113466765132E-16,-1.,-1.12027918221652E-15));
#44518=DIRECTION('ref_axis',(0.340031491310375,9.29036174476144E-16,-0.940414049723441));
#44519=DIRECTION('center_axis',(3.66113466765132E-16,1.,1.12027918221652E-15));
#44520=DIRECTION('ref_axis',(0.99665523930918,-2.73338486732788E-16,-0.0817210741336743));
#44521=DIRECTION('',(3.66113466765132E-16,1.,1.12027918221652E-15));
#44522=DIRECTION('center_axis',(-3.66113466765132E-16,-1.,-1.12027918221652E-15));
#44523=DIRECTION('ref_axis',(0.99665523930918,-2.73338486732788E-16,-0.0817210741336743));
#44524=DIRECTION('',(3.66113466765132E-16,1.,1.12027918221652E-15));
#44525=DIRECTION('center_axis',(3.66113466765132E-16,1.,1.12027918221652E-15));
#44526=DIRECTION('ref_axis',(0.526253893797564,-1.14527282192027E-15,0.850327489419754));
#44527=DIRECTION('center_axis',(-3.66113466765132E-16,-1.,-1.12027918221652E-15));
#44528=DIRECTION('ref_axis',(0.526253893797564,-1.14527282192027E-15,0.850327489419754));
#44529=DIRECTION('',(-3.66113466765132E-16,-1.,-1.12027918221652E-15));
#44530=DIRECTION('center_axis',(3.66113466765132E-16,1.,1.12027918221652E-15));
#44531=DIRECTION('ref_axis',(0.214373809744306,1.01574944914611E-15,-0.976751692957689));
#44532=DIRECTION('',(3.66113466765132E-16,1.,1.12027918221652E-15));
#44533=DIRECTION('center_axis',(-3.66113466765132E-16,-1.,-1.12027918221652E-15));
#44534=DIRECTION('ref_axis',(0.214373809744306,1.01574944914611E-15,-0.976751692957689));
#44535=DIRECTION('center_axis',(3.66113466765132E-16,1.,1.12027918221652E-15));
#44536=DIRECTION('ref_axis',(0.977461974943571,-1.21358115044515E-16,-0.211111552358971));
#44537=DIRECTION('',(3.66113466765132E-16,1.,1.12027918221652E-15));
#44538=DIRECTION('center_axis',(-3.66113466765132E-16,-1.,-1.12027918221652E-15));
#44539=DIRECTION('ref_axis',(0.977461974943571,-1.21358115044515E-16,-0.211111552358971));
#44540=DIRECTION('',(3.66113466765132E-16,1.,1.12027918221652E-15));
#44541=DIRECTION('center_axis',(3.66113466765132E-16,1.,1.12027918221652E-15));
#44542=DIRECTION('ref_axis',(0.63274172811755,-1.09915790732807E-15,0.774362902971737));
#44543=DIRECTION('center_axis',(-3.66113466765132E-16,-1.,-1.12027918221652E-15));
#44544=DIRECTION('ref_axis',(0.63274172811755,-1.09915790732807E-15,0.774362902971737));
#44545=DIRECTION('',(-3.66113466765132E-16,-1.,-1.12027918221652E-15));
#44546=DIRECTION('center_axis',(3.66113466765132E-16,1.,1.12027918221652E-15));
#44547=DIRECTION('ref_axis',(0.0850481328578621,1.08508296912223E-15,-0.996376843918701));
#44548=DIRECTION('',(3.66113466765132E-16,1.,1.12027918221652E-15));
#44549=DIRECTION('center_axis',(-3.66113466765132E-16,-1.,-1.12027918221652E-15));
#44550=DIRECTION('ref_axis',(0.0850481328578621,1.08508296912223E-15,-0.996376843918701));
#44551=DIRECTION('center_axis',(3.66113466765132E-16,1.,1.12027918221652E-15));
#44552=DIRECTION('ref_axis',(0.941544065183019,3.2698727638996E-17,-0.336889853392226));
#44553=DIRECTION('',(3.66113466765132E-16,1.,1.12027918221652E-15));
#44554=DIRECTION('center_axis',(-3.66113466765132E-16,-1.,-1.12027918221652E-15));
#44555=DIRECTION('ref_axis',(0.941544065183019,3.2698727638996E-17,-0.336889853392226));
#44556=DIRECTION('',(3.66113466765132E-16,1.,1.12027918221652E-15));
#44557=DIRECTION('center_axis',(3.66113466765132E-16,1.,1.12027918221652E-15));
#44558=DIRECTION('ref_axis',(0.728403176040296,-1.03423609619734E-15,0.685148752559917));
#44559=DIRECTION('center_axis',(-3.66113466765132E-16,-1.,-1.12027918221652E-15));
#44560=DIRECTION('ref_axis',(0.728403176040296,-1.03423609619734E-15,0.685148752559917));
#44561=DIRECTION('',(-3.66113466765132E-16,-1.,-1.12027918221652E-15));
#44562=DIRECTION('center_axis',(3.66113466765132E-16,1.,1.12027918221652E-15));
#44563=DIRECTION('ref_axis',(-0.0457327411615761,1.13585041865483E-15,-0.998953710832413));
#44564=DIRECTION('',(3.66113466765132E-16,1.,1.12027918221652E-15));
#44565=DIRECTION('center_axis',(-3.66113466765132E-16,-1.,-1.12027918221652E-15));
#44566=DIRECTION('ref_axis',(-0.0457327411615761,1.13585041865483E-15,-0.998953710832413));
#44567=DIRECTION('center_axis',(3.66113466765132E-16,1.,1.12027918221652E-15));
#44568=DIRECTION('ref_axis',(0.889516075421853,1.86196086026803E-16,-0.456903875630426));
#44569=DIRECTION('',(3.66113466765132E-16,1.,1.12027918221652E-15));
#44570=DIRECTION('center_axis',(-3.66113466765132E-16,-1.,-1.12027918221652E-15));
#44571=DIRECTION('ref_axis',(0.889516075421853,1.86196086026803E-16,-0.456903875630426));
#44572=DIRECTION('',(3.66113466765132E-16,1.,1.12027918221652E-15));
#44573=DIRECTION('center_axis',(3.66113466765132E-16,1.,1.12027918221652E-15));
#44574=DIRECTION('ref_axis',(0.811601443669479,-9.51618218716256E-16,0.584211517032674));
#44575=DIRECTION('center_axis',(-3.66113466765132E-16,-1.,-1.12027918221652E-15));
#44576=DIRECTION('ref_axis',(0.811601443669479,-9.51618218716256E-16,0.584211517032674));
#44577=DIRECTION('',(-3.66113466765132E-16,-1.,-1.12027918221652E-15));
#44578=DIRECTION('center_axis',(3.66113466765132E-16,1.,1.12027918221652E-15));
#44579=DIRECTION('ref_axis',(-0.175731115300228,1.16718315260702E-15,-0.98443820279149));
#44580=DIRECTION('',(3.66113466765132E-16,1.,1.12027918221652E-15));
#44581=DIRECTION('center_axis',(-3.66113466765132E-16,-1.,-1.12027918221652E-15));
#44582=DIRECTION('ref_axis',(-0.175731115300228,1.16718315260702E-15,-0.98443820279149));
#44583=DIRECTION('center_axis',(3.66113466765132E-16,1.,1.12027918221652E-15));
#44584=DIRECTION('ref_axis',(0.822268218989772,3.36507577759385E-16,-0.569100145878903));
#44585=DIRECTION('',(3.66113466765132E-16,1.,1.12027918221652E-15));
#44586=DIRECTION('center_axis',(-3.66113466765132E-16,-1.,-1.12027918221652E-15));
#44587=DIRECTION('ref_axis',(0.822268218989772,3.36507577759385E-16,-0.569100145878903));
#44588=DIRECTION('',(3.66113466765132E-16,1.,1.12027918221652E-15));
#44589=DIRECTION('center_axis',(3.66113466765132E-16,1.,1.12027918221652E-15));
#44590=DIRECTION('ref_axis',(0.880912985579045,-8.52717889674523E-16,0.473278260474969));
#44591=DIRECTION('center_axis',(-3.66113466765132E-16,-1.,-1.12027918221652E-15));
#44592=DIRECTION('ref_axis',(0.880912985579045,-8.52717889674523E-16,0.473278260474969));
#44593=DIRECTION('',(-3.66113466765132E-16,-1.,-1.12027918221652E-15));
#44594=DIRECTION('center_axis',(3.66113466765132E-16,1.,1.12027918221652E-15));
#44595=DIRECTION('ref_axis',(-0.302722681334224,1.1785450592138E-15,-0.95307868416297));
#44596=DIRECTION('',(3.66113466765132E-16,1.,1.12027918221652E-15));
#44597=DIRECTION('center_axis',(-3.66113466765132E-16,-1.,-1.12027918221652E-15));
#44598=DIRECTION('ref_axis',(-0.302722681334224,1.1785450592138E-15,-0.95307868416297));
#44599=DIRECTION('center_axis',(3.66113466765132E-16,1.,1.12027918221652E-15));
#44600=DIRECTION('ref_axis',(0.740951125354955,4.81061331538975E-16,-0.671558954847023));
#44601=DIRECTION('',(3.66113466765132E-16,1.,1.12027918221652E-15));
#44602=DIRECTION('center_axis',(-3.66113466765132E-16,-1.,-1.12027918221652E-15));
#44603=DIRECTION('ref_axis',(0.740951125354955,4.81061331538975E-16,-0.671558954847023));
#44604=DIRECTION('',(3.66113466765132E-16,1.,1.12027918221652E-15));
#44605=DIRECTION('center_axis',(3.66113466765132E-16,1.,1.12027918221652E-15));
#44606=DIRECTION('ref_axis',(0.935151862070134,-7.39227321122395E-16,0.354247081663014));
#44607=DIRECTION('center_axis',(-3.66113466765132E-16,-1.,-1.12027918221652E-15));
#44608=DIRECTION('ref_axis',(0.935151862070134,-7.39227321122395E-16,0.354247081663014));
#44609=DIRECTION('',(-3.66113466765132E-16,-1.,-1.12027918221652E-15));
#44610=DIRECTION('center_axis',(3.66113466765132E-16,1.,1.12027918221652E-15));
#44611=DIRECTION('ref_axis',(-0.424534578360008,1.16974173310301E-15,-0.905411725005089));
#44612=DIRECTION('',(3.66113466765132E-16,1.,1.12027918221652E-15));
#44613=DIRECTION('center_axis',(-3.66113466765132E-16,-1.,-1.12027918221652E-15));
#44614=DIRECTION('ref_axis',(-0.424534578360008,1.16974173310301E-15,-0.905411725005089));
#44615=DIRECTION('center_axis',(3.66113466765132E-16,1.,1.12027918221652E-15));
#44616=DIRECTION('ref_axis',(0.646956152534853,6.17383992560536E-16,-0.762527203906392));
#44617=DIRECTION('',(3.66113466765132E-16,1.,1.12027918221652E-15));
#44618=DIRECTION('center_axis',(-3.66113466765132E-16,-1.,-1.12027918221652E-15));
#44619=DIRECTION('ref_axis',(0.646956152534853,6.17383992560536E-16,-0.762527203906392));
#44620=DIRECTION('',(3.66113466765132E-16,1.,1.12027918221652E-15));
#44621=DIRECTION('center_axis',(3.66113466765132E-16,1.,1.12027918221652E-15));
#44622=DIRECTION('ref_axis',(0.973390030928123,-6.13088368153331E-16,0.229154637067959));
#44623=DIRECTION('center_axis',(-3.66113466765132E-16,-1.,-1.12027918221652E-15));
#44624=DIRECTION('ref_axis',(0.973390030928123,-6.13088368153331E-16,0.229154637067959));
#44625=DIRECTION('',(-3.66113466765132E-16,-1.,-1.12027918221652E-15));
#44626=DIRECTION('center_axis',(3.66113466765132E-16,1.,1.12027918221652E-15));
#44627=DIRECTION('ref_axis',(-0.53908257104683,1.14092380162514E-15,-0.842252920204816));
#44628=DIRECTION('',(3.66113466765132E-16,1.,1.12027918221652E-15));
#44629=DIRECTION('center_axis',(-3.66113466765132E-16,-1.,-1.12027918221652E-15));
#44630=DIRECTION('ref_axis',(-0.53908257104683,1.14092380162514E-15,-0.842252920204816));
#44631=DIRECTION('center_axis',(3.66113466765132E-16,1.,1.12027918221652E-15));
#44632=DIRECTION('ref_axis',(0.541891580574746,7.43143042298206E-16,-0.840448401094442));
#44633=DIRECTION('',(3.66113466765132E-16,1.,1.12027918221652E-15));
#44634=DIRECTION('center_axis',(-3.66113466765132E-16,-1.,-1.12027918221652E-15));
#44635=DIRECTION('ref_axis',(0.541891580574746,7.43143042298206E-16,-0.840448401094442));
#44636=DIRECTION('',(3.66113466765132E-16,1.,1.12027918221652E-15));
#44637=DIRECTION('center_axis',(3.66113466765132E-16,1.,1.12027918221652E-15));
#44638=DIRECTION('ref_axis',(0.994973226482231,-4.76459303224953E-16,0.100141293099002));
#44639=DIRECTION('center_axis',(-3.66113466765132E-16,-1.,-1.12027918221652E-15));
#44640=DIRECTION('ref_axis',(0.994973226482231,-4.76459303224953E-16,0.100141293099002));
#44641=DIRECTION('',(-3.66113466765132E-16,-1.,-1.12027918221652E-15));
#44642=DIRECTION('center_axis',(3.66113466765132E-16,1.,1.12027918221652E-15));
#44643=DIRECTION('ref_axis',(-0.644406711481115,1.09258434757764E-15,-0.764682934423213));
#44644=DIRECTION('',(3.66113466765132E-16,1.,1.12027918221652E-15));
#44645=DIRECTION('center_axis',(-3.66113466765132E-16,-1.,-1.12027918221652E-15));
#44646=DIRECTION('ref_axis',(-0.644406711481115,1.09258434757764E-15,-0.764682934423213));
#44647=DIRECTION('center_axis',(3.66113466765132E-16,1.,1.12027918221652E-15));
#44648=DIRECTION('ref_axis',(0.427555093430276,8.56186708543976E-16,-0.903989293123446));
#44649=DIRECTION('',(3.66113466765132E-16,1.,1.12027918221652E-15));
#44650=DIRECTION('center_axis',(-3.66113466765132E-16,-1.,-1.12027918221652E-15));
#44651=DIRECTION('ref_axis',(0.427555093430276,8.56186708543976E-16,-0.903989293123446));
#44652=DIRECTION('',(3.66113466765132E-16,1.,1.12027918221652E-15));
#44653=DIRECTION('center_axis',(3.66113466765132E-16,1.,1.12027918221652E-15));
#44654=DIRECTION('ref_axis',(0.999532154272533,-3.31677887518921E-16,-0.0305854961592909));
#44655=DIRECTION('center_axis',(-3.66113466765132E-16,-1.,-1.12027918221652E-15));
#44656=DIRECTION('ref_axis',(0.999532154272533,-3.31677887518921E-16,-0.0305854961592909));
#44657=DIRECTION('',(-3.66113466765132E-16,-1.,-1.12027918221652E-15));
#44658=DIRECTION('center_axis',(3.66113466765132E-16,1.,1.12027918221652E-15));
#44659=DIRECTION('ref_axis',(-0.738704874418665,1.02555047242146E-15,-0.674029011623465));
#44660=DIRECTION('',(3.66113466765132E-16,1.,1.12027918221652E-15));
#44661=DIRECTION('center_axis',(-3.66113466765132E-16,-1.,-1.12027918221652E-15));
#44662=DIRECTION('ref_axis',(-0.738704874418665,1.02555047242146E-15,-0.674029011623465));
#44663=DIRECTION('center_axis',(3.66113466765132E-16,1.,1.12027918221652E-15));
#44664=DIRECTION('ref_axis',(0.305903020096548,9.54580782826757E-16,-0.952062677713926));
#44665=DIRECTION('',(3.66113466765132E-16,1.,1.12027918221652E-15));
#44666=DIRECTION('center_axis',(-3.66113466765132E-16,-1.,-1.12027918221652E-15));
#44667=DIRECTION('ref_axis',(0.305903020096548,9.54580782826757E-16,-0.952062677713926));
#44668=DIRECTION('',(3.66113466765132E-16,1.,1.12027918221652E-15));
#44669=DIRECTION('center_axis',(3.66113466765132E-16,1.,1.12027918221652E-15));
#44670=DIRECTION('ref_axis',(0.986988809780564,-1.81221371198957E-16,-0.160788959098396));
#44671=DIRECTION('center_axis',(-3.66113466765132E-16,-1.,-1.12027918221652E-15));
#44672=DIRECTION('ref_axis',(0.986988809780564,-1.81221371198957E-16,-0.160788959098396));
#44673=DIRECTION('',(-3.66113466765132E-16,-1.,-1.12027918221652E-15));
#44674=DIRECTION('center_axis',(3.66113466765132E-16,1.,1.12027918221652E-15));
#44675=DIRECTION('ref_axis',(-0.820363592147226,9.40969144345854E-16,-0.571842265558694));
#44676=DIRECTION('',(3.66113466765132E-16,1.,1.12027918221652E-15));
#44677=DIRECTION('center_axis',(-3.66113466765132E-16,-1.,-1.12027918221652E-15));
#44678=DIRECTION('ref_axis',(-0.820363592147226,9.40969144345854E-16,-0.571842265558694));
#44679=DIRECTION('center_axis',(3.66113466765132E-16,1.,1.12027918221652E-15));
#44680=DIRECTION('ref_axis',(0.179016861276627,1.03664171525558E-15,-0.983846005927078));
#44681=DIRECTION('',(3.66113466765132E-16,1.,1.12027918221652E-15));
#44682=DIRECTION('center_axis',(-3.66113466765132E-16,-1.,-1.12027918221652E-15));
#44683=DIRECTION('ref_axis',(0.179016861276627,1.03664171525558E-15,-0.983846005927078));
#44684=DIRECTION('',(3.66113466765132E-16,1.,1.12027918221652E-15));
#44685=DIRECTION('center_axis',(3.66113466765132E-16,1.,1.12027918221652E-15));
#44686=DIRECTION('ref_axis',(0.957557813108254,-2.76641069737229E-17,-0.288241278368206));
#44687=DIRECTION('center_axis',(-3.66113466765132E-16,-1.,-1.12027918221652E-15));
#44688=DIRECTION('ref_axis',(0.957557813108254,-2.76641069737229E-17,-0.288241278368206));
#44689=DIRECTION('',(-3.66113466765132E-16,-1.,-1.12027918221652E-15));
#44690=DIRECTION('center_axis',(3.66113466765132E-16,1.,1.12027918221652E-15));
#44691=DIRECTION('ref_axis',(-0.887985661366392,8.40287573324551E-16,-0.459871139785583));
#44692=DIRECTION('',(3.66113466765132E-16,1.,1.12027918221652E-15));
#44693=DIRECTION('center_axis',(-3.66113466765132E-16,-1.,-1.12027918221652E-15));
#44694=DIRECTION('ref_axis',(-0.887985661366392,8.40287573324551E-16,-0.459871139785583));
#44695=DIRECTION('center_axis',(3.66113466765132E-16,1.,1.12027918221652E-15));
#44696=DIRECTION('ref_axis',(0.0490676743274116,1.100965420525E-15,-0.998795456205173));
#44697=DIRECTION('',(3.66113466765132E-16,1.,1.12027918221652E-15));
#44698=DIRECTION('center_axis',(-3.66113466765132E-16,-1.,-1.12027918221652E-15));
#44699=DIRECTION('ref_axis',(0.0490676743274116,1.100965420525E-15,-0.998795456205173));
#44700=DIRECTION('',(3.66113466765132E-16,1.,1.12027918221652E-15));
#44701=DIRECTION('center_axis',(3.66113466765132E-16,1.,1.12027918221652E-15));
#44702=DIRECTION('ref_axis',(0.91174273676848,1.26366497791772E-16,-0.410761709449557));
#44703=DIRECTION('center_axis',(-3.66113466765132E-16,-1.,-1.12027918221652E-15));
#44704=DIRECTION('ref_axis',(0.91174273676848,1.26366497791772E-16,-0.410761709449557));
#44705=DIRECTION('',(-3.66113466765132E-16,-1.,-1.12027918221652E-15));
#44706=DIRECTION('center_axis',(3.66113466765132E-16,1.,1.12027918221652E-15));
#44707=DIRECTION('ref_axis',(-0.940414049723441,7.25228448951937E-16,-0.340031491310375));
#44708=DIRECTION('',(3.66113466765132E-16,1.,1.12027918221652E-15));
#44709=DIRECTION('center_axis',(-3.66113466765132E-16,-1.,-1.12027918221652E-15));
#44710=DIRECTION('ref_axis',(-0.940414049723441,7.25228448951937E-16,-0.340031491310375));
#44711=DIRECTION('center_axis',(3.66113466765132E-16,1.,1.12027918221652E-15));
#44712=DIRECTION('ref_axis',(-0.081721074133674,1.14645130220395E-15,-0.99665523930918));
#44713=DIRECTION('',(3.66113466765132E-16,1.,1.12027918221652E-15));
#44714=DIRECTION('center_axis',(-3.66113466765132E-16,-1.,-1.12027918221652E-15));
#44715=DIRECTION('ref_axis',(-0.081721074133674,1.14645130220395E-15,-0.99665523930918));
#44716=DIRECTION('',(3.66113466765132E-16,1.,1.12027918221652E-15));
#44717=DIRECTION('center_axis',(3.66113466765132E-16,1.,1.12027918221652E-15));
#44718=DIRECTION('ref_axis',(0.850327489419755,2.78234936744635E-16,-0.526253893797563));
#44719=DIRECTION('center_axis',(-3.66113466765132E-16,-1.,-1.12027918221652E-15));
#44720=DIRECTION('ref_axis',(0.850327489419755,2.78234936744635E-16,-0.526253893797563));
#44721=DIRECTION('',(-3.66113466765132E-16,-1.,-1.12027918221652E-15));
#44722=DIRECTION('center_axis',(3.66113466765132E-16,1.,1.12027918221652E-15));
#44723=DIRECTION('ref_axis',(-0.976751692957689,5.97760464746442E-16,-0.214373809744306));
#44724=DIRECTION('',(3.66113466765132E-16,1.,1.12027918221652E-15));
#44725=DIRECTION('center_axis',(-3.66113466765132E-16,-1.,-1.12027918221652E-15));
#44726=DIRECTION('ref_axis',(-0.976751692957689,5.97760464746442E-16,-0.214373809744306));
#44727=DIRECTION('center_axis',(3.66113466765132E-16,1.,1.12027918221652E-15));
#44728=DIRECTION('ref_axis',(-0.211111552358971,1.17232108424584E-15,-0.977461974943571));
#44729=DIRECTION('',(3.66113466765132E-16,1.,1.12027918221652E-15));
#44730=DIRECTION('center_axis',(-3.66113466765132E-16,-1.,-1.12027918221652E-15));
#44731=DIRECTION('ref_axis',(-0.211111552358971,1.17232108424584E-15,-0.977461974943571));
#44732=DIRECTION('',(3.66113466765132E-16,1.,1.12027918221652E-15));
#44733=DIRECTION('center_axis',(3.66113466765132E-16,1.,1.12027918221652E-15));
#44734=DIRECTION('ref_axis',(0.774362902971737,4.25342698788503E-16,-0.63274172811755));
#44735=DIRECTION('center_axis',(-3.66113466765132E-16,-1.,-1.12027918221652E-15));
#44736=DIRECTION('ref_axis',(0.774362902971737,4.25342698788503E-16,-0.63274172811755));
#44737=DIRECTION('',(-3.66113466765132E-16,-1.,-1.12027918221652E-15));
#44738=DIRECTION('center_axis',(3.66113466765132E-16,1.,1.12027918221652E-15));
#44739=DIRECTION('ref_axis',(-0.996376843918701,4.60064633258625E-16,-0.0850481328578625));
#44740=DIRECTION('',(3.66113466765132E-16,1.,1.12027918221652E-15));
#44741=DIRECTION('center_axis',(-3.66113466765132E-16,-1.,-1.12027918221652E-15));
#44742=DIRECTION('ref_axis',(-0.996376843918701,4.60064633258625E-16,-0.0850481328578625));
#44743=DIRECTION('center_axis',(3.66113466765132E-16,1.,1.12027918221652E-15));
#44744=DIRECTION('ref_axis',(-0.336889853392226,1.17813212750748E-15,-0.941544065183019));
#44745=DIRECTION('',(3.66113466765132E-16,1.,1.12027918221652E-15));
#44746=DIRECTION('center_axis',(-3.66113466765132E-16,-1.,-1.12027918221652E-15));
#44747=DIRECTION('ref_axis',(-0.336889853392226,1.17813212750748E-15,-0.941544065183019));
#44748=DIRECTION('',(3.66113466765132E-16,1.,1.12027918221652E-15));
#44749=DIRECTION('center_axis',(3.66113466765132E-16,1.,1.12027918221652E-15));
#44750=DIRECTION('ref_axis',(0.685148752559917,5.65172729328822E-16,-0.728403176040296));
#44751=DIRECTION('center_axis',(-3.66113466765132E-16,-1.,-1.12027918221652E-15));
#44752=DIRECTION('ref_axis',(0.685148752559917,5.65172729328822E-16,-0.728403176040296));
#44753=DIRECTION('',(-3.66113466765132E-16,-1.,-1.12027918221652E-15));
#44754=DIRECTION('center_axis',(3.66113466765132E-16,1.,1.12027918221652E-15));
#44755=DIRECTION('ref_axis',(-0.998953710832413,3.14496968341738E-16,0.045732741161576));
#44756=DIRECTION('',(3.66113466765132E-16,1.,1.12027918221652E-15));
#44757=DIRECTION('center_axis',(-3.66113466765132E-16,-1.,-1.12027918221652E-15));
#44758=DIRECTION('ref_axis',(-0.998953710832413,3.14496968341738E-16,0.045732741161576));
#44759=DIRECTION('center_axis',(3.66113466765132E-16,1.,1.12027918221652E-15));
#44760=DIRECTION('ref_axis',(-0.456903875630426,1.16378500342752E-15,-0.889516075421853));
#44761=DIRECTION('',(3.66113466765132E-16,1.,1.12027918221652E-15));
#44762=DIRECTION('center_axis',(-3.66113466765132E-16,-1.,-1.12027918221652E-15));
#44763=DIRECTION('ref_axis',(-0.456903875630426,1.16378500342752E-15,-0.889516075421853));
#44764=DIRECTION('',(3.66113466765132E-16,1.,1.12027918221652E-15));
#44765=DIRECTION('center_axis',(3.66113466765132E-16,1.,1.12027918221652E-15));
#44766=DIRECTION('ref_axis',(0.584211517032674,6.95332497774842E-16,-0.811601443669479));
#44767=DIRECTION('center_axis',(-3.66113466765132E-16,-1.,-1.12027918221652E-15));
#44768=DIRECTION('ref_axis',(0.584211517032674,6.95332497774842E-16,-0.811601443669479));
#44769=DIRECTION('',(-3.66113466765132E-16,-1.,-1.12027918221652E-15));
#44770=DIRECTION('center_axis',(3.66113466765132E-16,1.,1.12027918221652E-15));
#44771=DIRECTION('ref_axis',(-0.98443820279149,1.63548173101491E-16,0.175731115300228));
#44772=DIRECTION('',(3.66113466765132E-16,1.,1.12027918221652E-15));
#44773=DIRECTION('center_axis',(-3.66113466765132E-16,-1.,-1.12027918221652E-15));
#44774=DIRECTION('ref_axis',(-0.98443820279149,1.63548173101491E-16,0.175731115300228));
#44775=DIRECTION('center_axis',(3.66113466765132E-16,1.,1.12027918221652E-15));
#44776=DIRECTION('ref_axis',(-0.569100145878903,1.12952519527676E-15,-0.822268218989772));
#44777=DIRECTION('',(3.66113466765132E-16,1.,1.12027918221652E-15));
#44778=DIRECTION('center_axis',(-3.66113466765132E-16,-1.,-1.12027918221652E-15));
#44779=DIRECTION('ref_axis',(-0.569100145878903,1.12952519527676E-15,-0.822268218989772));
#44780=DIRECTION('',(3.66113466765132E-16,1.,1.12027918221652E-15));
#44781=DIRECTION('center_axis',(3.66113466765132E-16,1.,1.12027918221652E-15));
#44782=DIRECTION('ref_axis',(0.473278260474969,8.13594934401345E-16,-0.880912985579045));
#44783=DIRECTION('center_axis',(-3.66113466765132E-16,-1.,-1.12027918221652E-15));
#44784=DIRECTION('ref_axis',(0.473278260474969,8.13594934401345E-16,-0.880912985579045));
#44785=DIRECTION('',(-3.66113466765132E-16,-1.,-1.12027918221652E-15));
#44786=DIRECTION('center_axis',(3.66113466765132E-16,1.,1.12027918221652E-15));
#44787=DIRECTION('ref_axis',(-0.95307868416297,9.80102327535809E-18,0.302722681334224));
#44788=DIRECTION('',(3.66113466765132E-16,1.,1.12027918221652E-15));
#44789=DIRECTION('center_axis',(-3.66113466765132E-16,-1.,-1.12027918221652E-15));
#44790=DIRECTION('ref_axis',(-0.95307868416297,9.80102327535809E-18,0.302722681334224));
#44791=DIRECTION('center_axis',(3.66113466765132E-16,1.,1.12027918221652E-15));
#44792=DIRECTION('ref_axis',(-0.671558954847023,1.07593889787127E-15,-0.740951125354955));
#44793=DIRECTION('',(3.66113466765132E-16,1.,1.12027918221652E-15));
#44794=DIRECTION('center_axis',(-3.66113466765132E-16,-1.,-1.12027918221652E-15));
#44795=DIRECTION('ref_axis',(-0.671558954847023,1.07593889787127E-15,-0.740951125354955));
#44796=DIRECTION('',(3.66113466765132E-16,1.,1.12027918221652E-15));
#44797=DIRECTION('center_axis',(3.66113466765132E-16,1.,1.12027918221652E-15));
#44798=DIRECTION('ref_axis',(0.354247081663014,9.17936536129109E-16,-0.935151862070134));
#44799=DIRECTION('center_axis',(-3.66113466765132E-16,-1.,-1.12027918221652E-15));
#44800=DIRECTION('ref_axis',(0.354247081663014,9.17936536129109E-16,-0.935151862070134));
#44801=DIRECTION('',(-3.66113466765132E-16,-1.,-1.12027918221652E-15));
#44802=DIRECTION('center_axis',(3.66113466765132E-16,1.,1.12027918221652E-15));
#44803=DIRECTION('ref_axis',(-0.905411725005089,-1.44113824776374E-16,0.424534578360008));
#44804=DIRECTION('',(3.66113466765132E-16,1.,1.12027918221652E-15));
#44805=DIRECTION('center_axis',(-3.66113466765132E-16,-1.,-1.12027918221652E-15));
#44806=DIRECTION('ref_axis',(-0.905411725005089,-1.44113824776374E-16,0.424534578360008));
#44807=DIRECTION('center_axis',(3.66113466765132E-16,1.,1.12027918221652E-15));
#44808=DIRECTION('ref_axis',(-0.762527203906392,1.00394298761658E-15,-0.646956152534853));
#44809=DIRECTION('',(3.66113466765132E-16,1.,1.12027918221652E-15));
#44810=DIRECTION('center_axis',(-3.66113466765132E-16,-1.,-1.12027918221652E-15));
#44811=DIRECTION('ref_axis',(-0.762527203906392,1.00394298761658E-15,-0.646956152534853));
#44812=DIRECTION('',(3.66113466765132E-16,1.,1.12027918221652E-15));
#44813=DIRECTION('center_axis',(3.66113466765132E-16,1.,1.12027918221652E-15));
#44814=DIRECTION('ref_axis',(0.229154637067959,1.00657198922362E-15,-0.973390030928123));
#44815=DIRECTION('center_axis',(-3.66113466765132E-16,-1.,-1.12027918221652E-15));
#44816=DIRECTION('ref_axis',(0.229154637067959,1.00657198922362E-15,-0.973390030928123));
#44817=DIRECTION('',(-3.66113466765132E-16,-1.,-1.12027918221652E-15));
#44818=DIRECTION('center_axis',(3.66113466765132E-16,1.,1.12027918221652E-15));
#44819=DIRECTION('ref_axis',(-0.842252920204816,-2.9556284533028E-16,0.53908257104683));
#44820=DIRECTION('',(3.66113466765132E-16,1.,1.12027918221652E-15));
#44821=DIRECTION('center_axis',(-3.66113466765132E-16,-1.,-1.12027918221652E-15));
#44822=DIRECTION('ref_axis',(-0.842252920204816,-2.9556284533028E-16,0.53908257104683));
#44823=DIRECTION('center_axis',(3.66113466765132E-16,1.,1.12027918221652E-15));
#44824=DIRECTION('ref_axis',(-0.840448401094441,9.14769334498193E-16,-0.541891580574747));
#44825=DIRECTION('',(3.66113466765132E-16,1.,1.12027918221652E-15));
#44826=DIRECTION('center_axis',(-3.66113466765132E-16,-1.,-1.12027918221652E-15));
#44827=DIRECTION('ref_axis',(-0.840448401094441,9.14769334498193E-16,-0.541891580574747));
#44828=DIRECTION('',(3.66113466765132E-16,1.,1.12027918221652E-15));
#44829=DIRECTION('center_axis',(3.66113466765132E-16,1.,1.12027918221652E-15));
#44830=DIRECTION('ref_axis',(0.100141293099002,1.07798471650803E-15,-0.994973226482231));
#44831=DIRECTION('center_axis',(-3.66113466765132E-16,-1.,-1.12027918221652E-15));
#44832=DIRECTION('ref_axis',(0.100141293099002,1.07798471650803E-15,-0.994973226482231));
#44833=DIRECTION('',(-3.66113466765132E-16,-1.,-1.12027918221652E-15));
#44834=DIRECTION('center_axis',(3.66113466765132E-16,1.,1.12027918221652E-15));
#44835=DIRECTION('ref_axis',(-0.764682934423213,-4.41954703655085E-16,0.644406711481115));
#44836=DIRECTION('',(3.66113466765132E-16,1.,1.12027918221652E-15));
#44837=DIRECTION('center_axis',(-3.66113466765132E-16,-1.,-1.12027918221652E-15));
#44838=DIRECTION('ref_axis',(-0.764682934423213,-4.41954703655085E-16,0.644406711481115));
#44839=DIRECTION('center_axis',(3.66113466765132E-16,1.,1.12027918221652E-15));
#44840=DIRECTION('ref_axis',(-0.903989293123446,8.09943724444565E-16,-0.427555093430277));
#44841=DIRECTION('',(3.66113466765132E-16,1.,1.12027918221652E-15));
#44842=DIRECTION('center_axis',(-3.66113466765132E-16,-1.,-1.12027918221652E-15));
#44843=DIRECTION('ref_axis',(-0.903989293123446,8.09943724444565E-16,-0.427555093430277));
#44844=DIRECTION('',(3.66113466765132E-16,1.,1.12027918221652E-15));
#44845=DIRECTION('center_axis',(3.66113466765132E-16,1.,1.12027918221652E-15));
#44846=DIRECTION('ref_axis',(-0.0305854961592907,1.13095282641916E-15,-0.999532154272533));
#44847=DIRECTION('center_axis',(-3.66113466765132E-16,-1.,-1.12027918221652E-15));
#44848=DIRECTION('ref_axis',(-0.0305854961592907,1.13095282641916E-15,-0.999532154272533));
#44849=DIRECTION('',(-3.66113466765132E-16,-1.,-1.12027918221652E-15));
#44850=DIRECTION('center_axis',(3.66113466765132E-16,1.,1.12027918221652E-15));
#44851=DIRECTION('ref_axis',(-0.674029011623465,-5.80784594467357E-16,0.738704874418665));
#44852=DIRECTION('',(3.66113466765132E-16,1.,1.12027918221652E-15));
#44853=DIRECTION('center_axis',(-3.66113466765132E-16,-1.,-1.12027918221652E-15));
#44854=DIRECTION('ref_axis',(-0.674029011623465,-5.80784594467357E-16,0.738704874418665));
#44855=DIRECTION('center_axis',(3.66113466765132E-16,1.,1.12027918221652E-15));
#44856=DIRECTION('ref_axis',(-0.952062677713926,6.91259752706865E-16,-0.305903020096548));
#44857=DIRECTION('',(3.66113466765132E-16,1.,1.12027918221652E-15));
#44858=DIRECTION('center_axis',(-3.66113466765132E-16,-1.,-1.12027918221652E-15));
#44859=DIRECTION('ref_axis',(-0.952062677713926,6.91259752706865E-16,-0.305903020096548));
#44860=DIRECTION('',(3.66113466765132E-16,1.,1.12027918221652E-15));
#44861=DIRECTION('center_axis',(3.66113466765132E-16,1.,1.12027918221652E-15));
#44862=DIRECTION('ref_axis',(-0.160788959098396,1.1645700199109E-15,-0.986988809780564));
#44863=DIRECTION('center_axis',(-3.66113466765132E-16,-1.,-1.12027918221652E-15));
#44864=DIRECTION('ref_axis',(-0.160788959098396,1.1645700199109E-15,-0.986988809780564));
#44865=DIRECTION('',(-3.66113466765132E-16,-1.,-1.12027918221652E-15));
#44866=DIRECTION('center_axis',(3.66113466765132E-16,1.,1.12027918221652E-15));
#44867=DIRECTION('ref_axis',(-0.571842265558694,-7.09677099844381E-16,0.820363592147226));
#44868=DIRECTION('',(3.66113466765132E-16,1.,1.12027918221652E-15));
#44869=DIRECTION('center_axis',(-3.66113466765132E-16,-1.,-1.12027918221652E-15));
#44870=DIRECTION('ref_axis',(-0.571842265558694,-7.09677099844381E-16,0.820363592147226));
#44871=DIRECTION('center_axis',(3.66113466765132E-16,1.,1.12027918221652E-15));
#44872=DIRECTION('ref_axis',(-0.983846005927078,5.60748134946939E-16,-0.179016861276627));
#44873=DIRECTION('',(3.66113466765132E-16,1.,1.12027918221652E-15));
#44874=DIRECTION('center_axis',(-3.66113466765132E-16,-1.,-1.12027918221652E-15));
#44875=DIRECTION('ref_axis',(-0.983846005927078,5.60748134946939E-16,-0.179016861276627));
#44876=DIRECTION('',(3.66113466765132E-16,1.,1.12027918221652E-15));
#44877=DIRECTION('center_axis',(3.66113466765132E-16,1.,1.12027918221652E-15));
#44878=DIRECTION('ref_axis',(-0.288241278368206,1.17826109748215E-15,-0.957557813108254));
#44879=DIRECTION('center_axis',(-3.66113466765132E-16,-1.,-1.12027918221652E-15));
#44880=DIRECTION('ref_axis',(-0.288241278368206,1.17826109748215E-15,-0.957557813108254));
#44881=DIRECTION('',(-3.66113466765132E-16,-1.,-1.12027918221652E-15));
#44882=DIRECTION('center_axis',(3.66113466765132E-16,1.,1.12027918221652E-15));
#44883=DIRECTION('ref_axis',(-0.459871139785583,-8.26426833283405E-16,0.887985661366392));
#44884=DIRECTION('',(3.66113466765132E-16,1.,1.12027918221652E-15));
#44885=DIRECTION('center_axis',(-3.66113466765132E-16,-1.,-1.12027918221652E-15));
#44886=DIRECTION('ref_axis',(-0.459871139785583,-8.26426833283405E-16,0.887985661366392));
#44887=DIRECTION('center_axis',(3.66113466765132E-16,1.,1.12027918221652E-15));
#44888=DIRECTION('ref_axis',(-0.998795456205173,4.20641961129317E-16,-0.0490676743274121));
#44889=DIRECTION('',(3.66113466765132E-16,1.,1.12027918221652E-15));
#44890=DIRECTION('center_axis',(-3.66113466765132E-16,-1.,-1.12027918221652E-15));
#44891=DIRECTION('ref_axis',(-0.998795456205173,4.20641961129317E-16,-0.0490676743274121));
#44892=DIRECTION('',(3.66113466765132E-16,1.,1.12027918221652E-15));
#44893=DIRECTION('center_axis',(3.66113466765132E-16,1.,1.12027918221652E-15));
#44894=DIRECTION('ref_axis',(-0.410761709449556,1.17179180099979E-15,-0.91174273676848));
#44895=DIRECTION('center_axis',(-3.66113466765132E-16,-1.,-1.12027918221652E-15));
#44896=DIRECTION('ref_axis',(-0.410761709449556,1.17179180099979E-15,-0.91174273676848));
#44897=DIRECTION('',(-3.66113466765132E-16,-1.,-1.12027918221652E-15));
#44898=DIRECTION('center_axis',(3.66113466765132E-16,1.,1.12027918221652E-15));
#44899=DIRECTION('ref_axis',(-0.340031491310375,-9.29036174476144E-16,0.940414049723441));
#44900=DIRECTION('',(3.66113466765132E-16,1.,1.12027918221652E-15));
#44901=DIRECTION('center_axis',(-3.66113466765132E-16,-1.,-1.12027918221652E-15));
#44902=DIRECTION('ref_axis',(-0.340031491310375,-9.29036174476144E-16,0.940414049723441));
#44903=DIRECTION('center_axis',(3.66113466765132E-16,1.,1.12027918221652E-15));
#44904=DIRECTION('ref_axis',(5.46077161851015E-15,-1.12027918221652E-15,
1.));
#44905=DIRECTION('center_axis',(-3.66113466765132E-16,-1.,-1.12027918221652E-15));
#44906=DIRECTION('ref_axis',(5.46077161851015E-15,-1.12027918221652E-15,
1.));
#44907=DIRECTION('',(3.66113466765132E-16,1.,1.12027918221652E-15));
#44908=DIRECTION('center_axis',(3.66113466765132E-16,1.,1.12027918221652E-15));
#44909=DIRECTION('ref_axis',(5.46077161851015E-15,-1.12027918221652E-15,
1.));
#44910=DIRECTION('center_axis',(-3.66113466765132E-16,-1.,-1.12027918221652E-15));
#44911=DIRECTION('ref_axis',(5.46077161851015E-15,-1.12027918221652E-15,
1.));
#44912=DIRECTION('center_axis',(3.66113466765132E-16,1.,1.12027918221652E-15));
#44913=DIRECTION('ref_axis',(5.46077161851015E-15,-1.12027918221652E-15,
1.));
#44914=DIRECTION('center_axis',(-3.66113466765132E-16,-1.,-1.12027918221652E-15));
#44915=DIRECTION('ref_axis',(5.46077161851015E-15,-1.12027918221652E-15,
1.));
#44916=DIRECTION('center_axis',(3.66113466765132E-16,1.,1.12027918221652E-15));
#44917=DIRECTION('ref_axis',(5.46077161851015E-15,-1.12027918221652E-15,
1.));
#44918=DIRECTION('center_axis',(-3.66113466765132E-16,-1.,-1.12027918221652E-15));
#44919=DIRECTION('ref_axis',(5.46077161851015E-15,-1.12027918221652E-15,
1.));
#44920=DIRECTION('center_axis',(3.66113466765132E-16,1.,1.12027918221652E-15));
#44921=DIRECTION('ref_axis',(5.46077161851015E-15,-1.12027918221652E-15,
1.));
#44922=DIRECTION('center_axis',(-3.66113466765132E-16,-1.,-1.12027918221652E-15));
#44923=DIRECTION('ref_axis',(5.46077161851015E-15,-1.12027918221652E-15,
1.));
#44924=DIRECTION('center_axis',(3.66113466765132E-16,1.,1.12027918221652E-15));
#44925=DIRECTION('ref_axis',(5.46077161851015E-15,-1.12027918221652E-15,
1.));
#44926=DIRECTION('center_axis',(-3.66113466765132E-16,-1.,-1.12027918221652E-15));
#44927=DIRECTION('ref_axis',(5.46077161851015E-15,-1.12027918221652E-15,
1.));
#44928=DIRECTION('center_axis',(3.66113466765132E-16,1.,1.12027918221652E-15));
#44929=DIRECTION('ref_axis',(5.46077161851015E-15,-1.12027918221652E-15,
1.));
#44930=DIRECTION('center_axis',(-3.66113466765132E-16,-1.,-1.12027918221652E-15));
#44931=DIRECTION('ref_axis',(5.46077161851015E-15,-1.12027918221652E-15,
1.));
#44932=DIRECTION('center_axis',(3.66113466765132E-16,1.,1.12027918221652E-15));
#44933=DIRECTION('ref_axis',(5.46077161851015E-15,-1.12027918221652E-15,
1.));
#44934=DIRECTION('center_axis',(-3.66113466765132E-16,-1.,-1.12027918221652E-15));
#44935=DIRECTION('ref_axis',(5.46077161851015E-15,-1.12027918221652E-15,
1.));
#44936=DIRECTION('center_axis',(3.66113466765132E-16,1.,1.12027918221652E-15));
#44937=DIRECTION('ref_axis',(5.46077161851015E-15,-1.12027918221652E-15,
1.));
#44938=DIRECTION('center_axis',(-3.66113466765132E-16,-1.,-1.12027918221652E-15));
#44939=DIRECTION('ref_axis',(5.46077161851015E-15,-1.12027918221652E-15,
1.));
#44940=DIRECTION('center_axis',(3.66113466765132E-16,1.,1.12027918221652E-15));
#44941=DIRECTION('ref_axis',(5.46077161851015E-15,-1.12027918221652E-15,
1.));
#44942=DIRECTION('center_axis',(-3.66113466765132E-16,-1.,-1.12027918221652E-15));
#44943=DIRECTION('ref_axis',(5.46077161851015E-15,-1.12027918221652E-15,
1.));
#44944=DIRECTION('center_axis',(3.66113466765132E-16,1.,1.12027918221652E-15));
#44945=DIRECTION('ref_axis',(5.46077161851015E-15,-1.12027918221652E-15,
1.));
#44946=DIRECTION('center_axis',(-3.66113466765132E-16,-1.,-1.12027918221652E-15));
#44947=DIRECTION('ref_axis',(5.46077161851015E-15,-1.12027918221652E-15,
1.));
#44948=DIRECTION('center_axis',(3.66113466765132E-16,1.,1.12027918221652E-15));
#44949=DIRECTION('ref_axis',(5.46077161851015E-15,-1.12027918221652E-15,
1.));
#44950=DIRECTION('center_axis',(-3.66113466765132E-16,-1.,-1.12027918221652E-15));
#44951=DIRECTION('ref_axis',(5.46077161851015E-15,-1.12027918221652E-15,
1.));
#44952=DIRECTION('center_axis',(3.66113466765132E-16,1.,1.12027918221652E-15));
#44953=DIRECTION('ref_axis',(-5.78239614844548E-15,1.12027918221652E-15,
-1.));
#44954=DIRECTION('center_axis',(-3.66113466765132E-16,-1.,-1.12027918221652E-15));
#44955=DIRECTION('ref_axis',(5.46077161851015E-15,-1.12027918221652E-15,
1.));
#44956=DIRECTION('center_axis',(3.66113466765132E-16,1.,1.12027918221652E-15));
#44957=DIRECTION('ref_axis',(5.46077161851015E-15,-1.12027918221652E-15,
1.));
#44958=DIRECTION('center_axis',(-3.66113466765132E-16,-1.,-1.12027918221652E-15));
#44959=DIRECTION('ref_axis',(5.46077161851015E-15,-1.12027918221652E-15,
1.));
#44960=DIRECTION('center_axis',(3.66113466765132E-16,1.,1.12027918221652E-15));
#44961=DIRECTION('ref_axis',(5.46077161851015E-15,-1.12027918221652E-15,
1.));
#44962=DIRECTION('center_axis',(-3.66113466765132E-16,-1.,-1.12027918221652E-15));
#44963=DIRECTION('ref_axis',(5.46077161851015E-15,-1.12027918221652E-15,
1.));
#44964=DIRECTION('center_axis',(3.66113466765132E-16,1.,1.12027918221652E-15));
#44965=DIRECTION('ref_axis',(5.46077161851015E-15,-1.12027918221652E-15,
1.));
#44966=DIRECTION('center_axis',(-3.66113466765132E-16,-1.,-1.12027918221652E-15));
#44967=DIRECTION('ref_axis',(5.46077161851015E-15,-1.12027918221652E-15,
1.));
#44968=DIRECTION('center_axis',(3.66113466765132E-16,1.,1.12027918221652E-15));
#44969=DIRECTION('ref_axis',(5.46077161851015E-15,-1.12027918221652E-15,
1.));
#44970=DIRECTION('center_axis',(-3.66113466765132E-16,-1.,-1.12027918221652E-15));
#44971=DIRECTION('ref_axis',(5.46077161851015E-15,-1.12027918221652E-15,
1.));
#44972=DIRECTION('center_axis',(3.66113466765132E-16,1.,1.12027918221652E-15));
#44973=DIRECTION('ref_axis',(5.46077161851015E-15,-1.12027918221652E-15,
1.));
#44974=DIRECTION('center_axis',(-3.66113466765132E-16,-1.,-1.12027918221652E-15));
#44975=DIRECTION('ref_axis',(5.46077161851015E-15,-1.12027918221652E-15,
1.));
#44976=DIRECTION('center_axis',(3.66113466765132E-16,1.,1.12027918221652E-15));
#44977=DIRECTION('ref_axis',(5.46077161851015E-15,-1.12027918221652E-15,
1.));
#44978=DIRECTION('center_axis',(-3.66113466765132E-16,-1.,-1.12027918221652E-15));
#44979=DIRECTION('ref_axis',(5.46077161851015E-15,-1.12027918221652E-15,
1.));
#44980=DIRECTION('center_axis',(3.66113466765132E-16,1.,1.12027918221652E-15));
#44981=DIRECTION('ref_axis',(5.46077161851015E-15,-1.12027918221652E-15,
1.));
#44982=DIRECTION('center_axis',(-3.66113466765132E-16,-1.,-1.12027918221652E-15));
#44983=DIRECTION('ref_axis',(5.46077161851015E-15,-1.12027918221652E-15,
1.));
#44984=DIRECTION('center_axis',(3.66113466765132E-16,1.,1.12027918221652E-15));
#44985=DIRECTION('ref_axis',(5.46077161851015E-15,-1.12027918221652E-15,
1.));
#44986=DIRECTION('center_axis',(-3.66113466765132E-16,-1.,-1.12027918221652E-15));
#44987=DIRECTION('ref_axis',(5.46077161851015E-15,-1.12027918221652E-15,
1.));
#44988=DIRECTION('center_axis',(3.66113466765132E-16,1.,1.12027918221652E-15));
#44989=DIRECTION('ref_axis',(5.46077161851015E-15,-1.12027918221652E-15,
1.));
#44990=DIRECTION('center_axis',(-3.66113466765132E-16,-1.,-1.12027918221652E-15));
#44991=DIRECTION('ref_axis',(5.46077161851015E-15,-1.12027918221652E-15,
1.));
#44992=DIRECTION('center_axis',(3.66113466765132E-16,1.,1.12027918221652E-15));
#44993=DIRECTION('ref_axis',(5.46077161851015E-15,-1.12027918221652E-15,
1.));
#44994=DIRECTION('center_axis',(-3.66113466765132E-16,-1.,-1.12027918221652E-15));
#44995=DIRECTION('ref_axis',(5.46077161851015E-15,-1.12027918221652E-15,
1.));
#44996=DIRECTION('center_axis',(3.66113466765132E-16,1.,1.12027918221652E-15));
#44997=DIRECTION('ref_axis',(5.46077161851015E-15,-1.12027918221652E-15,
1.));
#44998=DIRECTION('center_axis',(-3.66113466765132E-16,-1.,-1.12027918221652E-15));
#44999=DIRECTION('ref_axis',(5.46077161851015E-15,-1.12027918221652E-15,
1.));
#45000=DIRECTION('center_axis',(3.66113466765132E-16,1.,1.12027918221652E-15));
#45001=DIRECTION('ref_axis',(5.46077161851015E-15,-1.12027918221652E-15,
1.));
#45002=DIRECTION('center_axis',(-3.66113466765132E-16,-1.,-1.12027918221652E-15));
#45003=DIRECTION('ref_axis',(5.46077161851015E-15,-1.12027918221652E-15,
1.));
#45004=DIRECTION('center_axis',(3.66113466765132E-16,1.,1.12027918221652E-15));
#45005=DIRECTION('ref_axis',(5.46077161851015E-15,-1.12027918221652E-15,
1.));
#45006=DIRECTION('center_axis',(-3.66113466765132E-16,-1.,-1.12027918221652E-15));
#45007=DIRECTION('ref_axis',(5.46077161851015E-15,-1.12027918221652E-15,
1.));
#45008=DIRECTION('center_axis',(3.66113466765132E-16,1.,1.12027918221652E-15));
#45009=DIRECTION('ref_axis',(5.46077161851015E-15,-1.12027918221652E-15,
1.));
#45010=DIRECTION('center_axis',(-3.66113466765132E-16,-1.,-1.12027918221652E-15));
#45011=DIRECTION('ref_axis',(5.46077161851015E-15,-1.12027918221652E-15,
1.));
#45012=DIRECTION('center_axis',(3.66113466765132E-16,1.,1.12027918221652E-15));
#45013=DIRECTION('ref_axis',(5.46077161851015E-15,-1.12027918221652E-15,
1.));
#45014=DIRECTION('center_axis',(-3.66113466765132E-16,-1.,-1.12027918221652E-15));
#45015=DIRECTION('ref_axis',(5.46077161851015E-15,-1.12027918221652E-15,
1.));
#45016=DIRECTION('center_axis',(3.66113466765132E-16,1.,1.12027918221652E-15));
#45017=DIRECTION('ref_axis',(5.46077161851015E-15,-1.12027918221652E-15,
1.));
#45018=DIRECTION('center_axis',(-3.66113466765132E-16,-1.,-1.12027918221652E-15));
#45019=DIRECTION('ref_axis',(5.46077161851015E-15,-1.12027918221652E-15,
1.));
#45020=DIRECTION('center_axis',(3.66113466765132E-16,1.,1.12027918221652E-15));
#45021=DIRECTION('ref_axis',(5.46077161851015E-15,-1.12027918221652E-15,
1.));
#45022=DIRECTION('center_axis',(-3.66113466765132E-16,-1.,-1.12027918221652E-15));
#45023=DIRECTION('ref_axis',(5.46077161851015E-15,-1.12027918221652E-15,
1.));
#45024=DIRECTION('center_axis',(3.66113466765132E-16,1.,1.12027918221652E-15));
#45025=DIRECTION('ref_axis',(5.46077161851015E-15,-1.12027918221652E-15,
1.));
#45026=DIRECTION('center_axis',(-3.66113466765132E-16,-1.,-1.12027918221652E-15));
#45027=DIRECTION('ref_axis',(5.46077161851015E-15,-1.12027918221652E-15,
1.));
#45028=DIRECTION('center_axis',(3.66113466765132E-16,1.,1.12027918221652E-15));
#45029=DIRECTION('ref_axis',(5.46077161851015E-15,-1.12027918221652E-15,
1.));
#45030=DIRECTION('center_axis',(-3.66113466765132E-16,-1.,-1.12027918221652E-15));
#45031=DIRECTION('ref_axis',(5.46077161851015E-15,-1.12027918221652E-15,
1.));
#45032=DIRECTION('center_axis',(3.66113466765132E-16,1.,1.12027918221652E-15));
#45033=DIRECTION('ref_axis',(5.46077161851015E-15,-1.12027918221652E-15,
1.));
#45034=DIRECTION('center_axis',(-3.66113466765132E-16,-1.,-1.12027918221652E-15));
#45035=DIRECTION('ref_axis',(5.46077161851015E-15,-1.12027918221652E-15,
1.));
#45036=DIRECTION('center_axis',(3.66113466765132E-16,1.,1.12027918221652E-15));
#45037=DIRECTION('ref_axis',(5.46077161851015E-15,-1.12027918221652E-15,
1.));
#45038=DIRECTION('center_axis',(-3.66113466765132E-16,-1.,-1.12027918221652E-15));
#45039=DIRECTION('ref_axis',(5.46077161851015E-15,-1.12027918221652E-15,
1.));
#45040=DIRECTION('center_axis',(3.66113466765132E-16,1.,1.12027918221652E-15));
#45041=DIRECTION('ref_axis',(5.46077161851015E-15,-1.12027918221652E-15,
1.));
#45042=DIRECTION('center_axis',(-3.66113466765132E-16,-1.,-1.12027918221652E-15));
#45043=DIRECTION('ref_axis',(5.46077161851015E-15,-1.12027918221652E-15,
1.));
#45044=DIRECTION('center_axis',(3.66113466765132E-16,1.,1.12027918221652E-15));
#45045=DIRECTION('ref_axis',(5.46077161851015E-15,-1.12027918221652E-15,
1.));
#45046=DIRECTION('center_axis',(-3.66113466765132E-16,-1.,-1.12027918221652E-15));
#45047=DIRECTION('ref_axis',(5.46077161851015E-15,-1.12027918221652E-15,
1.));
#45048=DIRECTION('center_axis',(3.66113466765132E-16,1.,1.12027918221652E-15));
#45049=DIRECTION('ref_axis',(5.46077161851015E-15,-1.12027918221652E-15,
1.));
#45050=DIRECTION('center_axis',(-3.66113466765132E-16,-1.,-1.12027918221652E-15));
#45051=DIRECTION('ref_axis',(5.46077161851015E-15,-1.12027918221652E-15,
1.));
#45052=DIRECTION('center_axis',(3.66113466765132E-16,1.,1.12027918221652E-15));
#45053=DIRECTION('ref_axis',(5.46077161851015E-15,-1.12027918221652E-15,
1.));
#45054=DIRECTION('center_axis',(-3.66113466765132E-16,-1.,-1.12027918221652E-15));
#45055=DIRECTION('ref_axis',(5.46077161851015E-15,-1.12027918221652E-15,
1.));
#45056=DIRECTION('center_axis',(3.66113466765132E-16,1.,1.12027918221652E-15));
#45057=DIRECTION('ref_axis',(5.46077161851015E-15,-1.12027918221652E-15,
1.));
#45058=DIRECTION('center_axis',(-3.66113466765132E-16,-1.,-1.12027918221652E-15));
#45059=DIRECTION('ref_axis',(5.46077161851015E-15,-1.12027918221652E-15,
1.));
#45060=DIRECTION('center_axis',(3.66113466765132E-16,1.,1.12027918221652E-15));
#45061=DIRECTION('ref_axis',(5.46077161851015E-15,-1.12027918221652E-15,
1.));
#45062=DIRECTION('center_axis',(-3.66113466765132E-16,-1.,-1.12027918221652E-15));
#45063=DIRECTION('ref_axis',(5.46077161851015E-15,-1.12027918221652E-15,
1.));
#45064=DIRECTION('center_axis',(3.66113466765132E-16,1.,1.12027918221652E-15));
#45065=DIRECTION('ref_axis',(5.46077161851015E-15,-1.12027918221652E-15,
1.));
#45066=DIRECTION('center_axis',(-3.66113466765132E-16,-1.,-1.12027918221652E-15));
#45067=DIRECTION('ref_axis',(5.46077161851015E-15,-1.12027918221652E-15,
1.));
#45068=DIRECTION('center_axis',(3.66113466765132E-16,1.,1.12027918221652E-15));
#45069=DIRECTION('ref_axis',(5.46077161851015E-15,-1.12027918221652E-15,
1.));
#45070=DIRECTION('center_axis',(-3.66113466765132E-16,-1.,-1.12027918221652E-15));
#45071=DIRECTION('ref_axis',(5.46077161851015E-15,-1.12027918221652E-15,
1.));
#45072=DIRECTION('center_axis',(3.66113466765132E-16,1.,1.12027918221652E-15));
#45073=DIRECTION('ref_axis',(5.46077161851015E-15,-1.12027918221652E-15,
1.));
#45074=DIRECTION('center_axis',(-3.66113466765132E-16,-1.,-1.12027918221652E-15));
#45075=DIRECTION('ref_axis',(5.46077161851015E-15,-1.12027918221652E-15,
1.));
#45076=DIRECTION('center_axis',(3.66113466765132E-16,1.,1.12027918221652E-15));
#45077=DIRECTION('ref_axis',(5.46077161851015E-15,-1.12027918221652E-15,
1.));
#45078=DIRECTION('center_axis',(-3.66113466765132E-16,-1.,-1.12027918221652E-15));
#45079=DIRECTION('ref_axis',(5.46077161851015E-15,-1.12027918221652E-15,
1.));
#45080=DIRECTION('center_axis',(3.66113466765132E-16,1.,1.12027918221652E-15));
#45081=DIRECTION('ref_axis',(5.46077161851015E-15,-1.12027918221652E-15,
1.));
#45082=DIRECTION('center_axis',(-3.66113466765132E-16,-1.,-1.12027918221652E-15));
#45083=DIRECTION('ref_axis',(5.46077161851015E-15,-1.12027918221652E-15,
1.));
#45084=DIRECTION('center_axis',(3.66113466765132E-16,1.,1.12027918221652E-15));
#45085=DIRECTION('ref_axis',(5.46077161851015E-15,-1.12027918221652E-15,
1.));
#45086=DIRECTION('center_axis',(-3.66113466765132E-16,-1.,-1.12027918221652E-15));
#45087=DIRECTION('ref_axis',(5.46077161851015E-15,-1.12027918221652E-15,
1.));
#45088=DIRECTION('center_axis',(3.66113466765132E-16,1.,1.12027918221652E-15));
#45089=DIRECTION('ref_axis',(5.46077161851015E-15,-1.12027918221652E-15,
1.));
#45090=DIRECTION('center_axis',(-3.66113466765132E-16,-1.,-1.12027918221652E-15));
#45091=DIRECTION('ref_axis',(5.46077161851015E-15,-1.12027918221652E-15,
1.));
#45092=DIRECTION('center_axis',(3.66113466765132E-16,1.,1.12027918221652E-15));
#45093=DIRECTION('ref_axis',(-0.99665523930918,2.73338486732788E-16,0.0817210741336742));
#45094=DIRECTION('',(3.66113466765132E-16,1.,1.12027918221652E-15));
#45095=DIRECTION('center_axis',(-3.66113466765132E-16,-1.,-1.12027918221652E-15));
#45096=DIRECTION('ref_axis',(-0.99665523930918,2.73338486732788E-16,0.0817210741336742));
#45097=DIRECTION('',(3.66113466765132E-16,1.,1.12027918221652E-15));
#45098=DIRECTION('center_axis',(3.66113466765132E-16,1.,1.12027918221652E-15));
#45099=DIRECTION('ref_axis',(-0.526253893797564,1.14527282192027E-15,-0.850327489419754));
#45100=DIRECTION('center_axis',(-3.66113466765132E-16,-1.,-1.12027918221652E-15));
#45101=DIRECTION('ref_axis',(-0.526253893797564,1.14527282192027E-15,-0.850327489419754));
#45102=DIRECTION('',(-3.66113466765132E-16,-1.,-1.12027918221652E-15));
#45103=DIRECTION('center_axis',(3.66113466765132E-16,1.,1.12027918221652E-15));
#45104=DIRECTION('ref_axis',(-0.214373809744306,-1.01574944914611E-15,0.976751692957689));
#45105=DIRECTION('center_axis',(-3.66113466765132E-16,-1.,-1.12027918221652E-15));
#45106=DIRECTION('ref_axis',(-0.214373809744306,-1.01574944914611E-15,0.976751692957689));
#45107=DIRECTION('center_axis',(3.66113466765132E-16,1.,1.12027918221652E-15));
#45108=DIRECTION('ref_axis',(5.46077161851015E-15,-1.12027918221652E-15,
1.));
#45109=DIRECTION('center_axis',(-3.66113466765132E-16,-1.,-1.12027918221652E-15));
#45110=DIRECTION('ref_axis',(5.46077161851015E-15,-1.12027918221652E-15,
1.));
#45111=DIRECTION('center_axis',(-3.66113466765132E-16,-1.,-1.12027918221652E-15));
#45112=DIRECTION('ref_axis',(5.46077161851015E-15,-1.12027918221652E-15,
1.));
#45113=DIRECTION('axis',(0.,0.,1.));
#45114=DIRECTION('refdir',(1.,0.,0.));
#45115=DIRECTION('center_axis',(3.66113466765123E-16,1.,-5.66153840231349E-16));
#45116=DIRECTION('ref_axis',(0.996957691137886,-2.96059473233375E-16,0.0779446090567888));
#45117=DIRECTION('center_axis',(-3.66113466765123E-16,-1.,5.66153840231349E-16));
#45118=DIRECTION('ref_axis',(-0.996957691137886,3.20870996777813E-16,-0.0779446090567869));
#45119=DIRECTION('center_axis',(-0.0779446090567859,5.92967996423326E-16,
0.996957691137886));
#45120=DIRECTION('ref_axis',(-0.996957691137886,3.33066907387547E-16,-0.0779446090567859));
#45121=DIRECTION('center_axis',(3.66113466765123E-16,1.,-5.66153840231349E-16));
#45122=DIRECTION('ref_axis',(-0.996957691137886,3.20870996777813E-16,-0.0779446090567869));
#45123=DIRECTION('center_axis',(3.66113466765123E-16,1.,-5.66153840231349E-16));
#45124=DIRECTION('ref_axis',(-0.996957691137886,3.20870996777813E-16,-0.0779446090567869));
#45125=DIRECTION('center_axis',(3.66113466765123E-16,1.,-5.66153840231349E-16));
#45126=DIRECTION('ref_axis',(-0.996957691137886,3.20870996777813E-16,-0.0779446090567869));
#45127=DIRECTION('',(-3.66113466765123E-16,-1.,5.66153840231349E-16));
#45128=DIRECTION('center_axis',(-3.66113466765123E-16,-1.,5.66153840231349E-16));
#45129=DIRECTION('ref_axis',(-0.996957691137886,3.20870996777813E-16,-0.0779446090567869));
#45130=DIRECTION('center_axis',(3.66113466765123E-16,1.,-5.66153840231349E-16));
#45131=DIRECTION('ref_axis',(0.996957691137886,-3.20870996777813E-16,0.0779446090567869));
#45132=DIRECTION('',(0.0779446090567869,-5.92967996423326E-16,-0.996957691137886));
#45133=DIRECTION('',(0.996957691137886,-3.20870996777813E-16,0.0779446090567869));
#45134=DIRECTION('',(-0.0779446090567869,5.92967996423326E-16,0.996957691137886));
#45135=DIRECTION('center_axis',(-3.66113466765123E-16,-1.,5.66153840231349E-16));
#45136=DIRECTION('ref_axis',(0.327345662251861,4.15115746948114E-16,0.944904660484268));
#45137=DIRECTION('center_axis',(-3.66113466765123E-16,-1.,5.66153840231349E-16));
#45138=DIRECTION('ref_axis',(-0.996957691137886,3.1347473636475E-16,-0.0779446090567884));
#45139=DIRECTION('center_axis',(3.66113466765123E-16,1.,-5.66153840231349E-16));
#45140=DIRECTION('ref_axis',(-0.996957691137886,3.20870996777813E-16,-0.0779446090567869));
#45141=DIRECTION('center_axis',(0.077944609056788,-5.92967996423326E-16,
-0.996957691137886));
#45142=DIRECTION('ref_axis',(0.996957691137886,-3.26536183713281E-16,0.077944609056788));
#45143=DIRECTION('center_axis',(-3.66113466765123E-16,-1.,5.66153840231349E-16));
#45144=DIRECTION('ref_axis',(-0.996957691137886,3.20870996777813E-16,-0.0779446090567869));
#45145=DIRECTION('center_axis',(3.66113466765123E-16,1.,-5.66153840231349E-16));
#45146=DIRECTION('ref_axis',(-0.993453242215613,2.99039498345089E-16,-0.114239465734422));
#45147=DIRECTION('center_axis',(3.66113466765123E-16,1.,-5.66153840231349E-16));
#45148=DIRECTION('ref_axis',(-0.176304286675074,-4.92738071143036E-16,-0.984335714327177));
#45149=DIRECTION('center_axis',(3.66113466765123E-16,1.,-5.66153840231349E-16));
#45150=DIRECTION('ref_axis',(0.798717078866636,-6.33079672938476E-16,-0.601706762407361));
#45151=DIRECTION('center_axis',(-3.66113466765123E-16,-1.,5.66153840231349E-16));
#45152=DIRECTION('ref_axis',(-0.996957691137886,3.20870996777813E-16,-0.0779446090567869));
#45153=DIRECTION('center_axis',(3.66113466765123E-16,1.,-5.66153840231349E-16));
#45154=DIRECTION('ref_axis',(-0.999093173971444,3.89886789042682E-16,0.0425773381467764));
#45155=DIRECTION('center_axis',(3.66113466765123E-16,1.,-5.66153840231349E-16));
#45156=DIRECTION('ref_axis',(-0.328117719236679,-4.14681459743577E-16,-0.944636841502024));
#45157=DIRECTION('center_axis',(3.66113466765123E-16,1.,-5.66153840231349E-16));
#45158=DIRECTION('ref_axis',(0.694755870742498,-6.61563157380586E-16,-0.719245632637998));
#45159=DIRECTION('center_axis',(-3.66113466765123E-16,-1.,5.66153840231349E-16));
#45160=DIRECTION('ref_axis',(-0.996957691137886,3.20870996777813E-16,-0.0779446090567869));
#45161=DIRECTION('center_axis',(3.66113466765123E-16,1.,-5.66153840231349E-16));
#45162=DIRECTION('ref_axis',(-0.980132115983957,4.71133773033976E-16,0.198345746656716));
#45163=DIRECTION('center_axis',(3.66113466765123E-16,1.,-5.66153840231349E-16));
#45164=DIRECTION('ref_axis',(-0.471851804590399,-3.26414014556371E-16,-0.881677874569156));
#45165=DIRECTION('center_axis',(3.66113466765123E-16,1.,-5.66153840231349E-16));
#45166=DIRECTION('ref_axis',(0.573687467318141,-6.73756761285746E-16,-0.819074288353686));
#45167=DIRECTION('center_axis',(-3.66113466765123E-16,-1.,5.66153840231349E-16));
#45168=DIRECTION('ref_axis',(-0.996957691137886,3.20870996777813E-16,-0.0779446090567869));
#45169=DIRECTION('center_axis',(3.66113466765123E-16,1.,-5.66153840231349E-16));
#45170=DIRECTION('ref_axis',(-0.937036952428947,5.40779879929828E-16,0.349230224612176));
#45171=DIRECTION('center_axis',(3.66113466765123E-16,1.,-5.66153840231349E-16));
#45172=DIRECTION('ref_axis',(-0.603967332528746,-2.30109173024781E-16,-0.797009072243291));
#45173=DIRECTION('center_axis',(3.66113466765123E-16,1.,-5.66153840231349E-16));
#45174=DIRECTION('ref_axis',(0.438492974488865,-6.6936023765756E-16,-0.898734616738394));
#45175=DIRECTION('center_axis',(-3.66113466765123E-16,-1.,5.66153840231349E-16));
#45176=DIRECTION('ref_axis',(-0.996957691137886,3.20870996777813E-16,-0.0779446090567869));
#45177=DIRECTION('center_axis',(3.66113466765123E-16,1.,-5.66153840231349E-16));
#45178=DIRECTION('ref_axis',(-0.870868829257786,5.97110191436282E-16,0.491515495409018));
#45179=DIRECTION('center_axis',(3.66113466765123E-16,1.,-5.66153840231349E-16));
#45180=DIRECTION('ref_axis',(-0.721211180287579,-1.28138279964759E-16,-0.692715261437336));
#45181=DIRECTION('center_axis',(3.66113466765123E-16,1.,-5.66153840231349E-16));
#45182=DIRECTION('ref_axis',(0.292501329352925,-6.48481843498979E-16,-0.956265116129817));
#45183=DIRECTION('center_axis',(-3.66113466765123E-16,-1.,5.66153840231349E-16));
#45184=DIRECTION('ref_axis',(-0.996957691137886,3.20870996777813E-16,-0.0779446090567869));
#45185=DIRECTION('center_axis',(3.66113466765123E-16,1.,-5.66153840231349E-16));
#45186=DIRECTION('ref_axis',(-0.78325702526236,6.38737668334465E-16,0.621698023462484));
#45187=DIRECTION('center_axis',(3.66113466765123E-16,1.,-5.66153840231349E-16));
#45188=DIRECTION('ref_axis',(-0.820696415225053,-2.30121971854362E-17,-0.571364501904649));
#45189=DIRECTION('center_axis',(3.66113466765123E-16,1.,-5.66153840231349E-16));
#45190=DIRECTION('ref_axis',(0.139307330732061,-6.11635674165605E-16,-0.990249194700156));
#45191=DIRECTION('center_axis',(-3.66113466765123E-16,-1.,5.66153840231349E-16));
#45192=DIRECTION('ref_axis',(-0.996957691137886,3.20870996777813E-16,-0.0779446090567869));
#45193=DIRECTION('center_axis',(3.66113466765123E-16,1.,-5.66153840231349E-16));
#45194=DIRECTION('ref_axis',(-0.676358833823941,6.64637303989468E-16,0.736572282880858));
#45195=DIRECTION('center_axis',(3.66113466765123E-16,1.,-5.66153840231349E-16));
#45196=DIRECTION('ref_axis',(-0.899973380684442,8.26805222616965E-17,-0.435944852085004));
#45197=DIRECTION('center_axis',(3.66113466765123E-16,1.,-5.66153840231349E-16));
#45198=DIRECTION('ref_axis',(-0.0173168767059515,-5.5972900463185E-16,-0.999850051648321));
#45199=DIRECTION('center_axis',(-3.66113466765123E-16,-1.,5.66153840231349E-16));
#45200=DIRECTION('ref_axis',(-0.996957691137886,3.20870996777813E-16,-0.0779446090567869));
#45201=DIRECTION('center_axis',(3.66113466765123E-16,1.,-5.66153840231349E-16));
#45202=DIRECTION('ref_axis',(-0.552806443190503,6.74171363415503E-16,0.833309688151449));
#45203=DIRECTION('center_axis',(3.66113466765123E-16,1.,-5.66153840231349E-16));
#45204=DIRECTION('ref_axis',(-0.957090014670973,1.86337372849825E-16,-0.289790793189011));
#45205=DIRECTION('center_axis',(3.66113466765123E-16,1.,-5.66153840231349E-16));
#45206=DIRECTION('ref_axis',(-0.173514685168044,-4.94039949369995E-16,-0.98483128201283));
#45207=DIRECTION('center_axis',(-3.66113466765123E-16,-1.,5.66153840231349E-16));
#45208=DIRECTION('ref_axis',(-0.996957691137886,3.20870996777813E-16,-0.0779446090567869));
#45209=DIRECTION('center_axis',(3.66113466765123E-16,1.,-5.66153840231349E-16));
#45210=DIRECTION('ref_axis',(-0.415642123266314,6.67105086427771E-16,0.909528243303456));
#45211=DIRECTION('center_axis',(3.66113466765123E-16,1.,-5.66153840231349E-16));
#45212=DIRECTION('ref_axis',(-0.990639916096657,2.85405978900106E-16,-0.136501123204203));
#45213=DIRECTION('center_axis',(3.66113466765123E-16,1.,-5.66153840231349E-16));
#45214=DIRECTION('ref_axis',(-0.325439986219075,-4.16185990930063E-16,-0.945562697746547));
#45215=DIRECTION('center_axis',(-3.66113466765123E-16,-1.,5.66153840231349E-16));
#45216=DIRECTION('ref_axis',(-0.996957691137886,3.20870996777813E-16,-0.0779446090567869));
#45217=DIRECTION('center_axis',(3.66113466765123E-16,1.,-5.66153840231349E-16));
#45218=DIRECTION('ref_axis',(-0.268243314830189,6.43612468217339E-16,0.963351194554152));
#45219=DIRECTION('center_axis',(3.66113466765123E-16,1.,-5.66153840231349E-16));
#45220=DIRECTION('ref_axis',(-0.999796975042654,3.77446942541727E-16,0.0201496574551479));
#45221=DIRECTION('center_axis',(3.66113466765123E-16,1.,-5.66153840231349E-16));
#45222=DIRECTION('ref_axis',(-0.469351874736002,-3.28084152151318E-16,-0.883011221719068));
#45223=DIRECTION('center_axis',(-3.66113466765123E-16,-1.,5.66153840231349E-16));
#45224=DIRECTION('ref_axis',(-0.996957691137886,3.20870996777813E-16,-0.0779446090567869));
#45225=DIRECTION('center_axis',(3.66113466765123E-16,1.,-5.66153840231349E-16));
#45226=DIRECTION('ref_axis',(-0.114239465734422,6.04271975012079E-16,0.993453242215613));
#45227=DIRECTION('center_axis',(3.66113466765123E-16,1.,-5.66153840231349E-16));
#45228=DIRECTION('ref_axis',(-0.984335714327177,4.60193909783388E-16,0.176304286675074));
#45229=DIRECTION('center_axis',(3.66113466765123E-16,1.,-5.66153840231349E-16));
#45230=DIRECTION('ref_axis',(-0.601706762407361,-2.31903792697734E-16,-0.798717078866636));
#45231=DIRECTION('center_axis',(-3.66113466765123E-16,-1.,5.66153840231349E-16));
#45232=DIRECTION('ref_axis',(-0.996957691137886,3.20870996777813E-16,-0.0779446090567869));
#45233=DIRECTION('center_axis',(3.66113466765123E-16,1.,-5.66153840231349E-16));
#45234=DIRECTION('ref_axis',(0.0425773381467764,5.50052300318313E-16,0.999093173971444));
#45235=DIRECTION('center_axis',(3.66113466765123E-16,1.,-5.66153840231349E-16));
#45236=DIRECTION('ref_axis',(-0.944636841502024,5.31609375670159E-16,0.328117719236679));
#45237=DIRECTION('center_axis',(3.66113466765123E-16,1.,-5.66153840231349E-16));
#45238=DIRECTION('ref_axis',(-0.719245632637998,-1.30013192223369E-16,-0.694755870742498));
#45239=DIRECTION('center_axis',(-3.66113466765123E-16,-1.,5.66153840231349E-16));
#45240=DIRECTION('ref_axis',(-0.996957691137886,3.20870996777813E-16,-0.0779446090567869));
#45241=DIRECTION('center_axis',(3.66113466765123E-16,1.,-5.66153840231349E-16));
#45242=DIRECTION('ref_axis',(0.198345746656716,4.82288512471788E-16,0.980132115983957));
#45243=DIRECTION('center_axis',(3.66113466765123E-16,1.,-5.66153840231349E-16));
#45244=DIRECTION('ref_axis',(-0.881677874569156,5.89934854417565E-16,0.471851804590399));
#45245=DIRECTION('center_axis',(3.66113466765123E-16,1.,-5.66153840231349E-16));
#45246=DIRECTION('ref_axis',(-0.819074288353686,-2.49212354674179E-17,-0.573687467318141));
#45247=DIRECTION('center_axis',(-3.66113466765123E-16,-1.,5.66153840231349E-16));
#45248=DIRECTION('ref_axis',(-0.996957691137886,3.20870996777813E-16,-0.0779446090567869));
#45249=DIRECTION('center_axis',(3.66113466765123E-16,1.,-5.66153840231349E-16));
#45250=DIRECTION('ref_axis',(0.349230224612176,4.02649180824402E-16,0.937036952428947));
#45251=DIRECTION('center_axis',(3.66113466765123E-16,1.,-5.66153840231349E-16));
#45252=DIRECTION('ref_axis',(-0.797009072243291,6.33734179167679E-16,0.603967332528746));
#45253=DIRECTION('center_axis',(3.66113466765123E-16,1.,-5.66153840231349E-16));
#45254=DIRECTION('ref_axis',(-0.898734616738394,8.07843648145798E-17,-0.438492974488865));
#45255=DIRECTION('center_axis',(-3.66113466765123E-16,-1.,5.66153840231349E-16));
#45256=DIRECTION('ref_axis',(-0.996957691137886,3.20870996777813E-16,-0.0779446090567869));
#45257=DIRECTION('center_axis',(3.66113466765123E-16,1.,-5.66153840231349E-16));
#45258=DIRECTION('ref_axis',(0.491515495409017,3.13095290029103E-16,0.870868829257787));
#45259=DIRECTION('center_axis',(3.66113466765123E-16,1.,-5.66153840231349E-16));
#45260=DIRECTION('ref_axis',(-0.692715261437337,6.61928865183528E-16,0.721211180287579));
#45261=DIRECTION('center_axis',(3.66113466765123E-16,1.,-5.66153840231349E-16));
#45262=DIRECTION('ref_axis',(-0.956265116129817,1.84500785926907E-16,-0.292501329352925));
#45263=DIRECTION('center_axis',(-3.66113466765123E-16,-1.,5.66153840231349E-16));
#45264=DIRECTION('ref_axis',(-0.996957691137886,3.20870996777813E-16,-0.0779446090567869));
#45265=DIRECTION('center_axis',(3.66113466765123E-16,1.,-5.66153840231349E-16));
#45266=DIRECTION('ref_axis',(0.621698023462484,2.15831954089593E-16,0.78325702526236));
#45267=DIRECTION('center_axis',(3.66113466765123E-16,1.,-5.66153840231349E-16));
#45268=DIRECTION('ref_axis',(-0.571364501904649,6.73824665722604E-16,0.820696415225053));
#45269=DIRECTION('center_axis',(3.66113466765123E-16,1.,-5.66153840231349E-16));
#45270=DIRECTION('ref_axis',(-0.990249194700156,2.83674185366711E-16,-0.13930733073206));
#45271=DIRECTION('center_axis',(-3.66113466765123E-16,-1.,5.66153840231349E-16));
#45272=DIRECTION('ref_axis',(-0.996957691137886,3.20870996777813E-16,-0.0779446090567869));
#45273=DIRECTION('center_axis',(3.66113466765123E-16,1.,-5.66153840231349E-16));
#45274=DIRECTION('ref_axis',(0.736572282880858,1.1325411913521E-16,0.676358833823941));
#45275=DIRECTION('center_axis',(3.66113466765123E-16,1.,-5.66153840231349E-16));
#45276=DIRECTION('ref_axis',(-0.435944852085004,6.69128666695736E-16,0.899973380684442));
#45277=DIRECTION('center_axis',(3.66113466765123E-16,1.,-5.66153840231349E-16));
#45278=DIRECTION('ref_axis',(-0.999850051648321,3.75862584902141E-16,0.0173168767059515));
#45279=DIRECTION('center_axis',(-3.66113466765123E-16,-1.,5.66153840231349E-16));
#45280=DIRECTION('ref_axis',(-0.996957691137886,3.20870996777813E-16,-0.0779446090567869));
#45281=DIRECTION('center_axis',(3.66113466765123E-16,1.,-5.66153840231349E-16));
#45282=DIRECTION('ref_axis',(0.833309688151449,7.88759189884587E-18,0.552806443190503));
#45283=DIRECTION('center_axis',(3.66113466765123E-16,1.,-5.66153840231349E-16));
#45284=DIRECTION('ref_axis',(-0.289790793189011,6.47956499184093E-16,0.957090014670973));
#45285=DIRECTION('center_axis',(3.66113466765123E-16,1.,-5.66153840231349E-16));
#45286=DIRECTION('ref_axis',(-0.98483128201283,4.5879600018088E-16,0.173514685168044));
#45287=DIRECTION('center_axis',(-3.66113466765123E-16,-1.,5.66153840231349E-16));
#45288=DIRECTION('ref_axis',(-0.996957691137886,3.20870996777813E-16,-0.0779446090567869));
#45289=DIRECTION('center_axis',(3.66113466765123E-16,1.,-5.66153840231349E-16));
#45290=DIRECTION('ref_axis',(0.909528243303456,-9.76731540274849E-17,0.415642123266314));
#45291=DIRECTION('center_axis',(3.66113466765123E-16,1.,-5.66153840231349E-16));
#45292=DIRECTION('ref_axis',(-0.136501123204203,6.10829492218208E-16,0.990639916096657));
#45293=DIRECTION('center_axis',(3.66113466765123E-16,1.,-5.66153840231349E-16));
#45294=DIRECTION('ref_axis',(-0.945562697746547,5.30432335278537E-16,0.325439986219075));
#45295=DIRECTION('center_axis',(-3.66113466765123E-16,-1.,5.66153840231349E-16));
#45296=DIRECTION('ref_axis',(-0.996957691137886,3.20870996777813E-16,-0.0779446090567869));
#45297=DIRECTION('center_axis',(3.66113466765123E-16,1.,-5.66153840231349E-16));
#45298=DIRECTION('ref_axis',(0.963351194554152,-2.00828862743045E-16,0.268243314830189));
#45299=DIRECTION('center_axis',(3.66113466765123E-16,1.,-5.66153840231349E-16));
#45300=DIRECTION('ref_axis',(0.0201496574551478,5.58661835927051E-16,0.999796975042654));
#45301=DIRECTION('center_axis',(3.66113466765123E-16,1.,-5.66153840231349E-16));
#45302=DIRECTION('ref_axis',(-0.883011221719068,5.89007665877645E-16,0.469351874736002));
#45303=DIRECTION('center_axis',(-3.66113466765123E-16,-1.,5.66153840231349E-16));
#45304=DIRECTION('ref_axis',(-0.996957691137886,3.20870996777813E-16,-0.0779446090567869));
#45305=DIRECTION('center_axis',(3.66113466765123E-16,1.,-5.66153840231349E-16));
#45306=DIRECTION('ref_axis',(0.993453242215613,-2.99039498345089E-16,0.114239465734422));
#45307=DIRECTION('center_axis',(3.66113466765123E-16,1.,-5.66153840231349E-16));
#45308=DIRECTION('ref_axis',(0.176304286675074,4.92738071143036E-16,0.984335714327177));
#45309=DIRECTION('center_axis',(3.66113466765123E-16,1.,-5.66153840231349E-16));
#45310=DIRECTION('ref_axis',(-0.798717078866636,6.33079672938476E-16,0.601706762407361));
#45311=DIRECTION('center_axis',(-3.66113466765123E-16,-1.,5.66153840231349E-16));
#45312=DIRECTION('ref_axis',(-0.996957691137886,3.20870996777813E-16,-0.0779446090567869));
#45313=DIRECTION('center_axis',(3.66113466765123E-16,1.,-5.66153840231349E-16));
#45314=DIRECTION('ref_axis',(0.999093173971444,-3.89886789042682E-16,-0.0425773381467764));
#45315=DIRECTION('center_axis',(3.66113466765123E-16,1.,-5.66153840231349E-16));
#45316=DIRECTION('ref_axis',(0.328117719236679,4.14681459743577E-16,0.944636841502024));
#45317=DIRECTION('center_axis',(3.66113466765123E-16,1.,-5.66153840231349E-16));
#45318=DIRECTION('ref_axis',(-0.694755870742498,6.61563157380586E-16,0.719245632637998));
#45319=DIRECTION('center_axis',(-3.66113466765123E-16,-1.,5.66153840231349E-16));
#45320=DIRECTION('ref_axis',(-0.996957691137886,3.20870996777813E-16,-0.0779446090567869));
#45321=DIRECTION('center_axis',(3.66113466765123E-16,1.,-5.66153840231349E-16));
#45322=DIRECTION('ref_axis',(0.980132115983957,-4.71133773033976E-16,-0.198345746656716));
#45323=DIRECTION('center_axis',(3.66113466765123E-16,1.,-5.66153840231349E-16));
#45324=DIRECTION('ref_axis',(0.471851804590399,3.26414014556371E-16,0.881677874569156));
#45325=DIRECTION('center_axis',(3.66113466765123E-16,1.,-5.66153840231349E-16));
#45326=DIRECTION('ref_axis',(-0.573687467318141,6.73756761285746E-16,0.819074288353686));
#45327=DIRECTION('center_axis',(-3.66113466765123E-16,-1.,5.66153840231349E-16));
#45328=DIRECTION('ref_axis',(-0.996957691137886,3.20870996777813E-16,-0.0779446090567869));
#45329=DIRECTION('center_axis',(3.66113466765123E-16,1.,-5.66153840231349E-16));
#45330=DIRECTION('ref_axis',(0.937036952428947,-5.40779879929828E-16,-0.349230224612176));
#45331=DIRECTION('center_axis',(3.66113466765123E-16,1.,-5.66153840231349E-16));
#45332=DIRECTION('ref_axis',(0.603967332528746,2.30109173024781E-16,0.797009072243291));
#45333=DIRECTION('center_axis',(3.66113466765123E-16,1.,-5.66153840231349E-16));
#45334=DIRECTION('ref_axis',(-0.438492974488865,6.6936023765756E-16,0.898734616738394));
#45335=DIRECTION('center_axis',(-3.66113466765123E-16,-1.,5.66153840231349E-16));
#45336=DIRECTION('ref_axis',(-0.996957691137886,3.20870996777813E-16,-0.0779446090567869));
#45337=DIRECTION('center_axis',(3.66113466765123E-16,1.,-5.66153840231349E-16));
#45338=DIRECTION('ref_axis',(0.870868829257786,-5.97110191436282E-16,-0.491515495409018));
#45339=DIRECTION('center_axis',(3.66113466765123E-16,1.,-5.66153840231349E-16));
#45340=DIRECTION('ref_axis',(0.721211180287579,1.2813827996476E-16,0.692715261437337));
#45341=DIRECTION('center_axis',(3.66113466765123E-16,1.,-5.66153840231349E-16));
#45342=DIRECTION('ref_axis',(-0.292501329352925,6.48481843498979E-16,0.956265116129817));
#45343=DIRECTION('center_axis',(-3.66113466765123E-16,-1.,5.66153840231349E-16));
#45344=DIRECTION('ref_axis',(-0.996957691137886,3.20870996777813E-16,-0.0779446090567869));
#45345=DIRECTION('center_axis',(3.66113466765123E-16,1.,-5.66153840231349E-16));
#45346=DIRECTION('ref_axis',(0.78325702526236,-6.38737668334465E-16,-0.621698023462484));
#45347=DIRECTION('center_axis',(3.66113466765123E-16,1.,-5.66153840231349E-16));
#45348=DIRECTION('ref_axis',(0.820696415225053,2.30121971854362E-17,0.571364501904649));
#45349=DIRECTION('center_axis',(3.66113466765123E-16,1.,-5.66153840231349E-16));
#45350=DIRECTION('ref_axis',(-0.13930733073206,6.11635674165605E-16,0.990249194700156));
#45351=DIRECTION('center_axis',(-3.66113466765123E-16,-1.,5.66153840231349E-16));
#45352=DIRECTION('ref_axis',(-0.996957691137886,3.20870996777813E-16,-0.0779446090567869));
#45353=DIRECTION('center_axis',(3.66113466765123E-16,1.,-5.66153840231349E-16));
#45354=DIRECTION('ref_axis',(0.676358833823941,-6.64637303989468E-16,-0.736572282880858));
#45355=DIRECTION('center_axis',(3.66113466765123E-16,1.,-5.66153840231349E-16));
#45356=DIRECTION('ref_axis',(0.899973380684442,-8.26805222616965E-17,0.435944852085004));
#45357=DIRECTION('center_axis',(3.66113466765123E-16,1.,-5.66153840231349E-16));
#45358=DIRECTION('ref_axis',(0.0173168767059515,5.5972900463185E-16,0.999850051648321));
#45359=DIRECTION('center_axis',(-3.66113466765123E-16,-1.,5.66153840231349E-16));
#45360=DIRECTION('ref_axis',(-0.996957691137886,3.20870996777813E-16,-0.0779446090567869));
#45361=DIRECTION('center_axis',(3.66113466765123E-16,1.,-5.66153840231349E-16));
#45362=DIRECTION('ref_axis',(0.552806443190503,-6.74171363415503E-16,-0.833309688151449));
#45363=DIRECTION('center_axis',(3.66113466765123E-16,1.,-5.66153840231349E-16));
#45364=DIRECTION('ref_axis',(0.957090014670973,-1.86337372849825E-16,0.289790793189011));
#45365=DIRECTION('center_axis',(3.66113466765123E-16,1.,-5.66153840231349E-16));
#45366=DIRECTION('ref_axis',(0.173514685168044,4.94039949369995E-16,0.98483128201283));
#45367=DIRECTION('center_axis',(-3.66113466765123E-16,-1.,5.66153840231349E-16));
#45368=DIRECTION('ref_axis',(-0.996957691137886,3.20870996777813E-16,-0.0779446090567869));
#45369=DIRECTION('center_axis',(3.66113466765123E-16,1.,-5.66153840231349E-16));
#45370=DIRECTION('ref_axis',(0.415642123266314,-6.67105086427771E-16,-0.909528243303456));
#45371=DIRECTION('center_axis',(3.66113466765123E-16,1.,-5.66153840231349E-16));
#45372=DIRECTION('ref_axis',(0.990639916096657,-2.85405978900105E-16,0.136501123204203));
#45373=DIRECTION('center_axis',(3.66113466765123E-16,1.,-5.66153840231349E-16));
#45374=DIRECTION('ref_axis',(0.325439986219075,4.16185990930063E-16,0.945562697746547));
#45375=DIRECTION('center_axis',(-3.66113466765123E-16,-1.,5.66153840231349E-16));
#45376=DIRECTION('ref_axis',(-0.996957691137886,3.20870996777813E-16,-0.0779446090567869));
#45377=DIRECTION('center_axis',(3.66113466765123E-16,1.,-5.66153840231349E-16));
#45378=DIRECTION('ref_axis',(0.268243314830189,-6.43612468217339E-16,-0.963351194554152));
#45379=DIRECTION('center_axis',(3.66113466765123E-16,1.,-5.66153840231349E-16));
#45380=DIRECTION('ref_axis',(0.999796975042654,-3.77446942541727E-16,-0.0201496574551476));
#45381=DIRECTION('center_axis',(3.66113466765123E-16,1.,-5.66153840231349E-16));
#45382=DIRECTION('ref_axis',(0.469351874736002,3.28084152151318E-16,0.883011221719068));
#45383=DIRECTION('center_axis',(-3.66113466765123E-16,-1.,5.66153840231349E-16));
#45384=DIRECTION('ref_axis',(-0.996957691137886,3.20870996777813E-16,-0.0779446090567869));
#45385=DIRECTION('center_axis',(3.66113466765123E-16,1.,-5.66153840231349E-16));
#45386=DIRECTION('ref_axis',(0.114239465734422,-6.04271975012079E-16,-0.993453242215613));
#45387=DIRECTION('center_axis',(3.66113466765123E-16,1.,-5.66153840231349E-16));
#45388=DIRECTION('ref_axis',(0.984335714327177,-4.60193909783388E-16,-0.176304286675074));
#45389=DIRECTION('center_axis',(3.66113466765123E-16,1.,-5.66153840231349E-16));
#45390=DIRECTION('ref_axis',(0.601706762407361,2.31903792697734E-16,0.798717078866636));
#45391=DIRECTION('center_axis',(-3.66113466765123E-16,-1.,5.66153840231349E-16));
#45392=DIRECTION('ref_axis',(-0.996957691137886,3.20870996777813E-16,-0.0779446090567869));
#45393=DIRECTION('center_axis',(3.66113466765123E-16,1.,-5.66153840231349E-16));
#45394=DIRECTION('ref_axis',(-0.0425773381467764,-5.50052300318313E-16,
-0.999093173971444));
#45395=DIRECTION('center_axis',(3.66113466765123E-16,1.,-5.66153840231349E-16));
#45396=DIRECTION('ref_axis',(0.944636841502024,-5.31609375670159E-16,-0.328117719236679));
#45397=DIRECTION('center_axis',(3.66113466765123E-16,1.,-5.66153840231349E-16));
#45398=DIRECTION('ref_axis',(0.719245632637998,1.30013192223369E-16,0.694755870742498));
#45399=DIRECTION('center_axis',(-3.66113466765123E-16,-1.,5.66153840231349E-16));
#45400=DIRECTION('ref_axis',(-0.996957691137886,3.20870996777813E-16,-0.0779446090567869));
#45401=DIRECTION('center_axis',(3.66113466765123E-16,1.,-5.66153840231349E-16));
#45402=DIRECTION('ref_axis',(-0.198345746656716,-4.82288512471788E-16,-0.980132115983957));
#45403=DIRECTION('center_axis',(3.66113466765123E-16,1.,-5.66153840231349E-16));
#45404=DIRECTION('ref_axis',(0.881677874569156,-5.89934854417565E-16,-0.471851804590399));
#45405=DIRECTION('center_axis',(3.66113466765123E-16,1.,-5.66153840231349E-16));
#45406=DIRECTION('ref_axis',(0.819074288353686,2.49212354674179E-17,0.573687467318141));
#45407=DIRECTION('center_axis',(-3.66113466765123E-16,-1.,5.66153840231349E-16));
#45408=DIRECTION('ref_axis',(-0.996957691137886,3.20870996777813E-16,-0.0779446090567869));
#45409=DIRECTION('center_axis',(3.66113466765123E-16,1.,-5.66153840231349E-16));
#45410=DIRECTION('ref_axis',(-0.349230224612176,-4.02649180824402E-16,-0.937036952428947));
#45411=DIRECTION('center_axis',(3.66113466765123E-16,1.,-5.66153840231349E-16));
#45412=DIRECTION('ref_axis',(0.797009072243291,-6.33734179167679E-16,-0.603967332528746));
#45413=DIRECTION('center_axis',(3.66113466765123E-16,1.,-5.66153840231349E-16));
#45414=DIRECTION('ref_axis',(0.898734616738394,-8.07843648145798E-17,0.438492974488865));
#45415=DIRECTION('center_axis',(-3.66113466765123E-16,-1.,5.66153840231349E-16));
#45416=DIRECTION('ref_axis',(-0.996957691137886,3.20870996777813E-16,-0.0779446090567869));
#45417=DIRECTION('center_axis',(3.66113466765123E-16,1.,-5.66153840231349E-16));
#45418=DIRECTION('ref_axis',(-0.491515495409017,-3.13095290029103E-16,-0.870868829257787));
#45419=DIRECTION('center_axis',(3.66113466765123E-16,1.,-5.66153840231349E-16));
#45420=DIRECTION('ref_axis',(0.692715261437337,-6.61928865183528E-16,-0.721211180287579));
#45421=DIRECTION('center_axis',(3.66113466765123E-16,1.,-5.66153840231349E-16));
#45422=DIRECTION('ref_axis',(0.956265116129817,-1.84500785926907E-16,0.292501329352925));
#45423=DIRECTION('center_axis',(-3.66113466765123E-16,-1.,5.66153840231349E-16));
#45424=DIRECTION('ref_axis',(-0.996957691137886,3.20870996777813E-16,-0.0779446090567869));
#45425=DIRECTION('center_axis',(3.66113466765123E-16,1.,-5.66153840231349E-16));
#45426=DIRECTION('ref_axis',(-0.621698023462484,-2.15831954089593E-16,-0.78325702526236));
#45427=DIRECTION('center_axis',(3.66113466765123E-16,1.,-5.66153840231349E-16));
#45428=DIRECTION('ref_axis',(0.571364501904649,-6.73824665722604E-16,-0.820696415225053));
#45429=DIRECTION('center_axis',(3.66113466765123E-16,1.,-5.66153840231349E-16));
#45430=DIRECTION('ref_axis',(0.990249194700156,-2.83674185366711E-16,0.139307330732061));
#45431=DIRECTION('center_axis',(-3.66113466765123E-16,-1.,5.66153840231349E-16));
#45432=DIRECTION('ref_axis',(-0.996957691137886,3.20870996777813E-16,-0.0779446090567869));
#45433=DIRECTION('center_axis',(3.66113466765123E-16,1.,-5.66153840231349E-16));
#45434=DIRECTION('ref_axis',(-0.736572282880858,-1.1325411913521E-16,-0.676358833823941));
#45435=DIRECTION('center_axis',(3.66113466765123E-16,1.,-5.66153840231349E-16));
#45436=DIRECTION('ref_axis',(0.435944852085004,-6.69128666695736E-16,-0.899973380684442));
#45437=DIRECTION('center_axis',(3.66113466765123E-16,1.,-5.66153840231349E-16));
#45438=DIRECTION('ref_axis',(0.999850051648321,-3.75862584902141E-16,-0.0173168767059515));
#45439=DIRECTION('center_axis',(-3.66113466765123E-16,-1.,5.66153840231349E-16));
#45440=DIRECTION('ref_axis',(-0.996957691137886,3.20870996777813E-16,-0.0779446090567869));
#45441=DIRECTION('center_axis',(3.66113466765123E-16,1.,-5.66153840231349E-16));
#45442=DIRECTION('ref_axis',(-0.833309688151449,-7.88759189884587E-18,-0.552806443190503));
#45443=DIRECTION('center_axis',(3.66113466765123E-16,1.,-5.66153840231349E-16));
#45444=DIRECTION('ref_axis',(0.289790793189011,-6.47956499184093E-16,-0.957090014670973));
#45445=DIRECTION('center_axis',(3.66113466765123E-16,1.,-5.66153840231349E-16));
#45446=DIRECTION('ref_axis',(0.98483128201283,-4.5879600018088E-16,-0.173514685168044));
#45447=DIRECTION('center_axis',(-3.66113466765123E-16,-1.,5.66153840231349E-16));
#45448=DIRECTION('ref_axis',(-0.996957691137886,3.20870996777813E-16,-0.0779446090567869));
#45449=DIRECTION('center_axis',(3.66113466765123E-16,1.,-5.66153840231349E-16));
#45450=DIRECTION('ref_axis',(-0.909528243303456,9.76731540274849E-17,-0.415642123266314));
#45451=DIRECTION('center_axis',(3.66113466765123E-16,1.,-5.66153840231349E-16));
#45452=DIRECTION('ref_axis',(0.136501123204203,-6.10829492218208E-16,-0.990639916096657));
#45453=DIRECTION('center_axis',(3.66113466765123E-16,1.,-5.66153840231349E-16));
#45454=DIRECTION('ref_axis',(0.945562697746547,-5.30432335278537E-16,-0.325439986219075));
#45455=DIRECTION('center_axis',(-3.66113466765123E-16,-1.,5.66153840231349E-16));
#45456=DIRECTION('ref_axis',(-0.996957691137886,3.20870996777813E-16,-0.0779446090567869));
#45457=DIRECTION('center_axis',(3.66113466765123E-16,1.,-5.66153840231349E-16));
#45458=DIRECTION('ref_axis',(-0.963351194554152,2.00828862743045E-16,-0.268243314830189));
#45459=DIRECTION('center_axis',(3.66113466765123E-16,1.,-5.66153840231349E-16));
#45460=DIRECTION('ref_axis',(-0.0201496574551477,-5.58661835927051E-16,
-0.999796975042654));
#45461=DIRECTION('center_axis',(3.66113466765123E-16,1.,-5.66153840231349E-16));
#45462=DIRECTION('ref_axis',(0.883011221719068,-5.89007665877645E-16,-0.469351874736002));
#45463=DIRECTION('center_axis',(-3.66113466765123E-16,-1.,5.66153840231349E-16));
#45464=DIRECTION('ref_axis',(-0.996957691137886,3.20870996777813E-16,-0.0779446090567869));
#45465=DIRECTION('center_axis',(0.0779446090567869,-5.92967996423326E-16,
-0.996957691137886));
#45466=DIRECTION('ref_axis',(0.996957691137886,-3.20870996777813E-16,0.0779446090567869));
#45467=DIRECTION('',(-0.996957691137886,3.20870996777813E-16,-0.0779446090567869));
#45468=DIRECTION('',(-3.66113466765123E-16,-1.,5.66153840231349E-16));
#45469=DIRECTION('',(-3.66113466765123E-16,-1.,5.66153840231349E-16));
#45470=DIRECTION('center_axis',(-0.996957691137886,3.20870996777813E-16,
-0.0779446090567869));
#45471=DIRECTION('ref_axis',(0.0779446090567869,-5.92967996423326E-16,-0.996957691137886));
#45472=DIRECTION('',(-0.0779446090567869,5.92967996423326E-16,0.996957691137886));
#45473=DIRECTION('',(3.66113466765123E-16,1.,-5.66153840231349E-16));
#45474=DIRECTION('center_axis',(-3.66113466765123E-16,-1.,5.66153840231349E-16));
#45475=DIRECTION('ref_axis',(-0.0779446090567859,5.92967996423326E-16,0.996957691137886));
#45476=DIRECTION('center_axis',(3.66113466765123E-16,1.,-5.66153840231349E-16));
#45477=DIRECTION('ref_axis',(-0.996957691137886,3.20870996777813E-16,-0.0779446090567869));
#45478=DIRECTION('',(-3.66113466765123E-16,-1.,5.66153840231349E-16));
#45479=DIRECTION('center_axis',(0.996957691137886,-3.20870996777813E-16,
0.0779446090567869));
#45480=DIRECTION('ref_axis',(-0.0779446090567869,5.92967996423326E-16,0.996957691137886));
#45481=DIRECTION('',(0.0779446090567869,-5.92967996423326E-16,-0.996957691137886));
#45482=DIRECTION('center_axis',(3.66113466765123E-16,1.,-5.66153840231349E-16));
#45483=DIRECTION('ref_axis',(-0.176304286675074,-4.92738071143036E-16,-0.984335714327177));
#45484=DIRECTION('',(3.66113466765123E-16,1.,-5.66153840231349E-16));
#45485=DIRECTION('center_axis',(-3.66113466765123E-16,-1.,5.66153840231349E-16));
#45486=DIRECTION('ref_axis',(-0.176304286675074,-4.92738071143036E-16,-0.984335714327177));
#45487=DIRECTION('',(3.66113466765123E-16,1.,-5.66153840231349E-16));
#45488=DIRECTION('center_axis',(3.66113466765123E-16,1.,-5.66153840231349E-16));
#45489=DIRECTION('ref_axis',(0.798717078866636,-6.33079672938476E-16,-0.601706762407361));
#45490=DIRECTION('center_axis',(-3.66113466765123E-16,-1.,5.66153840231349E-16));
#45491=DIRECTION('ref_axis',(0.798717078866636,-6.33079672938476E-16,-0.601706762407361));
#45492=DIRECTION('',(-3.66113466765123E-16,-1.,5.66153840231349E-16));
#45493=DIRECTION('center_axis',(3.66113466765123E-16,1.,-5.66153840231349E-16));
#45494=DIRECTION('ref_axis',(-0.993453242215613,2.99039498345089E-16,-0.114239465734422));
#45495=DIRECTION('',(3.66113466765123E-16,1.,-5.66153840231349E-16));
#45496=DIRECTION('center_axis',(-3.66113466765123E-16,-1.,5.66153840231349E-16));
#45497=DIRECTION('ref_axis',(-0.993453242215613,2.99039498345089E-16,-0.114239465734422));
#45498=DIRECTION('center_axis',(3.66113466765123E-16,1.,-5.66153840231349E-16));
#45499=DIRECTION('ref_axis',(-0.328117719236679,-4.14681459743577E-16,-0.944636841502024));
#45500=DIRECTION('',(3.66113466765123E-16,1.,-5.66153840231349E-16));
#45501=DIRECTION('center_axis',(-3.66113466765123E-16,-1.,5.66153840231349E-16));
#45502=DIRECTION('ref_axis',(-0.328117719236679,-4.14681459743577E-16,-0.944636841502024));
#45503=DIRECTION('',(3.66113466765123E-16,1.,-5.66153840231349E-16));
#45504=DIRECTION('center_axis',(3.66113466765123E-16,1.,-5.66153840231349E-16));
#45505=DIRECTION('ref_axis',(0.694755870742498,-6.61563157380586E-16,-0.719245632637998));
#45506=DIRECTION('center_axis',(-3.66113466765123E-16,-1.,5.66153840231349E-16));
#45507=DIRECTION('ref_axis',(0.694755870742498,-6.61563157380586E-16,-0.719245632637998));
#45508=DIRECTION('',(-3.66113466765123E-16,-1.,5.66153840231349E-16));
#45509=DIRECTION('center_axis',(3.66113466765123E-16,1.,-5.66153840231349E-16));
#45510=DIRECTION('ref_axis',(-0.999093173971444,3.89886789042682E-16,0.0425773381467764));
#45511=DIRECTION('',(3.66113466765123E-16,1.,-5.66153840231349E-16));
#45512=DIRECTION('center_axis',(-3.66113466765123E-16,-1.,5.66153840231349E-16));
#45513=DIRECTION('ref_axis',(-0.999093173971444,3.89886789042682E-16,0.0425773381467764));
#45514=DIRECTION('center_axis',(3.66113466765123E-16,1.,-5.66153840231349E-16));
#45515=DIRECTION('ref_axis',(-0.471851804590399,-3.26414014556371E-16,-0.881677874569156));
#45516=DIRECTION('',(3.66113466765123E-16,1.,-5.66153840231349E-16));
#45517=DIRECTION('center_axis',(-3.66113466765123E-16,-1.,5.66153840231349E-16));
#45518=DIRECTION('ref_axis',(-0.471851804590399,-3.26414014556371E-16,-0.881677874569156));
#45519=DIRECTION('',(3.66113466765123E-16,1.,-5.66153840231349E-16));
#45520=DIRECTION('center_axis',(3.66113466765123E-16,1.,-5.66153840231349E-16));
#45521=DIRECTION('ref_axis',(0.573687467318141,-6.73756761285746E-16,-0.819074288353686));
#45522=DIRECTION('center_axis',(-3.66113466765123E-16,-1.,5.66153840231349E-16));
#45523=DIRECTION('ref_axis',(0.573687467318141,-6.73756761285746E-16,-0.819074288353686));
#45524=DIRECTION('',(-3.66113466765123E-16,-1.,5.66153840231349E-16));
#45525=DIRECTION('center_axis',(3.66113466765123E-16,1.,-5.66153840231349E-16));
#45526=DIRECTION('ref_axis',(-0.980132115983957,4.71133773033976E-16,0.198345746656716));
#45527=DIRECTION('',(3.66113466765123E-16,1.,-5.66153840231349E-16));
#45528=DIRECTION('center_axis',(-3.66113466765123E-16,-1.,5.66153840231349E-16));
#45529=DIRECTION('ref_axis',(-0.980132115983957,4.71133773033976E-16,0.198345746656716));
#45530=DIRECTION('center_axis',(3.66113466765123E-16,1.,-5.66153840231349E-16));
#45531=DIRECTION('ref_axis',(-0.603967332528746,-2.30109173024781E-16,-0.797009072243291));
#45532=DIRECTION('',(3.66113466765123E-16,1.,-5.66153840231349E-16));
#45533=DIRECTION('center_axis',(-3.66113466765123E-16,-1.,5.66153840231349E-16));
#45534=DIRECTION('ref_axis',(-0.603967332528746,-2.30109173024781E-16,-0.797009072243291));
#45535=DIRECTION('',(3.66113466765123E-16,1.,-5.66153840231349E-16));
#45536=DIRECTION('center_axis',(3.66113466765123E-16,1.,-5.66153840231349E-16));
#45537=DIRECTION('ref_axis',(0.438492974488865,-6.6936023765756E-16,-0.898734616738394));
#45538=DIRECTION('center_axis',(-3.66113466765123E-16,-1.,5.66153840231349E-16));
#45539=DIRECTION('ref_axis',(0.438492974488865,-6.6936023765756E-16,-0.898734616738394));
#45540=DIRECTION('',(-3.66113466765123E-16,-1.,5.66153840231349E-16));
#45541=DIRECTION('center_axis',(3.66113466765123E-16,1.,-5.66153840231349E-16));
#45542=DIRECTION('ref_axis',(-0.937036952428947,5.40779879929828E-16,0.349230224612176));
#45543=DIRECTION('',(3.66113466765123E-16,1.,-5.66153840231349E-16));
#45544=DIRECTION('center_axis',(-3.66113466765123E-16,-1.,5.66153840231349E-16));
#45545=DIRECTION('ref_axis',(-0.937036952428947,5.40779879929828E-16,0.349230224612176));
#45546=DIRECTION('center_axis',(3.66113466765123E-16,1.,-5.66153840231349E-16));
#45547=DIRECTION('ref_axis',(-0.721211180287579,-1.28138279964759E-16,-0.692715261437336));
#45548=DIRECTION('',(3.66113466765123E-16,1.,-5.66153840231349E-16));
#45549=DIRECTION('center_axis',(-3.66113466765123E-16,-1.,5.66153840231349E-16));
#45550=DIRECTION('ref_axis',(-0.721211180287579,-1.28138279964759E-16,-0.692715261437336));
#45551=DIRECTION('',(3.66113466765123E-16,1.,-5.66153840231349E-16));
#45552=DIRECTION('center_axis',(3.66113466765123E-16,1.,-5.66153840231349E-16));
#45553=DIRECTION('ref_axis',(0.292501329352925,-6.48481843498979E-16,-0.956265116129817));
#45554=DIRECTION('center_axis',(-3.66113466765123E-16,-1.,5.66153840231349E-16));
#45555=DIRECTION('ref_axis',(0.292501329352925,-6.48481843498979E-16,-0.956265116129817));
#45556=DIRECTION('',(-3.66113466765123E-16,-1.,5.66153840231349E-16));
#45557=DIRECTION('center_axis',(3.66113466765123E-16,1.,-5.66153840231349E-16));
#45558=DIRECTION('ref_axis',(-0.870868829257786,5.97110191436282E-16,0.491515495409018));
#45559=DIRECTION('',(3.66113466765123E-16,1.,-5.66153840231349E-16));
#45560=DIRECTION('center_axis',(-3.66113466765123E-16,-1.,5.66153840231349E-16));
#45561=DIRECTION('ref_axis',(-0.870868829257786,5.97110191436282E-16,0.491515495409018));
#45562=DIRECTION('center_axis',(3.66113466765123E-16,1.,-5.66153840231349E-16));
#45563=DIRECTION('ref_axis',(-0.820696415225053,-2.30121971854362E-17,-0.571364501904649));
#45564=DIRECTION('',(3.66113466765123E-16,1.,-5.66153840231349E-16));
#45565=DIRECTION('center_axis',(-3.66113466765123E-16,-1.,5.66153840231349E-16));
#45566=DIRECTION('ref_axis',(-0.820696415225053,-2.30121971854362E-17,-0.571364501904649));
#45567=DIRECTION('',(3.66113466765123E-16,1.,-5.66153840231349E-16));
#45568=DIRECTION('center_axis',(3.66113466765123E-16,1.,-5.66153840231349E-16));
#45569=DIRECTION('ref_axis',(0.139307330732061,-6.11635674165605E-16,-0.990249194700156));
#45570=DIRECTION('center_axis',(-3.66113466765123E-16,-1.,5.66153840231349E-16));
#45571=DIRECTION('ref_axis',(0.139307330732061,-6.11635674165605E-16,-0.990249194700156));
#45572=DIRECTION('',(-3.66113466765123E-16,-1.,5.66153840231349E-16));
#45573=DIRECTION('center_axis',(3.66113466765123E-16,1.,-5.66153840231349E-16));
#45574=DIRECTION('ref_axis',(-0.78325702526236,6.38737668334465E-16,0.621698023462484));
#45575=DIRECTION('',(3.66113466765123E-16,1.,-5.66153840231349E-16));
#45576=DIRECTION('center_axis',(-3.66113466765123E-16,-1.,5.66153840231349E-16));
#45577=DIRECTION('ref_axis',(-0.78325702526236,6.38737668334465E-16,0.621698023462484));
#45578=DIRECTION('center_axis',(3.66113466765123E-16,1.,-5.66153840231349E-16));
#45579=DIRECTION('ref_axis',(-0.899973380684442,8.26805222616965E-17,-0.435944852085004));
#45580=DIRECTION('',(3.66113466765123E-16,1.,-5.66153840231349E-16));
#45581=DIRECTION('center_axis',(-3.66113466765123E-16,-1.,5.66153840231349E-16));
#45582=DIRECTION('ref_axis',(-0.899973380684442,8.26805222616965E-17,-0.435944852085004));
#45583=DIRECTION('',(3.66113466765123E-16,1.,-5.66153840231349E-16));
#45584=DIRECTION('center_axis',(3.66113466765123E-16,1.,-5.66153840231349E-16));
#45585=DIRECTION('ref_axis',(-0.0173168767059515,-5.5972900463185E-16,-0.999850051648321));
#45586=DIRECTION('center_axis',(-3.66113466765123E-16,-1.,5.66153840231349E-16));
#45587=DIRECTION('ref_axis',(-0.0173168767059515,-5.5972900463185E-16,-0.999850051648321));
#45588=DIRECTION('',(-3.66113466765123E-16,-1.,5.66153840231349E-16));
#45589=DIRECTION('center_axis',(3.66113466765123E-16,1.,-5.66153840231349E-16));
#45590=DIRECTION('ref_axis',(-0.676358833823941,6.64637303989468E-16,0.736572282880858));
#45591=DIRECTION('',(3.66113466765123E-16,1.,-5.66153840231349E-16));
#45592=DIRECTION('center_axis',(-3.66113466765123E-16,-1.,5.66153840231349E-16));
#45593=DIRECTION('ref_axis',(-0.676358833823941,6.64637303989468E-16,0.736572282880858));
#45594=DIRECTION('center_axis',(3.66113466765123E-16,1.,-5.66153840231349E-16));
#45595=DIRECTION('ref_axis',(-0.957090014670973,1.86337372849825E-16,-0.289790793189011));
#45596=DIRECTION('',(3.66113466765123E-16,1.,-5.66153840231349E-16));
#45597=DIRECTION('center_axis',(-3.66113466765123E-16,-1.,5.66153840231349E-16));
#45598=DIRECTION('ref_axis',(-0.957090014670973,1.86337372849825E-16,-0.289790793189011));
#45599=DIRECTION('',(3.66113466765123E-16,1.,-5.66153840231349E-16));
#45600=DIRECTION('center_axis',(3.66113466765123E-16,1.,-5.66153840231349E-16));
#45601=DIRECTION('ref_axis',(-0.173514685168044,-4.94039949369995E-16,-0.98483128201283));
#45602=DIRECTION('center_axis',(-3.66113466765123E-16,-1.,5.66153840231349E-16));
#45603=DIRECTION('ref_axis',(-0.173514685168044,-4.94039949369995E-16,-0.98483128201283));
#45604=DIRECTION('',(-3.66113466765123E-16,-1.,5.66153840231349E-16));
#45605=DIRECTION('center_axis',(3.66113466765123E-16,1.,-5.66153840231349E-16));
#45606=DIRECTION('ref_axis',(-0.552806443190503,6.74171363415503E-16,0.833309688151449));
#45607=DIRECTION('',(3.66113466765123E-16,1.,-5.66153840231349E-16));
#45608=DIRECTION('center_axis',(-3.66113466765123E-16,-1.,5.66153840231349E-16));
#45609=DIRECTION('ref_axis',(-0.552806443190503,6.74171363415503E-16,0.833309688151449));
#45610=DIRECTION('center_axis',(3.66113466765123E-16,1.,-5.66153840231349E-16));
#45611=DIRECTION('ref_axis',(-0.990639916096657,2.85405978900106E-16,-0.136501123204203));
#45612=DIRECTION('',(3.66113466765123E-16,1.,-5.66153840231349E-16));
#45613=DIRECTION('center_axis',(-3.66113466765123E-16,-1.,5.66153840231349E-16));
#45614=DIRECTION('ref_axis',(-0.990639916096657,2.85405978900106E-16,-0.136501123204203));
#45615=DIRECTION('',(3.66113466765123E-16,1.,-5.66153840231349E-16));
#45616=DIRECTION('center_axis',(3.66113466765123E-16,1.,-5.66153840231349E-16));
#45617=DIRECTION('ref_axis',(-0.325439986219075,-4.16185990930063E-16,-0.945562697746547));
#45618=DIRECTION('center_axis',(-3.66113466765123E-16,-1.,5.66153840231349E-16));
#45619=DIRECTION('ref_axis',(-0.325439986219075,-4.16185990930063E-16,-0.945562697746547));
#45620=DIRECTION('',(-3.66113466765123E-16,-1.,5.66153840231349E-16));
#45621=DIRECTION('center_axis',(3.66113466765123E-16,1.,-5.66153840231349E-16));
#45622=DIRECTION('ref_axis',(-0.415642123266314,6.67105086427771E-16,0.909528243303456));
#45623=DIRECTION('',(3.66113466765123E-16,1.,-5.66153840231349E-16));
#45624=DIRECTION('center_axis',(-3.66113466765123E-16,-1.,5.66153840231349E-16));
#45625=DIRECTION('ref_axis',(-0.415642123266314,6.67105086427771E-16,0.909528243303456));
#45626=DIRECTION('center_axis',(3.66113466765123E-16,1.,-5.66153840231349E-16));
#45627=DIRECTION('ref_axis',(-0.999796975042654,3.77446942541727E-16,0.0201496574551479));
#45628=DIRECTION('',(3.66113466765123E-16,1.,-5.66153840231349E-16));
#45629=DIRECTION('center_axis',(-3.66113466765123E-16,-1.,5.66153840231349E-16));
#45630=DIRECTION('ref_axis',(-0.999796975042654,3.77446942541727E-16,0.0201496574551479));
#45631=DIRECTION('',(3.66113466765123E-16,1.,-5.66153840231349E-16));
#45632=DIRECTION('center_axis',(3.66113466765123E-16,1.,-5.66153840231349E-16));
#45633=DIRECTION('ref_axis',(-0.469351874736002,-3.28084152151318E-16,-0.883011221719068));
#45634=DIRECTION('center_axis',(-3.66113466765123E-16,-1.,5.66153840231349E-16));
#45635=DIRECTION('ref_axis',(-0.469351874736002,-3.28084152151318E-16,-0.883011221719068));
#45636=DIRECTION('',(-3.66113466765123E-16,-1.,5.66153840231349E-16));
#45637=DIRECTION('center_axis',(3.66113466765123E-16,1.,-5.66153840231349E-16));
#45638=DIRECTION('ref_axis',(-0.268243314830189,6.43612468217339E-16,0.963351194554152));
#45639=DIRECTION('',(3.66113466765123E-16,1.,-5.66153840231349E-16));
#45640=DIRECTION('center_axis',(-3.66113466765123E-16,-1.,5.66153840231349E-16));
#45641=DIRECTION('ref_axis',(-0.268243314830189,6.43612468217339E-16,0.963351194554152));
#45642=DIRECTION('center_axis',(3.66113466765123E-16,1.,-5.66153840231349E-16));
#45643=DIRECTION('ref_axis',(-0.984335714327177,4.60193909783388E-16,0.176304286675074));
#45644=DIRECTION('',(3.66113466765123E-16,1.,-5.66153840231349E-16));
#45645=DIRECTION('center_axis',(-3.66113466765123E-16,-1.,5.66153840231349E-16));
#45646=DIRECTION('ref_axis',(-0.984335714327177,4.60193909783388E-16,0.176304286675074));
#45647=DIRECTION('',(3.66113466765123E-16,1.,-5.66153840231349E-16));
#45648=DIRECTION('center_axis',(3.66113466765123E-16,1.,-5.66153840231349E-16));
#45649=DIRECTION('ref_axis',(-0.601706762407361,-2.31903792697734E-16,-0.798717078866636));
#45650=DIRECTION('center_axis',(-3.66113466765123E-16,-1.,5.66153840231349E-16));
#45651=DIRECTION('ref_axis',(-0.601706762407361,-2.31903792697734E-16,-0.798717078866636));
#45652=DIRECTION('',(-3.66113466765123E-16,-1.,5.66153840231349E-16));
#45653=DIRECTION('center_axis',(3.66113466765123E-16,1.,-5.66153840231349E-16));
#45654=DIRECTION('ref_axis',(-0.114239465734422,6.04271975012079E-16,0.993453242215613));
#45655=DIRECTION('',(3.66113466765123E-16,1.,-5.66153840231349E-16));
#45656=DIRECTION('center_axis',(-3.66113466765123E-16,-1.,5.66153840231349E-16));
#45657=DIRECTION('ref_axis',(-0.114239465734422,6.04271975012079E-16,0.993453242215613));
#45658=DIRECTION('center_axis',(3.66113466765123E-16,1.,-5.66153840231349E-16));
#45659=DIRECTION('ref_axis',(-0.944636841502024,5.31609375670159E-16,0.328117719236679));
#45660=DIRECTION('',(3.66113466765123E-16,1.,-5.66153840231349E-16));
#45661=DIRECTION('center_axis',(-3.66113466765123E-16,-1.,5.66153840231349E-16));
#45662=DIRECTION('ref_axis',(-0.944636841502024,5.31609375670159E-16,0.328117719236679));
#45663=DIRECTION('',(3.66113466765123E-16,1.,-5.66153840231349E-16));
#45664=DIRECTION('center_axis',(3.66113466765123E-16,1.,-5.66153840231349E-16));
#45665=DIRECTION('ref_axis',(-0.719245632637998,-1.30013192223369E-16,-0.694755870742498));
#45666=DIRECTION('center_axis',(-3.66113466765123E-16,-1.,5.66153840231349E-16));
#45667=DIRECTION('ref_axis',(-0.719245632637998,-1.30013192223369E-16,-0.694755870742498));
#45668=DIRECTION('',(-3.66113466765123E-16,-1.,5.66153840231349E-16));
#45669=DIRECTION('center_axis',(3.66113466765123E-16,1.,-5.66153840231349E-16));
#45670=DIRECTION('ref_axis',(0.0425773381467764,5.50052300318313E-16,0.999093173971444));
#45671=DIRECTION('',(3.66113466765123E-16,1.,-5.66153840231349E-16));
#45672=DIRECTION('center_axis',(-3.66113466765123E-16,-1.,5.66153840231349E-16));
#45673=DIRECTION('ref_axis',(0.0425773381467764,5.50052300318313E-16,0.999093173971444));
#45674=DIRECTION('center_axis',(3.66113466765123E-16,1.,-5.66153840231349E-16));
#45675=DIRECTION('ref_axis',(-0.881677874569156,5.89934854417565E-16,0.471851804590399));
#45676=DIRECTION('',(3.66113466765123E-16,1.,-5.66153840231349E-16));
#45677=DIRECTION('center_axis',(-3.66113466765123E-16,-1.,5.66153840231349E-16));
#45678=DIRECTION('ref_axis',(-0.881677874569156,5.89934854417565E-16,0.471851804590399));
#45679=DIRECTION('',(3.66113466765123E-16,1.,-5.66153840231349E-16));
#45680=DIRECTION('center_axis',(3.66113466765123E-16,1.,-5.66153840231349E-16));
#45681=DIRECTION('ref_axis',(-0.819074288353686,-2.49212354674179E-17,-0.573687467318141));
#45682=DIRECTION('center_axis',(-3.66113466765123E-16,-1.,5.66153840231349E-16));
#45683=DIRECTION('ref_axis',(-0.819074288353686,-2.49212354674179E-17,-0.573687467318141));
#45684=DIRECTION('',(-3.66113466765123E-16,-1.,5.66153840231349E-16));
#45685=DIRECTION('center_axis',(3.66113466765123E-16,1.,-5.66153840231349E-16));
#45686=DIRECTION('ref_axis',(0.198345746656716,4.82288512471788E-16,0.980132115983957));
#45687=DIRECTION('',(3.66113466765123E-16,1.,-5.66153840231349E-16));
#45688=DIRECTION('center_axis',(-3.66113466765123E-16,-1.,5.66153840231349E-16));
#45689=DIRECTION('ref_axis',(0.198345746656716,4.82288512471788E-16,0.980132115983957));
#45690=DIRECTION('center_axis',(3.66113466765123E-16,1.,-5.66153840231349E-16));
#45691=DIRECTION('ref_axis',(-0.797009072243291,6.33734179167679E-16,0.603967332528746));
#45692=DIRECTION('',(3.66113466765123E-16,1.,-5.66153840231349E-16));
#45693=DIRECTION('center_axis',(-3.66113466765123E-16,-1.,5.66153840231349E-16));
#45694=DIRECTION('ref_axis',(-0.797009072243291,6.33734179167679E-16,0.603967332528746));
#45695=DIRECTION('',(3.66113466765123E-16,1.,-5.66153840231349E-16));
#45696=DIRECTION('center_axis',(3.66113466765123E-16,1.,-5.66153840231349E-16));
#45697=DIRECTION('ref_axis',(-0.898734616738394,8.07843648145798E-17,-0.438492974488865));
#45698=DIRECTION('center_axis',(-3.66113466765123E-16,-1.,5.66153840231349E-16));
#45699=DIRECTION('ref_axis',(-0.898734616738394,8.07843648145798E-17,-0.438492974488865));
#45700=DIRECTION('',(-3.66113466765123E-16,-1.,5.66153840231349E-16));
#45701=DIRECTION('center_axis',(3.66113466765123E-16,1.,-5.66153840231349E-16));
#45702=DIRECTION('ref_axis',(0.349230224612176,4.02649180824402E-16,0.937036952428947));
#45703=DIRECTION('',(3.66113466765123E-16,1.,-5.66153840231349E-16));
#45704=DIRECTION('center_axis',(-3.66113466765123E-16,-1.,5.66153840231349E-16));
#45705=DIRECTION('ref_axis',(0.349230224612176,4.02649180824402E-16,0.937036952428947));
#45706=DIRECTION('center_axis',(3.66113466765123E-16,1.,-5.66153840231349E-16));
#45707=DIRECTION('ref_axis',(-0.692715261437337,6.61928865183528E-16,0.721211180287579));
#45708=DIRECTION('',(3.66113466765123E-16,1.,-5.66153840231349E-16));
#45709=DIRECTION('center_axis',(-3.66113466765123E-16,-1.,5.66153840231349E-16));
#45710=DIRECTION('ref_axis',(-0.692715261437337,6.61928865183528E-16,0.721211180287579));
#45711=DIRECTION('',(3.66113466765123E-16,1.,-5.66153840231349E-16));
#45712=DIRECTION('center_axis',(3.66113466765123E-16,1.,-5.66153840231349E-16));
#45713=DIRECTION('ref_axis',(-0.956265116129817,1.84500785926907E-16,-0.292501329352925));
#45714=DIRECTION('center_axis',(-3.66113466765123E-16,-1.,5.66153840231349E-16));
#45715=DIRECTION('ref_axis',(-0.956265116129817,1.84500785926907E-16,-0.292501329352925));
#45716=DIRECTION('',(-3.66113466765123E-16,-1.,5.66153840231349E-16));
#45717=DIRECTION('center_axis',(3.66113466765123E-16,1.,-5.66153840231349E-16));
#45718=DIRECTION('ref_axis',(0.491515495409017,3.13095290029103E-16,0.870868829257787));
#45719=DIRECTION('',(3.66113466765123E-16,1.,-5.66153840231349E-16));
#45720=DIRECTION('center_axis',(-3.66113466765123E-16,-1.,5.66153840231349E-16));
#45721=DIRECTION('ref_axis',(0.491515495409017,3.13095290029103E-16,0.870868829257787));
#45722=DIRECTION('center_axis',(3.66113466765123E-16,1.,-5.66153840231349E-16));
#45723=DIRECTION('ref_axis',(-0.571364501904649,6.73824665722604E-16,0.820696415225053));
#45724=DIRECTION('',(3.66113466765123E-16,1.,-5.66153840231349E-16));
#45725=DIRECTION('center_axis',(-3.66113466765123E-16,-1.,5.66153840231349E-16));
#45726=DIRECTION('ref_axis',(-0.571364501904649,6.73824665722604E-16,0.820696415225053));
#45727=DIRECTION('',(3.66113466765123E-16,1.,-5.66153840231349E-16));
#45728=DIRECTION('center_axis',(3.66113466765123E-16,1.,-5.66153840231349E-16));
#45729=DIRECTION('ref_axis',(-0.990249194700156,2.83674185366711E-16,-0.13930733073206));
#45730=DIRECTION('center_axis',(-3.66113466765123E-16,-1.,5.66153840231349E-16));
#45731=DIRECTION('ref_axis',(-0.990249194700156,2.83674185366711E-16,-0.13930733073206));
#45732=DIRECTION('',(-3.66113466765123E-16,-1.,5.66153840231349E-16));
#45733=DIRECTION('center_axis',(3.66113466765123E-16,1.,-5.66153840231349E-16));
#45734=DIRECTION('ref_axis',(0.621698023462484,2.15831954089593E-16,0.78325702526236));
#45735=DIRECTION('',(3.66113466765123E-16,1.,-5.66153840231349E-16));
#45736=DIRECTION('center_axis',(-3.66113466765123E-16,-1.,5.66153840231349E-16));
#45737=DIRECTION('ref_axis',(0.621698023462484,2.15831954089593E-16,0.78325702526236));
#45738=DIRECTION('center_axis',(3.66113466765123E-16,1.,-5.66153840231349E-16));
#45739=DIRECTION('ref_axis',(-0.435944852085004,6.69128666695736E-16,0.899973380684442));
#45740=DIRECTION('',(3.66113466765123E-16,1.,-5.66153840231349E-16));
#45741=DIRECTION('center_axis',(-3.66113466765123E-16,-1.,5.66153840231349E-16));
#45742=DIRECTION('ref_axis',(-0.435944852085004,6.69128666695736E-16,0.899973380684442));
#45743=DIRECTION('',(3.66113466765123E-16,1.,-5.66153840231349E-16));
#45744=DIRECTION('center_axis',(3.66113466765123E-16,1.,-5.66153840231349E-16));
#45745=DIRECTION('ref_axis',(-0.999850051648321,3.75862584902141E-16,0.0173168767059515));
#45746=DIRECTION('center_axis',(-3.66113466765123E-16,-1.,5.66153840231349E-16));
#45747=DIRECTION('ref_axis',(-0.999850051648321,3.75862584902141E-16,0.0173168767059515));
#45748=DIRECTION('',(-3.66113466765123E-16,-1.,5.66153840231349E-16));
#45749=DIRECTION('center_axis',(3.66113466765123E-16,1.,-5.66153840231349E-16));
#45750=DIRECTION('ref_axis',(0.736572282880858,1.1325411913521E-16,0.676358833823941));
#45751=DIRECTION('',(3.66113466765123E-16,1.,-5.66153840231349E-16));
#45752=DIRECTION('center_axis',(-3.66113466765123E-16,-1.,5.66153840231349E-16));
#45753=DIRECTION('ref_axis',(0.736572282880858,1.1325411913521E-16,0.676358833823941));
#45754=DIRECTION('center_axis',(3.66113466765123E-16,1.,-5.66153840231349E-16));
#45755=DIRECTION('ref_axis',(-0.289790793189011,6.47956499184093E-16,0.957090014670973));
#45756=DIRECTION('',(3.66113466765123E-16,1.,-5.66153840231349E-16));
#45757=DIRECTION('center_axis',(-3.66113466765123E-16,-1.,5.66153840231349E-16));
#45758=DIRECTION('ref_axis',(-0.289790793189011,6.47956499184093E-16,0.957090014670973));
#45759=DIRECTION('',(3.66113466765123E-16,1.,-5.66153840231349E-16));
#45760=DIRECTION('center_axis',(3.66113466765123E-16,1.,-5.66153840231349E-16));
#45761=DIRECTION('ref_axis',(-0.98483128201283,4.5879600018088E-16,0.173514685168044));
#45762=DIRECTION('center_axis',(-3.66113466765123E-16,-1.,5.66153840231349E-16));
#45763=DIRECTION('ref_axis',(-0.98483128201283,4.5879600018088E-16,0.173514685168044));
#45764=DIRECTION('',(-3.66113466765123E-16,-1.,5.66153840231349E-16));
#45765=DIRECTION('center_axis',(3.66113466765123E-16,1.,-5.66153840231349E-16));
#45766=DIRECTION('ref_axis',(0.833309688151449,7.88759189884587E-18,0.552806443190503));
#45767=DIRECTION('',(3.66113466765123E-16,1.,-5.66153840231349E-16));
#45768=DIRECTION('center_axis',(-3.66113466765123E-16,-1.,5.66153840231349E-16));
#45769=DIRECTION('ref_axis',(0.833309688151449,7.88759189884587E-18,0.552806443190503));
#45770=DIRECTION('center_axis',(3.66113466765123E-16,1.,-5.66153840231349E-16));
#45771=DIRECTION('ref_axis',(-0.136501123204203,6.10829492218208E-16,0.990639916096657));
#45772=DIRECTION('',(3.66113466765123E-16,1.,-5.66153840231349E-16));
#45773=DIRECTION('center_axis',(-3.66113466765123E-16,-1.,5.66153840231349E-16));
#45774=DIRECTION('ref_axis',(-0.136501123204203,6.10829492218208E-16,0.990639916096657));
#45775=DIRECTION('',(3.66113466765123E-16,1.,-5.66153840231349E-16));
#45776=DIRECTION('center_axis',(3.66113466765123E-16,1.,-5.66153840231349E-16));
#45777=DIRECTION('ref_axis',(-0.945562697746547,5.30432335278537E-16,0.325439986219075));
#45778=DIRECTION('center_axis',(-3.66113466765123E-16,-1.,5.66153840231349E-16));
#45779=DIRECTION('ref_axis',(-0.945562697746547,5.30432335278537E-16,0.325439986219075));
#45780=DIRECTION('',(-3.66113466765123E-16,-1.,5.66153840231349E-16));
#45781=DIRECTION('center_axis',(3.66113466765123E-16,1.,-5.66153840231349E-16));
#45782=DIRECTION('ref_axis',(0.909528243303456,-9.76731540274849E-17,0.415642123266314));
#45783=DIRECTION('',(3.66113466765123E-16,1.,-5.66153840231349E-16));
#45784=DIRECTION('center_axis',(-3.66113466765123E-16,-1.,5.66153840231349E-16));
#45785=DIRECTION('ref_axis',(0.909528243303456,-9.76731540274849E-17,0.415642123266314));
#45786=DIRECTION('center_axis',(3.66113466765123E-16,1.,-5.66153840231349E-16));
#45787=DIRECTION('ref_axis',(0.0201496574551478,5.58661835927051E-16,0.999796975042654));
#45788=DIRECTION('',(3.66113466765123E-16,1.,-5.66153840231349E-16));
#45789=DIRECTION('center_axis',(-3.66113466765123E-16,-1.,5.66153840231349E-16));
#45790=DIRECTION('ref_axis',(0.0201496574551478,5.58661835927051E-16,0.999796975042654));
#45791=DIRECTION('',(3.66113466765123E-16,1.,-5.66153840231349E-16));
#45792=DIRECTION('center_axis',(3.66113466765123E-16,1.,-5.66153840231349E-16));
#45793=DIRECTION('ref_axis',(-0.883011221719068,5.89007665877645E-16,0.469351874736002));
#45794=DIRECTION('center_axis',(-3.66113466765123E-16,-1.,5.66153840231349E-16));
#45795=DIRECTION('ref_axis',(-0.883011221719068,5.89007665877645E-16,0.469351874736002));
#45796=DIRECTION('',(-3.66113466765123E-16,-1.,5.66153840231349E-16));
#45797=DIRECTION('center_axis',(3.66113466765123E-16,1.,-5.66153840231349E-16));
#45798=DIRECTION('ref_axis',(0.963351194554152,-2.00828862743045E-16,0.268243314830189));
#45799=DIRECTION('',(3.66113466765123E-16,1.,-5.66153840231349E-16));
#45800=DIRECTION('center_axis',(-3.66113466765123E-16,-1.,5.66153840231349E-16));
#45801=DIRECTION('ref_axis',(0.963351194554152,-2.00828862743045E-16,0.268243314830189));
#45802=DIRECTION('center_axis',(3.66113466765123E-16,1.,-5.66153840231349E-16));
#45803=DIRECTION('ref_axis',(0.176304286675074,4.92738071143036E-16,0.984335714327177));
#45804=DIRECTION('',(3.66113466765123E-16,1.,-5.66153840231349E-16));
#45805=DIRECTION('center_axis',(-3.66113466765123E-16,-1.,5.66153840231349E-16));
#45806=DIRECTION('ref_axis',(0.176304286675074,4.92738071143036E-16,0.984335714327177));
#45807=DIRECTION('',(3.66113466765123E-16,1.,-5.66153840231349E-16));
#45808=DIRECTION('center_axis',(3.66113466765123E-16,1.,-5.66153840231349E-16));
#45809=DIRECTION('ref_axis',(-0.798717078866636,6.33079672938476E-16,0.601706762407361));
#45810=DIRECTION('center_axis',(-3.66113466765123E-16,-1.,5.66153840231349E-16));
#45811=DIRECTION('ref_axis',(-0.798717078866636,6.33079672938476E-16,0.601706762407361));
#45812=DIRECTION('',(-3.66113466765123E-16,-1.,5.66153840231349E-16));
#45813=DIRECTION('center_axis',(3.66113466765123E-16,1.,-5.66153840231349E-16));
#45814=DIRECTION('ref_axis',(0.993453242215613,-2.99039498345089E-16,0.114239465734422));
#45815=DIRECTION('',(3.66113466765123E-16,1.,-5.66153840231349E-16));
#45816=DIRECTION('center_axis',(-3.66113466765123E-16,-1.,5.66153840231349E-16));
#45817=DIRECTION('ref_axis',(0.993453242215613,-2.99039498345089E-16,0.114239465734422));
#45818=DIRECTION('center_axis',(3.66113466765123E-16,1.,-5.66153840231349E-16));
#45819=DIRECTION('ref_axis',(0.328117719236679,4.14681459743577E-16,0.944636841502024));
#45820=DIRECTION('',(3.66113466765123E-16,1.,-5.66153840231349E-16));
#45821=DIRECTION('center_axis',(-3.66113466765123E-16,-1.,5.66153840231349E-16));
#45822=DIRECTION('ref_axis',(0.328117719236679,4.14681459743577E-16,0.944636841502024));
#45823=DIRECTION('',(3.66113466765123E-16,1.,-5.66153840231349E-16));
#45824=DIRECTION('center_axis',(3.66113466765123E-16,1.,-5.66153840231349E-16));
#45825=DIRECTION('ref_axis',(-0.694755870742498,6.61563157380586E-16,0.719245632637998));
#45826=DIRECTION('center_axis',(-3.66113466765123E-16,-1.,5.66153840231349E-16));
#45827=DIRECTION('ref_axis',(-0.694755870742498,6.61563157380586E-16,0.719245632637998));
#45828=DIRECTION('',(-3.66113466765123E-16,-1.,5.66153840231349E-16));
#45829=DIRECTION('center_axis',(3.66113466765123E-16,1.,-5.66153840231349E-16));
#45830=DIRECTION('ref_axis',(0.999093173971444,-3.89886789042682E-16,-0.0425773381467764));
#45831=DIRECTION('',(3.66113466765123E-16,1.,-5.66153840231349E-16));
#45832=DIRECTION('center_axis',(-3.66113466765123E-16,-1.,5.66153840231349E-16));
#45833=DIRECTION('ref_axis',(0.999093173971444,-3.89886789042682E-16,-0.0425773381467764));
#45834=DIRECTION('center_axis',(3.66113466765123E-16,1.,-5.66153840231349E-16));
#45835=DIRECTION('ref_axis',(0.471851804590399,3.26414014556371E-16,0.881677874569156));
#45836=DIRECTION('',(3.66113466765123E-16,1.,-5.66153840231349E-16));
#45837=DIRECTION('center_axis',(-3.66113466765123E-16,-1.,5.66153840231349E-16));
#45838=DIRECTION('ref_axis',(0.471851804590399,3.26414014556371E-16,0.881677874569156));
#45839=DIRECTION('',(3.66113466765123E-16,1.,-5.66153840231349E-16));
#45840=DIRECTION('center_axis',(3.66113466765123E-16,1.,-5.66153840231349E-16));
#45841=DIRECTION('ref_axis',(-0.573687467318141,6.73756761285746E-16,0.819074288353686));
#45842=DIRECTION('center_axis',(-3.66113466765123E-16,-1.,5.66153840231349E-16));
#45843=DIRECTION('ref_axis',(-0.573687467318141,6.73756761285746E-16,0.819074288353686));
#45844=DIRECTION('',(-3.66113466765123E-16,-1.,5.66153840231349E-16));
#45845=DIRECTION('center_axis',(3.66113466765123E-16,1.,-5.66153840231349E-16));
#45846=DIRECTION('ref_axis',(0.980132115983957,-4.71133773033976E-16,-0.198345746656716));
#45847=DIRECTION('',(3.66113466765123E-16,1.,-5.66153840231349E-16));
#45848=DIRECTION('center_axis',(-3.66113466765123E-16,-1.,5.66153840231349E-16));
#45849=DIRECTION('ref_axis',(0.980132115983957,-4.71133773033976E-16,-0.198345746656716));
#45850=DIRECTION('center_axis',(3.66113466765123E-16,1.,-5.66153840231349E-16));
#45851=DIRECTION('ref_axis',(0.603967332528746,2.30109173024781E-16,0.797009072243291));
#45852=DIRECTION('',(3.66113466765123E-16,1.,-5.66153840231349E-16));
#45853=DIRECTION('center_axis',(-3.66113466765123E-16,-1.,5.66153840231349E-16));
#45854=DIRECTION('ref_axis',(0.603967332528746,2.30109173024781E-16,0.797009072243291));
#45855=DIRECTION('',(3.66113466765123E-16,1.,-5.66153840231349E-16));
#45856=DIRECTION('center_axis',(3.66113466765123E-16,1.,-5.66153840231349E-16));
#45857=DIRECTION('ref_axis',(-0.438492974488865,6.6936023765756E-16,0.898734616738394));
#45858=DIRECTION('center_axis',(-3.66113466765123E-16,-1.,5.66153840231349E-16));
#45859=DIRECTION('ref_axis',(-0.438492974488865,6.6936023765756E-16,0.898734616738394));
#45860=DIRECTION('',(-3.66113466765123E-16,-1.,5.66153840231349E-16));
#45861=DIRECTION('center_axis',(3.66113466765123E-16,1.,-5.66153840231349E-16));
#45862=DIRECTION('ref_axis',(0.937036952428947,-5.40779879929828E-16,-0.349230224612176));
#45863=DIRECTION('',(3.66113466765123E-16,1.,-5.66153840231349E-16));
#45864=DIRECTION('center_axis',(-3.66113466765123E-16,-1.,5.66153840231349E-16));
#45865=DIRECTION('ref_axis',(0.937036952428947,-5.40779879929828E-16,-0.349230224612176));
#45866=DIRECTION('center_axis',(3.66113466765123E-16,1.,-5.66153840231349E-16));
#45867=DIRECTION('ref_axis',(0.721211180287579,1.2813827996476E-16,0.692715261437337));
#45868=DIRECTION('',(3.66113466765123E-16,1.,-5.66153840231349E-16));
#45869=DIRECTION('center_axis',(-3.66113466765123E-16,-1.,5.66153840231349E-16));
#45870=DIRECTION('ref_axis',(0.721211180287579,1.2813827996476E-16,0.692715261437337));
#45871=DIRECTION('',(3.66113466765123E-16,1.,-5.66153840231349E-16));
#45872=DIRECTION('center_axis',(3.66113466765123E-16,1.,-5.66153840231349E-16));
#45873=DIRECTION('ref_axis',(-0.292501329352925,6.48481843498979E-16,0.956265116129817));
#45874=DIRECTION('center_axis',(-3.66113466765123E-16,-1.,5.66153840231349E-16));
#45875=DIRECTION('ref_axis',(-0.292501329352925,6.48481843498979E-16,0.956265116129817));
#45876=DIRECTION('',(-3.66113466765123E-16,-1.,5.66153840231349E-16));
#45877=DIRECTION('center_axis',(3.66113466765123E-16,1.,-5.66153840231349E-16));
#45878=DIRECTION('ref_axis',(0.870868829257786,-5.97110191436282E-16,-0.491515495409018));
#45879=DIRECTION('',(3.66113466765123E-16,1.,-5.66153840231349E-16));
#45880=DIRECTION('center_axis',(-3.66113466765123E-16,-1.,5.66153840231349E-16));
#45881=DIRECTION('ref_axis',(0.870868829257786,-5.97110191436282E-16,-0.491515495409018));
#45882=DIRECTION('center_axis',(3.66113466765123E-16,1.,-5.66153840231349E-16));
#45883=DIRECTION('ref_axis',(0.820696415225053,2.30121971854362E-17,0.571364501904649));
#45884=DIRECTION('',(3.66113466765123E-16,1.,-5.66153840231349E-16));
#45885=DIRECTION('center_axis',(-3.66113466765123E-16,-1.,5.66153840231349E-16));
#45886=DIRECTION('ref_axis',(0.820696415225053,2.30121971854362E-17,0.571364501904649));
#45887=DIRECTION('',(3.66113466765123E-16,1.,-5.66153840231349E-16));
#45888=DIRECTION('center_axis',(3.66113466765123E-16,1.,-5.66153840231349E-16));
#45889=DIRECTION('ref_axis',(-0.13930733073206,6.11635674165605E-16,0.990249194700156));
#45890=DIRECTION('center_axis',(-3.66113466765123E-16,-1.,5.66153840231349E-16));
#45891=DIRECTION('ref_axis',(-0.13930733073206,6.11635674165605E-16,0.990249194700156));
#45892=DIRECTION('',(-3.66113466765123E-16,-1.,5.66153840231349E-16));
#45893=DIRECTION('center_axis',(3.66113466765123E-16,1.,-5.66153840231349E-16));
#45894=DIRECTION('ref_axis',(0.78325702526236,-6.38737668334465E-16,-0.621698023462484));
#45895=DIRECTION('',(3.66113466765123E-16,1.,-5.66153840231349E-16));
#45896=DIRECTION('center_axis',(-3.66113466765123E-16,-1.,5.66153840231349E-16));
#45897=DIRECTION('ref_axis',(0.78325702526236,-6.38737668334465E-16,-0.621698023462484));
#45898=DIRECTION('center_axis',(3.66113466765123E-16,1.,-5.66153840231349E-16));
#45899=DIRECTION('ref_axis',(0.899973380684442,-8.26805222616965E-17,0.435944852085004));
#45900=DIRECTION('',(3.66113466765123E-16,1.,-5.66153840231349E-16));
#45901=DIRECTION('center_axis',(-3.66113466765123E-16,-1.,5.66153840231349E-16));
#45902=DIRECTION('ref_axis',(0.899973380684442,-8.26805222616965E-17,0.435944852085004));
#45903=DIRECTION('',(3.66113466765123E-16,1.,-5.66153840231349E-16));
#45904=DIRECTION('center_axis',(3.66113466765123E-16,1.,-5.66153840231349E-16));
#45905=DIRECTION('ref_axis',(0.0173168767059515,5.5972900463185E-16,0.999850051648321));
#45906=DIRECTION('center_axis',(-3.66113466765123E-16,-1.,5.66153840231349E-16));
#45907=DIRECTION('ref_axis',(0.0173168767059515,5.5972900463185E-16,0.999850051648321));
#45908=DIRECTION('',(-3.66113466765123E-16,-1.,5.66153840231349E-16));
#45909=DIRECTION('center_axis',(3.66113466765123E-16,1.,-5.66153840231349E-16));
#45910=DIRECTION('ref_axis',(0.676358833823941,-6.64637303989468E-16,-0.736572282880858));
#45911=DIRECTION('',(3.66113466765123E-16,1.,-5.66153840231349E-16));
#45912=DIRECTION('center_axis',(-3.66113466765123E-16,-1.,5.66153840231349E-16));
#45913=DIRECTION('ref_axis',(0.676358833823941,-6.64637303989468E-16,-0.736572282880858));
#45914=DIRECTION('center_axis',(3.66113466765123E-16,1.,-5.66153840231349E-16));
#45915=DIRECTION('ref_axis',(0.957090014670973,-1.86337372849825E-16,0.289790793189011));
#45916=DIRECTION('',(3.66113466765123E-16,1.,-5.66153840231349E-16));
#45917=DIRECTION('center_axis',(-3.66113466765123E-16,-1.,5.66153840231349E-16));
#45918=DIRECTION('ref_axis',(0.957090014670973,-1.86337372849825E-16,0.289790793189011));
#45919=DIRECTION('',(3.66113466765123E-16,1.,-5.66153840231349E-16));
#45920=DIRECTION('center_axis',(3.66113466765123E-16,1.,-5.66153840231349E-16));
#45921=DIRECTION('ref_axis',(0.173514685168044,4.94039949369995E-16,0.98483128201283));
#45922=DIRECTION('center_axis',(-3.66113466765123E-16,-1.,5.66153840231349E-16));
#45923=DIRECTION('ref_axis',(0.173514685168044,4.94039949369995E-16,0.98483128201283));
#45924=DIRECTION('',(-3.66113466765123E-16,-1.,5.66153840231349E-16));
#45925=DIRECTION('center_axis',(3.66113466765123E-16,1.,-5.66153840231349E-16));
#45926=DIRECTION('ref_axis',(0.552806443190503,-6.74171363415503E-16,-0.833309688151449));
#45927=DIRECTION('',(3.66113466765123E-16,1.,-5.66153840231349E-16));
#45928=DIRECTION('center_axis',(-3.66113466765123E-16,-1.,5.66153840231349E-16));
#45929=DIRECTION('ref_axis',(0.552806443190503,-6.74171363415503E-16,-0.833309688151449));
#45930=DIRECTION('center_axis',(3.66113466765123E-16,1.,-5.66153840231349E-16));
#45931=DIRECTION('ref_axis',(0.990639916096657,-2.85405978900105E-16,0.136501123204203));
#45932=DIRECTION('',(3.66113466765123E-16,1.,-5.66153840231349E-16));
#45933=DIRECTION('center_axis',(-3.66113466765123E-16,-1.,5.66153840231349E-16));
#45934=DIRECTION('ref_axis',(0.990639916096657,-2.85405978900105E-16,0.136501123204203));
#45935=DIRECTION('',(3.66113466765123E-16,1.,-5.66153840231349E-16));
#45936=DIRECTION('center_axis',(3.66113466765123E-16,1.,-5.66153840231349E-16));
#45937=DIRECTION('ref_axis',(0.325439986219075,4.16185990930063E-16,0.945562697746547));
#45938=DIRECTION('center_axis',(-3.66113466765123E-16,-1.,5.66153840231349E-16));
#45939=DIRECTION('ref_axis',(0.325439986219075,4.16185990930063E-16,0.945562697746547));
#45940=DIRECTION('',(-3.66113466765123E-16,-1.,5.66153840231349E-16));
#45941=DIRECTION('center_axis',(3.66113466765123E-16,1.,-5.66153840231349E-16));
#45942=DIRECTION('ref_axis',(0.415642123266314,-6.67105086427771E-16,-0.909528243303456));
#45943=DIRECTION('',(3.66113466765123E-16,1.,-5.66153840231349E-16));
#45944=DIRECTION('center_axis',(-3.66113466765123E-16,-1.,5.66153840231349E-16));
#45945=DIRECTION('ref_axis',(0.415642123266314,-6.67105086427771E-16,-0.909528243303456));
#45946=DIRECTION('center_axis',(3.66113466765123E-16,1.,-5.66153840231349E-16));
#45947=DIRECTION('ref_axis',(0.999796975042654,-3.77446942541727E-16,-0.0201496574551476));
#45948=DIRECTION('',(3.66113466765123E-16,1.,-5.66153840231349E-16));
#45949=DIRECTION('center_axis',(-3.66113466765123E-16,-1.,5.66153840231349E-16));
#45950=DIRECTION('ref_axis',(0.999796975042654,-3.77446942541727E-16,-0.0201496574551476));
#45951=DIRECTION('',(3.66113466765123E-16,1.,-5.66153840231349E-16));
#45952=DIRECTION('center_axis',(3.66113466765123E-16,1.,-5.66153840231349E-16));
#45953=DIRECTION('ref_axis',(0.469351874736002,3.28084152151318E-16,0.883011221719068));
#45954=DIRECTION('center_axis',(-3.66113466765123E-16,-1.,5.66153840231349E-16));
#45955=DIRECTION('ref_axis',(0.469351874736002,3.28084152151318E-16,0.883011221719068));
#45956=DIRECTION('',(-3.66113466765123E-16,-1.,5.66153840231349E-16));
#45957=DIRECTION('center_axis',(3.66113466765123E-16,1.,-5.66153840231349E-16));
#45958=DIRECTION('ref_axis',(0.268243314830189,-6.43612468217339E-16,-0.963351194554152));
#45959=DIRECTION('',(3.66113466765123E-16,1.,-5.66153840231349E-16));
#45960=DIRECTION('center_axis',(-3.66113466765123E-16,-1.,5.66153840231349E-16));
#45961=DIRECTION('ref_axis',(0.268243314830189,-6.43612468217339E-16,-0.963351194554152));
#45962=DIRECTION('center_axis',(3.66113466765123E-16,1.,-5.66153840231349E-16));
#45963=DIRECTION('ref_axis',(0.984335714327177,-4.60193909783388E-16,-0.176304286675074));
#45964=DIRECTION('',(3.66113466765123E-16,1.,-5.66153840231349E-16));
#45965=DIRECTION('center_axis',(-3.66113466765123E-16,-1.,5.66153840231349E-16));
#45966=DIRECTION('ref_axis',(0.984335714327177,-4.60193909783388E-16,-0.176304286675074));
#45967=DIRECTION('',(3.66113466765123E-16,1.,-5.66153840231349E-16));
#45968=DIRECTION('center_axis',(3.66113466765123E-16,1.,-5.66153840231349E-16));
#45969=DIRECTION('ref_axis',(0.601706762407361,2.31903792697734E-16,0.798717078866636));
#45970=DIRECTION('center_axis',(-3.66113466765123E-16,-1.,5.66153840231349E-16));
#45971=DIRECTION('ref_axis',(0.601706762407361,2.31903792697734E-16,0.798717078866636));
#45972=DIRECTION('',(-3.66113466765123E-16,-1.,5.66153840231349E-16));
#45973=DIRECTION('center_axis',(3.66113466765123E-16,1.,-5.66153840231349E-16));
#45974=DIRECTION('ref_axis',(0.114239465734422,-6.04271975012079E-16,-0.993453242215613));
#45975=DIRECTION('',(3.66113466765123E-16,1.,-5.66153840231349E-16));
#45976=DIRECTION('center_axis',(-3.66113466765123E-16,-1.,5.66153840231349E-16));
#45977=DIRECTION('ref_axis',(0.114239465734422,-6.04271975012079E-16,-0.993453242215613));
#45978=DIRECTION('center_axis',(3.66113466765123E-16,1.,-5.66153840231349E-16));
#45979=DIRECTION('ref_axis',(0.944636841502024,-5.31609375670159E-16,-0.328117719236679));
#45980=DIRECTION('',(3.66113466765123E-16,1.,-5.66153840231349E-16));
#45981=DIRECTION('center_axis',(-3.66113466765123E-16,-1.,5.66153840231349E-16));
#45982=DIRECTION('ref_axis',(0.944636841502024,-5.31609375670159E-16,-0.328117719236679));
#45983=DIRECTION('',(3.66113466765123E-16,1.,-5.66153840231349E-16));
#45984=DIRECTION('center_axis',(3.66113466765123E-16,1.,-5.66153840231349E-16));
#45985=DIRECTION('ref_axis',(0.719245632637998,1.30013192223369E-16,0.694755870742498));
#45986=DIRECTION('center_axis',(-3.66113466765123E-16,-1.,5.66153840231349E-16));
#45987=DIRECTION('ref_axis',(0.719245632637998,1.30013192223369E-16,0.694755870742498));
#45988=DIRECTION('',(-3.66113466765123E-16,-1.,5.66153840231349E-16));
#45989=DIRECTION('center_axis',(3.66113466765123E-16,1.,-5.66153840231349E-16));
#45990=DIRECTION('ref_axis',(-0.0425773381467764,-5.50052300318313E-16,
-0.999093173971444));
#45991=DIRECTION('',(3.66113466765123E-16,1.,-5.66153840231349E-16));
#45992=DIRECTION('center_axis',(-3.66113466765123E-16,-1.,5.66153840231349E-16));
#45993=DIRECTION('ref_axis',(-0.0425773381467764,-5.50052300318313E-16,
-0.999093173971444));
#45994=DIRECTION('center_axis',(3.66113466765123E-16,1.,-5.66153840231349E-16));
#45995=DIRECTION('ref_axis',(0.881677874569156,-5.89934854417565E-16,-0.471851804590399));
#45996=DIRECTION('',(3.66113466765123E-16,1.,-5.66153840231349E-16));
#45997=DIRECTION('center_axis',(-3.66113466765123E-16,-1.,5.66153840231349E-16));
#45998=DIRECTION('ref_axis',(0.881677874569156,-5.89934854417565E-16,-0.471851804590399));
#45999=DIRECTION('',(3.66113466765123E-16,1.,-5.66153840231349E-16));
#46000=DIRECTION('center_axis',(3.66113466765123E-16,1.,-5.66153840231349E-16));
#46001=DIRECTION('ref_axis',(0.819074288353686,2.49212354674179E-17,0.573687467318141));
#46002=DIRECTION('center_axis',(-3.66113466765123E-16,-1.,5.66153840231349E-16));
#46003=DIRECTION('ref_axis',(0.819074288353686,2.49212354674179E-17,0.573687467318141));
#46004=DIRECTION('',(-3.66113466765123E-16,-1.,5.66153840231349E-16));
#46005=DIRECTION('center_axis',(3.66113466765123E-16,1.,-5.66153840231349E-16));
#46006=DIRECTION('ref_axis',(-0.198345746656716,-4.82288512471788E-16,-0.980132115983957));
#46007=DIRECTION('',(3.66113466765123E-16,1.,-5.66153840231349E-16));
#46008=DIRECTION('center_axis',(-3.66113466765123E-16,-1.,5.66153840231349E-16));
#46009=DIRECTION('ref_axis',(-0.198345746656716,-4.82288512471788E-16,-0.980132115983957));
#46010=DIRECTION('center_axis',(3.66113466765123E-16,1.,-5.66153840231349E-16));
#46011=DIRECTION('ref_axis',(0.797009072243291,-6.33734179167679E-16,-0.603967332528746));
#46012=DIRECTION('',(3.66113466765123E-16,1.,-5.66153840231349E-16));
#46013=DIRECTION('center_axis',(-3.66113466765123E-16,-1.,5.66153840231349E-16));
#46014=DIRECTION('ref_axis',(0.797009072243291,-6.33734179167679E-16,-0.603967332528746));
#46015=DIRECTION('',(3.66113466765123E-16,1.,-5.66153840231349E-16));
#46016=DIRECTION('center_axis',(3.66113466765123E-16,1.,-5.66153840231349E-16));
#46017=DIRECTION('ref_axis',(0.898734616738394,-8.07843648145798E-17,0.438492974488865));
#46018=DIRECTION('center_axis',(-3.66113466765123E-16,-1.,5.66153840231349E-16));
#46019=DIRECTION('ref_axis',(0.898734616738394,-8.07843648145798E-17,0.438492974488865));
#46020=DIRECTION('',(-3.66113466765123E-16,-1.,5.66153840231349E-16));
#46021=DIRECTION('center_axis',(3.66113466765123E-16,1.,-5.66153840231349E-16));
#46022=DIRECTION('ref_axis',(-0.349230224612176,-4.02649180824402E-16,-0.937036952428947));
#46023=DIRECTION('',(3.66113466765123E-16,1.,-5.66153840231349E-16));
#46024=DIRECTION('center_axis',(-3.66113466765123E-16,-1.,5.66153840231349E-16));
#46025=DIRECTION('ref_axis',(-0.349230224612176,-4.02649180824402E-16,-0.937036952428947));
#46026=DIRECTION('center_axis',(3.66113466765123E-16,1.,-5.66153840231349E-16));
#46027=DIRECTION('ref_axis',(0.692715261437337,-6.61928865183528E-16,-0.721211180287579));
#46028=DIRECTION('',(3.66113466765123E-16,1.,-5.66153840231349E-16));
#46029=DIRECTION('center_axis',(-3.66113466765123E-16,-1.,5.66153840231349E-16));
#46030=DIRECTION('ref_axis',(0.692715261437337,-6.61928865183528E-16,-0.721211180287579));
#46031=DIRECTION('',(3.66113466765123E-16,1.,-5.66153840231349E-16));
#46032=DIRECTION('center_axis',(3.66113466765123E-16,1.,-5.66153840231349E-16));
#46033=DIRECTION('ref_axis',(0.956265116129817,-1.84500785926907E-16,0.292501329352925));
#46034=DIRECTION('center_axis',(-3.66113466765123E-16,-1.,5.66153840231349E-16));
#46035=DIRECTION('ref_axis',(0.956265116129817,-1.84500785926907E-16,0.292501329352925));
#46036=DIRECTION('',(-3.66113466765123E-16,-1.,5.66153840231349E-16));
#46037=DIRECTION('center_axis',(3.66113466765123E-16,1.,-5.66153840231349E-16));
#46038=DIRECTION('ref_axis',(-0.491515495409017,-3.13095290029103E-16,-0.870868829257787));
#46039=DIRECTION('',(3.66113466765123E-16,1.,-5.66153840231349E-16));
#46040=DIRECTION('center_axis',(-3.66113466765123E-16,-1.,5.66153840231349E-16));
#46041=DIRECTION('ref_axis',(-0.491515495409017,-3.13095290029103E-16,-0.870868829257787));
#46042=DIRECTION('center_axis',(3.66113466765123E-16,1.,-5.66153840231349E-16));
#46043=DIRECTION('ref_axis',(0.571364501904649,-6.73824665722604E-16,-0.820696415225053));
#46044=DIRECTION('',(3.66113466765123E-16,1.,-5.66153840231349E-16));
#46045=DIRECTION('center_axis',(-3.66113466765123E-16,-1.,5.66153840231349E-16));
#46046=DIRECTION('ref_axis',(0.571364501904649,-6.73824665722604E-16,-0.820696415225053));
#46047=DIRECTION('',(3.66113466765123E-16,1.,-5.66153840231349E-16));
#46048=DIRECTION('center_axis',(3.66113466765123E-16,1.,-5.66153840231349E-16));
#46049=DIRECTION('ref_axis',(0.990249194700156,-2.83674185366711E-16,0.139307330732061));
#46050=DIRECTION('center_axis',(-3.66113466765123E-16,-1.,5.66153840231349E-16));
#46051=DIRECTION('ref_axis',(0.990249194700156,-2.83674185366711E-16,0.139307330732061));
#46052=DIRECTION('',(-3.66113466765123E-16,-1.,5.66153840231349E-16));
#46053=DIRECTION('center_axis',(3.66113466765123E-16,1.,-5.66153840231349E-16));
#46054=DIRECTION('ref_axis',(-0.621698023462484,-2.15831954089593E-16,-0.78325702526236));
#46055=DIRECTION('',(3.66113466765123E-16,1.,-5.66153840231349E-16));
#46056=DIRECTION('center_axis',(-3.66113466765123E-16,-1.,5.66153840231349E-16));
#46057=DIRECTION('ref_axis',(-0.621698023462484,-2.15831954089593E-16,-0.78325702526236));
#46058=DIRECTION('center_axis',(3.66113466765123E-16,1.,-5.66153840231349E-16));
#46059=DIRECTION('ref_axis',(0.435944852085004,-6.69128666695736E-16,-0.899973380684442));
#46060=DIRECTION('',(3.66113466765123E-16,1.,-5.66153840231349E-16));
#46061=DIRECTION('center_axis',(-3.66113466765123E-16,-1.,5.66153840231349E-16));
#46062=DIRECTION('ref_axis',(0.435944852085004,-6.69128666695736E-16,-0.899973380684442));
#46063=DIRECTION('',(3.66113466765123E-16,1.,-5.66153840231349E-16));
#46064=DIRECTION('center_axis',(3.66113466765123E-16,1.,-5.66153840231349E-16));
#46065=DIRECTION('ref_axis',(0.999850051648321,-3.75862584902141E-16,-0.0173168767059515));
#46066=DIRECTION('center_axis',(-3.66113466765123E-16,-1.,5.66153840231349E-16));
#46067=DIRECTION('ref_axis',(0.999850051648321,-3.75862584902141E-16,-0.0173168767059515));
#46068=DIRECTION('',(-3.66113466765123E-16,-1.,5.66153840231349E-16));
#46069=DIRECTION('center_axis',(3.66113466765123E-16,1.,-5.66153840231349E-16));
#46070=DIRECTION('ref_axis',(-0.736572282880858,-1.1325411913521E-16,-0.676358833823941));
#46071=DIRECTION('',(3.66113466765123E-16,1.,-5.66153840231349E-16));
#46072=DIRECTION('center_axis',(-3.66113466765123E-16,-1.,5.66153840231349E-16));
#46073=DIRECTION('ref_axis',(-0.736572282880858,-1.1325411913521E-16,-0.676358833823941));
#46074=DIRECTION('center_axis',(3.66113466765123E-16,1.,-5.66153840231349E-16));
#46075=DIRECTION('ref_axis',(0.289790793189011,-6.47956499184093E-16,-0.957090014670973));
#46076=DIRECTION('',(3.66113466765123E-16,1.,-5.66153840231349E-16));
#46077=DIRECTION('center_axis',(-3.66113466765123E-16,-1.,5.66153840231349E-16));
#46078=DIRECTION('ref_axis',(0.289790793189011,-6.47956499184093E-16,-0.957090014670973));
#46079=DIRECTION('',(3.66113466765123E-16,1.,-5.66153840231349E-16));
#46080=DIRECTION('center_axis',(3.66113466765123E-16,1.,-5.66153840231349E-16));
#46081=DIRECTION('ref_axis',(0.98483128201283,-4.5879600018088E-16,-0.173514685168044));
#46082=DIRECTION('center_axis',(-3.66113466765123E-16,-1.,5.66153840231349E-16));
#46083=DIRECTION('ref_axis',(0.98483128201283,-4.5879600018088E-16,-0.173514685168044));
#46084=DIRECTION('',(-3.66113466765123E-16,-1.,5.66153840231349E-16));
#46085=DIRECTION('center_axis',(3.66113466765123E-16,1.,-5.66153840231349E-16));
#46086=DIRECTION('ref_axis',(-0.833309688151449,-7.88759189884587E-18,-0.552806443190503));
#46087=DIRECTION('',(3.66113466765123E-16,1.,-5.66153840231349E-16));
#46088=DIRECTION('center_axis',(-3.66113466765123E-16,-1.,5.66153840231349E-16));
#46089=DIRECTION('ref_axis',(-0.833309688151449,-7.88759189884587E-18,-0.552806443190503));
#46090=DIRECTION('center_axis',(3.66113466765123E-16,1.,-5.66153840231349E-16));
#46091=DIRECTION('ref_axis',(0.136501123204203,-6.10829492218208E-16,-0.990639916096657));
#46092=DIRECTION('',(3.66113466765123E-16,1.,-5.66153840231349E-16));
#46093=DIRECTION('center_axis',(-3.66113466765123E-16,-1.,5.66153840231349E-16));
#46094=DIRECTION('ref_axis',(0.136501123204203,-6.10829492218208E-16,-0.990639916096657));
#46095=DIRECTION('',(3.66113466765123E-16,1.,-5.66153840231349E-16));
#46096=DIRECTION('center_axis',(3.66113466765123E-16,1.,-5.66153840231349E-16));
#46097=DIRECTION('ref_axis',(0.945562697746547,-5.30432335278537E-16,-0.325439986219075));
#46098=DIRECTION('center_axis',(-3.66113466765123E-16,-1.,5.66153840231349E-16));
#46099=DIRECTION('ref_axis',(0.945562697746547,-5.30432335278537E-16,-0.325439986219075));
#46100=DIRECTION('',(-3.66113466765123E-16,-1.,5.66153840231349E-16));
#46101=DIRECTION('center_axis',(3.66113466765123E-16,1.,-5.66153840231349E-16));
#46102=DIRECTION('ref_axis',(-0.909528243303456,9.76731540274849E-17,-0.415642123266314));
#46103=DIRECTION('',(3.66113466765123E-16,1.,-5.66153840231349E-16));
#46104=DIRECTION('center_axis',(-3.66113466765123E-16,-1.,5.66153840231349E-16));
#46105=DIRECTION('ref_axis',(-0.909528243303456,9.76731540274849E-17,-0.415642123266314));
#46106=DIRECTION('center_axis',(3.66113466765123E-16,1.,-5.66153840231349E-16));
#46107=DIRECTION('ref_axis',(-0.996957691137886,3.20870996777813E-16,-0.0779446090567869));
#46108=DIRECTION('center_axis',(-3.66113466765123E-16,-1.,5.66153840231349E-16));
#46109=DIRECTION('ref_axis',(-0.996957691137886,3.20870996777813E-16,-0.0779446090567869));
#46110=DIRECTION('',(3.66113466765123E-16,1.,-5.66153840231349E-16));
#46111=DIRECTION('center_axis',(3.66113466765123E-16,1.,-5.66153840231349E-16));
#46112=DIRECTION('ref_axis',(-0.996957691137886,3.20870996777813E-16,-0.0779446090567869));
#46113=DIRECTION('center_axis',(-3.66113466765123E-16,-1.,5.66153840231349E-16));
#46114=DIRECTION('ref_axis',(-0.996957691137886,3.20870996777813E-16,-0.0779446090567869));
#46115=DIRECTION('center_axis',(3.66113466765123E-16,1.,-5.66153840231349E-16));
#46116=DIRECTION('ref_axis',(-0.996957691137886,3.20870996777813E-16,-0.0779446090567869));
#46117=DIRECTION('center_axis',(-3.66113466765123E-16,-1.,5.66153840231349E-16));
#46118=DIRECTION('ref_axis',(-0.996957691137886,3.20870996777813E-16,-0.0779446090567869));
#46119=DIRECTION('center_axis',(3.66113466765123E-16,1.,-5.66153840231349E-16));
#46120=DIRECTION('ref_axis',(-0.996957691137886,3.20870996777813E-16,-0.0779446090567869));
#46121=DIRECTION('center_axis',(-3.66113466765123E-16,-1.,5.66153840231349E-16));
#46122=DIRECTION('ref_axis',(-0.996957691137886,3.20870996777813E-16,-0.0779446090567869));
#46123=DIRECTION('center_axis',(3.66113466765123E-16,1.,-5.66153840231349E-16));
#46124=DIRECTION('ref_axis',(-0.996957691137886,3.20870996777813E-16,-0.0779446090567869));
#46125=DIRECTION('center_axis',(-3.66113466765123E-16,-1.,5.66153840231349E-16));
#46126=DIRECTION('ref_axis',(-0.996957691137886,3.20870996777813E-16,-0.0779446090567869));
#46127=DIRECTION('center_axis',(3.66113466765123E-16,1.,-5.66153840231349E-16));
#46128=DIRECTION('ref_axis',(-0.996957691137886,3.20870996777813E-16,-0.0779446090567869));
#46129=DIRECTION('center_axis',(-3.66113466765123E-16,-1.,5.66153840231349E-16));
#46130=DIRECTION('ref_axis',(-0.996957691137886,3.20870996777813E-16,-0.0779446090567869));
#46131=DIRECTION('center_axis',(3.66113466765123E-16,1.,-5.66153840231349E-16));
#46132=DIRECTION('ref_axis',(-0.996957691137886,3.20870996777813E-16,-0.0779446090567869));
#46133=DIRECTION('center_axis',(-3.66113466765123E-16,-1.,5.66153840231349E-16));
#46134=DIRECTION('ref_axis',(-0.996957691137886,3.20870996777813E-16,-0.0779446090567869));
#46135=DIRECTION('center_axis',(3.66113466765123E-16,1.,-5.66153840231349E-16));
#46136=DIRECTION('ref_axis',(-0.996957691137886,3.20870996777813E-16,-0.0779446090567869));
#46137=DIRECTION('center_axis',(-3.66113466765123E-16,-1.,5.66153840231349E-16));
#46138=DIRECTION('ref_axis',(-0.996957691137886,3.20870996777813E-16,-0.0779446090567869));
#46139=DIRECTION('center_axis',(3.66113466765123E-16,1.,-5.66153840231349E-16));
#46140=DIRECTION('ref_axis',(-0.996957691137886,3.20870996777813E-16,-0.0779446090567869));
#46141=DIRECTION('center_axis',(-3.66113466765123E-16,-1.,5.66153840231349E-16));
#46142=DIRECTION('ref_axis',(-0.996957691137886,3.20870996777813E-16,-0.0779446090567869));
#46143=DIRECTION('center_axis',(3.66113466765123E-16,1.,-5.66153840231349E-16));
#46144=DIRECTION('ref_axis',(-0.996957691137886,3.20870996777813E-16,-0.0779446090567869));
#46145=DIRECTION('center_axis',(-3.66113466765123E-16,-1.,5.66153840231349E-16));
#46146=DIRECTION('ref_axis',(-0.996957691137886,3.20870996777813E-16,-0.0779446090567869));
#46147=DIRECTION('center_axis',(3.66113466765123E-16,1.,-5.66153840231349E-16));
#46148=DIRECTION('ref_axis',(0.996957691137886,-3.20870996777813E-16,0.0779446090567866));
#46149=DIRECTION('center_axis',(-3.66113466765123E-16,-1.,5.66153840231349E-16));
#46150=DIRECTION('ref_axis',(-0.996957691137886,3.20870996777813E-16,-0.0779446090567869));
#46151=DIRECTION('center_axis',(3.66113466765123E-16,1.,-5.66153840231349E-16));
#46152=DIRECTION('ref_axis',(-0.996957691137886,3.20870996777813E-16,-0.0779446090567869));
#46153=DIRECTION('center_axis',(-3.66113466765123E-16,-1.,5.66153840231349E-16));
#46154=DIRECTION('ref_axis',(-0.996957691137886,3.20870996777813E-16,-0.0779446090567869));
#46155=DIRECTION('center_axis',(3.66113466765123E-16,1.,-5.66153840231349E-16));
#46156=DIRECTION('ref_axis',(-0.996957691137886,3.20870996777813E-16,-0.0779446090567869));
#46157=DIRECTION('center_axis',(-3.66113466765123E-16,-1.,5.66153840231349E-16));
#46158=DIRECTION('ref_axis',(-0.996957691137886,3.20870996777813E-16,-0.0779446090567869));
#46159=DIRECTION('center_axis',(3.66113466765123E-16,1.,-5.66153840231349E-16));
#46160=DIRECTION('ref_axis',(-0.996957691137886,3.20870996777813E-16,-0.0779446090567869));
#46161=DIRECTION('center_axis',(-3.66113466765123E-16,-1.,5.66153840231349E-16));
#46162=DIRECTION('ref_axis',(-0.996957691137886,3.20870996777813E-16,-0.0779446090567869));
#46163=DIRECTION('center_axis',(3.66113466765123E-16,1.,-5.66153840231349E-16));
#46164=DIRECTION('ref_axis',(-0.996957691137886,3.20870996777813E-16,-0.0779446090567869));
#46165=DIRECTION('center_axis',(-3.66113466765123E-16,-1.,5.66153840231349E-16));
#46166=DIRECTION('ref_axis',(-0.996957691137886,3.20870996777813E-16,-0.0779446090567869));
#46167=DIRECTION('center_axis',(3.66113466765123E-16,1.,-5.66153840231349E-16));
#46168=DIRECTION('ref_axis',(-0.996957691137886,3.20870996777813E-16,-0.0779446090567869));
#46169=DIRECTION('center_axis',(-3.66113466765123E-16,-1.,5.66153840231349E-16));
#46170=DIRECTION('ref_axis',(-0.996957691137886,3.20870996777813E-16,-0.0779446090567869));
#46171=DIRECTION('center_axis',(3.66113466765123E-16,1.,-5.66153840231349E-16));
#46172=DIRECTION('ref_axis',(-0.996957691137886,3.20870996777813E-16,-0.0779446090567869));
#46173=DIRECTION('center_axis',(-3.66113466765123E-16,-1.,5.66153840231349E-16));
#46174=DIRECTION('ref_axis',(-0.996957691137886,3.20870996777813E-16,-0.0779446090567869));
#46175=DIRECTION('center_axis',(3.66113466765123E-16,1.,-5.66153840231349E-16));
#46176=DIRECTION('ref_axis',(-0.996957691137886,3.20870996777813E-16,-0.0779446090567869));
#46177=DIRECTION('center_axis',(-3.66113466765123E-16,-1.,5.66153840231349E-16));
#46178=DIRECTION('ref_axis',(-0.996957691137886,3.20870996777813E-16,-0.0779446090567869));
#46179=DIRECTION('center_axis',(3.66113466765123E-16,1.,-5.66153840231349E-16));
#46180=DIRECTION('ref_axis',(-0.996957691137886,3.20870996777813E-16,-0.0779446090567869));
#46181=DIRECTION('center_axis',(-3.66113466765123E-16,-1.,5.66153840231349E-16));
#46182=DIRECTION('ref_axis',(-0.996957691137886,3.20870996777813E-16,-0.0779446090567869));
#46183=DIRECTION('center_axis',(3.66113466765123E-16,1.,-5.66153840231349E-16));
#46184=DIRECTION('ref_axis',(-0.996957691137886,3.20870996777813E-16,-0.0779446090567869));
#46185=DIRECTION('center_axis',(-3.66113466765123E-16,-1.,5.66153840231349E-16));
#46186=DIRECTION('ref_axis',(-0.996957691137886,3.20870996777813E-16,-0.0779446090567869));
#46187=DIRECTION('center_axis',(3.66113466765123E-16,1.,-5.66153840231349E-16));
#46188=DIRECTION('ref_axis',(-0.996957691137886,3.20870996777813E-16,-0.0779446090567869));
#46189=DIRECTION('center_axis',(-3.66113466765123E-16,-1.,5.66153840231349E-16));
#46190=DIRECTION('ref_axis',(-0.996957691137886,3.20870996777813E-16,-0.0779446090567869));
#46191=DIRECTION('center_axis',(3.66113466765123E-16,1.,-5.66153840231349E-16));
#46192=DIRECTION('ref_axis',(-0.996957691137886,3.20870996777813E-16,-0.0779446090567869));
#46193=DIRECTION('center_axis',(-3.66113466765123E-16,-1.,5.66153840231349E-16));
#46194=DIRECTION('ref_axis',(-0.996957691137886,3.20870996777813E-16,-0.0779446090567869));
#46195=DIRECTION('center_axis',(3.66113466765123E-16,1.,-5.66153840231349E-16));
#46196=DIRECTION('ref_axis',(-0.996957691137886,3.20870996777813E-16,-0.0779446090567869));
#46197=DIRECTION('center_axis',(-3.66113466765123E-16,-1.,5.66153840231349E-16));
#46198=DIRECTION('ref_axis',(-0.996957691137886,3.20870996777813E-16,-0.0779446090567869));
#46199=DIRECTION('center_axis',(3.66113466765123E-16,1.,-5.66153840231349E-16));
#46200=DIRECTION('ref_axis',(-0.996957691137886,3.20870996777813E-16,-0.0779446090567869));
#46201=DIRECTION('center_axis',(-3.66113466765123E-16,-1.,5.66153840231349E-16));
#46202=DIRECTION('ref_axis',(-0.996957691137886,3.20870996777813E-16,-0.0779446090567869));
#46203=DIRECTION('center_axis',(3.66113466765123E-16,1.,-5.66153840231349E-16));
#46204=DIRECTION('ref_axis',(-0.996957691137886,3.20870996777813E-16,-0.0779446090567869));
#46205=DIRECTION('center_axis',(-3.66113466765123E-16,-1.,5.66153840231349E-16));
#46206=DIRECTION('ref_axis',(-0.996957691137886,3.20870996777813E-16,-0.0779446090567869));
#46207=DIRECTION('center_axis',(3.66113466765123E-16,1.,-5.66153840231349E-16));
#46208=DIRECTION('ref_axis',(-0.996957691137886,3.20870996777813E-16,-0.0779446090567869));
#46209=DIRECTION('center_axis',(-3.66113466765123E-16,-1.,5.66153840231349E-16));
#46210=DIRECTION('ref_axis',(-0.996957691137886,3.20870996777813E-16,-0.0779446090567869));
#46211=DIRECTION('center_axis',(3.66113466765123E-16,1.,-5.66153840231349E-16));
#46212=DIRECTION('ref_axis',(-0.996957691137886,3.20870996777813E-16,-0.0779446090567869));
#46213=DIRECTION('center_axis',(-3.66113466765123E-16,-1.,5.66153840231349E-16));
#46214=DIRECTION('ref_axis',(-0.996957691137886,3.20870996777813E-16,-0.0779446090567869));
#46215=DIRECTION('center_axis',(3.66113466765123E-16,1.,-5.66153840231349E-16));
#46216=DIRECTION('ref_axis',(-0.996957691137886,3.20870996777813E-16,-0.0779446090567869));
#46217=DIRECTION('center_axis',(-3.66113466765123E-16,-1.,5.66153840231349E-16));
#46218=DIRECTION('ref_axis',(-0.996957691137886,3.20870996777813E-16,-0.0779446090567869));
#46219=DIRECTION('center_axis',(3.66113466765123E-16,1.,-5.66153840231349E-16));
#46220=DIRECTION('ref_axis',(-0.996957691137886,3.20870996777813E-16,-0.0779446090567869));
#46221=DIRECTION('center_axis',(-3.66113466765123E-16,-1.,5.66153840231349E-16));
#46222=DIRECTION('ref_axis',(-0.996957691137886,3.20870996777813E-16,-0.0779446090567869));
#46223=DIRECTION('center_axis',(3.66113466765123E-16,1.,-5.66153840231349E-16));
#46224=DIRECTION('ref_axis',(-0.996957691137886,3.20870996777813E-16,-0.0779446090567869));
#46225=DIRECTION('center_axis',(-3.66113466765123E-16,-1.,5.66153840231349E-16));
#46226=DIRECTION('ref_axis',(-0.996957691137886,3.20870996777813E-16,-0.0779446090567869));
#46227=DIRECTION('center_axis',(3.66113466765123E-16,1.,-5.66153840231349E-16));
#46228=DIRECTION('ref_axis',(-0.996957691137886,3.20870996777813E-16,-0.0779446090567869));
#46229=DIRECTION('center_axis',(-3.66113466765123E-16,-1.,5.66153840231349E-16));
#46230=DIRECTION('ref_axis',(-0.996957691137886,3.20870996777813E-16,-0.0779446090567869));
#46231=DIRECTION('center_axis',(3.66113466765123E-16,1.,-5.66153840231349E-16));
#46232=DIRECTION('ref_axis',(-0.996957691137886,3.20870996777813E-16,-0.0779446090567869));
#46233=DIRECTION('center_axis',(-3.66113466765123E-16,-1.,5.66153840231349E-16));
#46234=DIRECTION('ref_axis',(-0.996957691137886,3.20870996777813E-16,-0.0779446090567869));
#46235=DIRECTION('center_axis',(3.66113466765123E-16,1.,-5.66153840231349E-16));
#46236=DIRECTION('ref_axis',(-0.996957691137886,3.20870996777813E-16,-0.0779446090567869));
#46237=DIRECTION('center_axis',(-3.66113466765123E-16,-1.,5.66153840231349E-16));
#46238=DIRECTION('ref_axis',(-0.996957691137886,3.20870996777813E-16,-0.0779446090567869));
#46239=DIRECTION('center_axis',(3.66113466765123E-16,1.,-5.66153840231349E-16));
#46240=DIRECTION('ref_axis',(-0.996957691137886,3.20870996777813E-16,-0.0779446090567869));
#46241=DIRECTION('center_axis',(-3.66113466765123E-16,-1.,5.66153840231349E-16));
#46242=DIRECTION('ref_axis',(-0.996957691137886,3.20870996777813E-16,-0.0779446090567869));
#46243=DIRECTION('center_axis',(3.66113466765123E-16,1.,-5.66153840231349E-16));
#46244=DIRECTION('ref_axis',(-0.996957691137886,3.20870996777813E-16,-0.0779446090567869));
#46245=DIRECTION('center_axis',(-3.66113466765123E-16,-1.,5.66153840231349E-16));
#46246=DIRECTION('ref_axis',(-0.996957691137886,3.20870996777813E-16,-0.0779446090567869));
#46247=DIRECTION('center_axis',(3.66113466765123E-16,1.,-5.66153840231349E-16));
#46248=DIRECTION('ref_axis',(-0.996957691137886,3.20870996777813E-16,-0.0779446090567869));
#46249=DIRECTION('center_axis',(-3.66113466765123E-16,-1.,5.66153840231349E-16));
#46250=DIRECTION('ref_axis',(-0.996957691137886,3.20870996777813E-16,-0.0779446090567869));
#46251=DIRECTION('center_axis',(3.66113466765123E-16,1.,-5.66153840231349E-16));
#46252=DIRECTION('ref_axis',(-0.996957691137886,3.20870996777813E-16,-0.0779446090567869));
#46253=DIRECTION('center_axis',(-3.66113466765123E-16,-1.,5.66153840231349E-16));
#46254=DIRECTION('ref_axis',(-0.996957691137886,3.20870996777813E-16,-0.0779446090567869));
#46255=DIRECTION('center_axis',(3.66113466765123E-16,1.,-5.66153840231349E-16));
#46256=DIRECTION('ref_axis',(-0.996957691137886,3.20870996777813E-16,-0.0779446090567869));
#46257=DIRECTION('center_axis',(-3.66113466765123E-16,-1.,5.66153840231349E-16));
#46258=DIRECTION('ref_axis',(-0.996957691137886,3.20870996777813E-16,-0.0779446090567869));
#46259=DIRECTION('center_axis',(3.66113466765123E-16,1.,-5.66153840231349E-16));
#46260=DIRECTION('ref_axis',(-0.996957691137886,3.20870996777813E-16,-0.0779446090567869));
#46261=DIRECTION('center_axis',(-3.66113466765123E-16,-1.,5.66153840231349E-16));
#46262=DIRECTION('ref_axis',(-0.996957691137886,3.20870996777813E-16,-0.0779446090567869));
#46263=DIRECTION('center_axis',(3.66113466765123E-16,1.,-5.66153840231349E-16));
#46264=DIRECTION('ref_axis',(-0.0201496574551477,-5.58661835927051E-16,
-0.999796975042654));
#46265=DIRECTION('',(3.66113466765123E-16,1.,-5.66153840231349E-16));
#46266=DIRECTION('center_axis',(-3.66113466765123E-16,-1.,5.66153840231349E-16));
#46267=DIRECTION('ref_axis',(-0.0201496574551477,-5.58661835927051E-16,
-0.999796975042654));
#46268=DIRECTION('',(3.66113466765123E-16,1.,-5.66153840231349E-16));
#46269=DIRECTION('center_axis',(3.66113466765123E-16,1.,-5.66153840231349E-16));
#46270=DIRECTION('ref_axis',(0.883011221719068,-5.89007665877645E-16,-0.469351874736002));
#46271=DIRECTION('center_axis',(-3.66113466765123E-16,-1.,5.66153840231349E-16));
#46272=DIRECTION('ref_axis',(0.883011221719068,-5.89007665877645E-16,-0.469351874736002));
#46273=DIRECTION('',(-3.66113466765123E-16,-1.,5.66153840231349E-16));
#46274=DIRECTION('center_axis',(3.66113466765123E-16,1.,-5.66153840231349E-16));
#46275=DIRECTION('ref_axis',(-0.963351194554152,2.00828862743045E-16,-0.268243314830189));
#46276=DIRECTION('center_axis',(-3.66113466765123E-16,-1.,5.66153840231349E-16));
#46277=DIRECTION('ref_axis',(-0.963351194554152,2.00828862743045E-16,-0.268243314830189));
#46278=DIRECTION('center_axis',(3.66113466765123E-16,1.,-5.66153840231349E-16));
#46279=DIRECTION('ref_axis',(-0.996957691137886,3.20870996777813E-16,-0.0779446090567869));
#46280=DIRECTION('center_axis',(-3.66113466765123E-16,-1.,5.66153840231349E-16));
#46281=DIRECTION('ref_axis',(-0.996957691137886,3.20870996777813E-16,-0.0779446090567869));
#46282=DIRECTION('center_axis',(-3.66113466765123E-16,-1.,5.66153840231349E-16));
#46283=DIRECTION('ref_axis',(-0.996957691137886,3.20870996777813E-16,-0.0779446090567869));
#46284=DIRECTION('',(0.,0.,1.));
#46285=DIRECTION('',(1.,0.,0.));
#46286=DIRECTION('',(0.,0.,1.));
#46287=DIRECTION('',(1.,0.,0.));
#46288=DIRECTION('axis',(0.,0.,1.));
#46289=DIRECTION('refdir',(1.,0.,0.));
#46290=DIRECTION('axis',(0.,0.,1.));
#46291=DIRECTION('refdir',(1.,0.,0.));
#46292=DIRECTION('center_axis',(-6.49090813559456E-14,1.,-2.55622388633908E-14));
#46293=DIRECTION('ref_axis',(0.581108581114938,5.85224396950113E-14,0.813826036051062));
#46294=DIRECTION('center_axis',(-7.0376604876213E-14,1.,-8.61946552381524E-15));
#46295=DIRECTION('ref_axis',(-2.74761886345665E-15,8.61946552381505E-15,
1.));
#46296=DIRECTION('center_axis',(-7.0376604876213E-14,1.,-8.61946552381524E-15));
#46297=DIRECTION('ref_axis',(-2.74761886345665E-15,8.61946552381505E-15,
1.));
#46298=DIRECTION('',(0.410905818312113,-0.707106781186504,0.575461908797893));
#46299=DIRECTION('center_axis',(6.80591214965025E-14,-1.,9.9941788598046E-15));
#46300=DIRECTION('ref_axis',(0.581108581114922,4.76832624898209E-14,0.813826036051073));
#46301=DIRECTION('center_axis',(6.76186946307289E-14,-1.,8.61946552381525E-15));
#46302=DIRECTION('ref_axis',(2.76820162751153E-15,8.61946552381544E-15,
1.));
#46303=DIRECTION('center_axis',(-6.65083299171228E-14,1.,-9.75928747178892E-15));
#46304=DIRECTION('ref_axis',(0.581108581114964,4.65909234683137E-14,0.813826036051043));
#46305=DIRECTION('',(-0.503254793602722,0.499999999999961,-0.704794021481398));
#46306=DIRECTION('center_axis',(6.76186946307289E-14,-1.,8.61946552381525E-15));
#46307=DIRECTION('ref_axis',(8.28402211847971E-15,8.61946552381581E-15,
1.));
#46308=DIRECTION('center_axis',(6.76186946307289E-14,-1.,8.61946552381525E-15));
#46309=DIRECTION('ref_axis',(8.28402211847971E-15,8.61946552381581E-15,
1.));
#46310=DIRECTION('center_axis',(-6.76186946307289E-14,1.,-8.61946552381525E-15));
#46311=DIRECTION('ref_axis',(-2.76820162751153E-15,-8.61946552381544E-15,
-1.));
#46312=DIRECTION('',(-6.76186946307289E-14,1.,-8.61946552381525E-15));
#46313=DIRECTION('center_axis',(-6.76186946307289E-14,1.,-8.61946552381525E-15));
#46314=DIRECTION('ref_axis',(-2.76820162751153E-15,-8.61946552381544E-15,
-1.));
#46315=DIRECTION('center_axis',(7.67012022460283E-14,-1.,8.61946552381523E-15));
#46316=DIRECTION('ref_axis',(-7.30945543516121E-15,-8.61946552381579E-15,
-1.));
#46317=DIRECTION('',(6.76186946307289E-14,-1.,8.61946552381525E-15));
#46318=DIRECTION('center_axis',(6.30774408230792E-14,-1.,8.61946552381526E-15));
#46319=DIRECTION('ref_axis',(-7.30945543516121E-15,-8.61946552381573E-15,
-1.));
#46320=DIRECTION('center_axis',(6.76186946307289E-14,-1.,8.61946552381525E-15));
#46321=DIRECTION('ref_axis',(2.76820162751153E-15,8.61946552381544E-15,
1.));
#46322=DIRECTION('center_axis',(6.82810966368524E-14,-1.,1.06870343811432E-14));
#46323=DIRECTION('ref_axis',(0.581108581114924,4.83761180111596E-14,0.813826036051071));
#46324=DIRECTION('center_axis',(-6.76186946307289E-14,1.,-8.61946552381525E-15));
#46325=DIRECTION('ref_axis',(-2.76820162751153E-15,-8.61946552381544E-15,
-1.));
#46326=DIRECTION('center_axis',(-6.69562926246054E-14,1.,-1.06870343811432E-14));
#46327=DIRECTION('ref_axis',(-0.581108581114914,-3.0211489376252E-14,0.813826036051079));
#46328=DIRECTION('center_axis',(6.76186946307289E-14,-1.,8.61946552381525E-15));
#46329=DIRECTION('ref_axis',(2.76820162751153E-15,8.61946552381544E-15,
1.));
#46330=DIRECTION('',(6.76186946307289E-14,-1.,8.61946552381525E-15));
#46331=DIRECTION('center_axis',(-6.13660760090327E-14,1.,9.49534209067263E-15));
#46332=DIRECTION('ref_axis',(0.581108581114914,2.79327967435979E-14,0.813826036051078));
#46333=DIRECTION('center_axis',(-6.76186946307289E-14,1.,-8.61946552381525E-15));
#46334=DIRECTION('ref_axis',(7.34396516680413E-14,8.61946552382022E-15,
1.));
#46335=DIRECTION('center_axis',(-6.76186946307289E-14,1.,-8.61946552381525E-15));
#46336=DIRECTION('ref_axis',(7.34396516680413E-14,8.61946552382022E-15,
1.));
#46337=DIRECTION('',(0.410905818312066,-0.707106781186573,0.575461908797841));
#46338=DIRECTION('center_axis',(6.25513333585901E-14,-1.,7.93981538629056E-15));
#46339=DIRECTION('ref_axis',(0.581108581114919,4.28107450576588E-14,0.813826036051075));
#46340=DIRECTION('center_axis',(6.76186946307289E-14,-1.,8.61946552381525E-15));
#46341=DIRECTION('ref_axis',(2.76820162751153E-15,8.61946552381544E-15,
1.));
#46342=DIRECTION('center_axis',(-6.82145042037028E-14,1.,-8.5945800386633E-15));
#46343=DIRECTION('ref_axis',(0.581108581114921,4.66345267536606E-14,0.813826036051073));
#46344=DIRECTION('',(-0.503254793602685,0.499999999999963,-0.704794021481423));
#46345=DIRECTION('center_axis',(6.76186946307289E-14,-1.,8.61946552381525E-15));
#46346=DIRECTION('ref_axis',(3.45767918888255E-15,8.61946552381548E-15,
1.));
#46347=DIRECTION('center_axis',(6.76186946307289E-14,-1.,8.61946552381525E-15));
#46348=DIRECTION('ref_axis',(3.45767918888255E-15,8.61946552381548E-15,
1.));
#46349=DIRECTION('center_axis',(-6.76186946307289E-14,1.,-8.61946552381525E-15));
#46350=DIRECTION('ref_axis',(-2.76820162751153E-15,-8.61946552381544E-15,
-1.));
#46351=DIRECTION('',(-6.76186946307289E-14,1.,-8.61946552381525E-15));
#46352=DIRECTION('center_axis',(-6.76186946307289E-14,1.,-8.61946552381525E-15));
#46353=DIRECTION('ref_axis',(-2.76820162751153E-15,-8.61946552381544E-15,
-1.));
#46354=DIRECTION('center_axis',(7.67012022460283E-14,-1.,8.61946552381523E-15));
#46355=DIRECTION('ref_axis',(-3.19394417197869E-15,-8.61946552381547E-15,
-1.));
#46356=DIRECTION('',(6.76186946307289E-14,-1.,8.61946552381525E-15));
#46357=DIRECTION('center_axis',(6.30774408230794E-14,-1.,8.61946552381514E-15));
#46358=DIRECTION('ref_axis',(5.55585269644891E-14,-8.61946552381163E-15,
-1.));
#46359=DIRECTION('center_axis',(6.76186946307289E-14,-1.,8.61946552381525E-15));
#46360=DIRECTION('ref_axis',(2.76820162751153E-15,8.61946552381544E-15,
1.));
#46361=DIRECTION('center_axis',(6.82810966368524E-14,-1.,1.06870343811432E-14));
#46362=DIRECTION('ref_axis',(0.581108581114918,4.83761180111593E-14,0.813826036051075));
#46363=DIRECTION('center_axis',(-6.76186946307289E-14,1.,-8.61946552381525E-15));
#46364=DIRECTION('ref_axis',(-2.76820162751153E-15,-8.61946552381544E-15,
-1.));
#46365=DIRECTION('center_axis',(-6.69562926246054E-14,1.,-1.06870343811432E-14));
#46366=DIRECTION('ref_axis',(-0.58110858111492,-3.02114893762525E-14,0.813826036051075));
#46367=DIRECTION('center_axis',(6.76186946307289E-14,-1.,8.61946552381525E-15));
#46368=DIRECTION('ref_axis',(4.22518722413247E-15,8.61946552381554E-15,
1.));
#46369=DIRECTION('',(6.76186946307289E-14,-1.,8.61946552381525E-15));
#46370=DIRECTION('center_axis',(-1.04261204031615E-14,-3.33541910048363E-16,
1.));
#46371=DIRECTION('ref_axis',(-0.581108581114994,0.813826036051022,-5.7872629435037E-15));
#46372=DIRECTION('center_axis',(2.76820162751153E-15,8.61946552381544E-15,
1.));
#46373=DIRECTION('ref_axis',(0.581108581114867,0.813826036051112,-8.62337118012903E-15));
#46374=DIRECTION('',(-0.410905818312093,0.575461908797838,-0.70710678118656));
#46375=DIRECTION('center_axis',(-3.80148262708044E-15,-5.39426451924816E-15,
-1.));
#46376=DIRECTION('ref_axis',(-0.581108581114975,0.813826036051035,-2.18091873555453E-15));
#46377=DIRECTION('center_axis',(2.76820162751153E-15,8.61946552381544E-15,
1.));
#46378=DIRECTION('ref_axis',(0.581108581114867,0.813826036051112,-8.62337118012903E-15));
#46379=DIRECTION('center_axis',(-2.76820162751153E-15,-8.61946552381544E-15,
-1.));
#46380=DIRECTION('ref_axis',(6.76186946307289E-14,-1.,8.61946552381525E-15));
#46381=DIRECTION('center_axis',(2.76820162751153E-15,8.61946552381544E-15,
1.));
#46382=DIRECTION('ref_axis',(-6.76186946307289E-14,1.,-8.61946552381525E-15));
#46383=DIRECTION('center_axis',(4.6446765469921E-16,-8.61946552381522E-15,
-1.));
#46384=DIRECTION('ref_axis',(-6.11533560663074E-14,1.,-8.61946552381525E-15));
#46385=DIRECTION('center_axis',(4.6446765469921E-16,-8.61946552381522E-15,
-1.));
#46386=DIRECTION('ref_axis',(-6.11533560663074E-14,1.,-8.61946552381525E-15));
#46387=DIRECTION('',(2.76820162751153E-15,8.61946552381544E-15,1.));
#46388=DIRECTION('center_axis',(-3.46259038420886E-16,8.70807119655905E-15,
1.));
#46389=DIRECTION('ref_axis',(0.581108581114959,-0.813826036051046,7.28806916206094E-15));
#46390=DIRECTION('',(-0.503254793602683,0.704794021481399,0.499999999999998));
#46391=DIRECTION('center_axis',(2.76820162751153E-15,8.61946552381544E-15,
1.));
#46392=DIRECTION('ref_axis',(6.76186946307289E-14,-1.,8.61946552381525E-15));
#46393=DIRECTION('center_axis',(-1.33644605120271E-14,-8.61946552381615E-15,
-1.));
#46394=DIRECTION('ref_axis',(4.11280474194391E-14,-1.,8.6194655238156E-15));
#46395=DIRECTION('',(-2.76820162751153E-15,-8.61946552381544E-15,-1.));
#46396=DIRECTION('center_axis',(-2.76820162751153E-15,-8.61946552381544E-15,
-1.));
#46397=DIRECTION('ref_axis',(0.58110858111497,-0.813826036051039,5.40611974012193E-15));
#46398=DIRECTION('center_axis',(-2.76820162751153E-15,-8.61946552381544E-15,
-1.));
#46399=DIRECTION('ref_axis',(6.76186946307289E-14,-1.,8.61946552381525E-15));
#46400=DIRECTION('center_axis',(-2.76820162751153E-15,-8.61946552381544E-15,
-1.));
#46401=DIRECTION('ref_axis',(-0.581108581114972,0.813826036051037,-5.40611974012191E-15));
#46402=DIRECTION('center_axis',(2.76820162751153E-15,8.61946552381544E-15,
1.));
#46403=DIRECTION('ref_axis',(-6.76186946307289E-14,1.,-8.61946552381525E-15));
#46404=DIRECTION('center_axis',(1.07977124127116E-14,7.41326354248036E-15,
1.));
#46405=DIRECTION('ref_axis',(0.581108581114866,0.813826036051113,-1.23077502224163E-14));
#46406=DIRECTION('',(2.76820162751153E-15,8.61946552381544E-15,1.));
#46407=DIRECTION('center_axis',(2.76820162751153E-15,8.61946552381544E-15,
1.));
#46408=DIRECTION('ref_axis',(-6.76186946307289E-14,1.,-8.61946552381525E-15));
#46409=DIRECTION('center_axis',(-6.76186946307289E-14,1.,-8.61946552381525E-15));
#46410=DIRECTION('ref_axis',(-1.91671653857721E-15,-8.61946552381538E-15,
-1.));
#46411=DIRECTION('center_axis',(7.67012022460283E-14,-1.,8.61946552381523E-15));
#46412=DIRECTION('ref_axis',(-3.33585835346774E-15,-8.61946552381548E-15,
-1.));
#46413=DIRECTION('',(6.76186946307289E-14,-1.,8.61946552381525E-15));
#46414=DIRECTION('center_axis',(6.30774408230794E-14,-1.,8.61946552381514E-15));
#46415=DIRECTION('ref_axis',(5.57004411459782E-14,-8.61946552381162E-15,
-1.));
#46416=DIRECTION('center_axis',(6.76186946307289E-14,-1.,8.61946552381525E-15));
#46417=DIRECTION('ref_axis',(2.76820162751153E-15,8.61946552381544E-15,
1.));
#46418=DIRECTION('center_axis',(6.82810966368524E-14,-1.,1.06870343811432E-14));
#46419=DIRECTION('ref_axis',(0.581108581114921,4.83761180111595E-14,0.813826036051073));
#46420=DIRECTION('center_axis',(6.76186946307289E-14,-1.,8.61946552381525E-15));
#46421=DIRECTION('ref_axis',(3.56292104385022E-15,8.61946552381549E-15,
1.));
#46422=DIRECTION('',(6.76186946307289E-14,-1.,8.61946552381525E-15));
#46423=DIRECTION('center_axis',(-6.69562926246054E-14,1.,-1.06870343811432E-14));
#46424=DIRECTION('ref_axis',(-0.581108581114923,-3.02114893762527E-14,0.813826036051072));
#46425=DIRECTION('center_axis',(-6.76186946307289E-14,1.,-8.61946552381525E-15));
#46426=DIRECTION('ref_axis',(-2.76820162751153E-15,-8.61946552381544E-15,
-1.));
#46427=DIRECTION('center_axis',(-6.72644410420969E-14,1.,-1.18043088936533E-14));
#46428=DIRECTION('ref_axis',(0.581108581114921,4.86945978087055E-14,0.813826036051073));
#46429=DIRECTION('center_axis',(-6.76186946307289E-14,1.,-8.61946552381525E-15));
#46430=DIRECTION('ref_axis',(7.32672822776985E-14,8.6194655238202E-15,1.));
#46431=DIRECTION('center_axis',(-6.76186946307289E-14,1.,-8.61946552381525E-15));
#46432=DIRECTION('ref_axis',(7.32672822776985E-14,8.6194655238202E-15,1.));
#46433=DIRECTION('',(0.410905818312108,-0.707106781186502,0.575461908797899));
#46434=DIRECTION('center_axis',(6.25513333585901E-14,-1.,7.93981538629056E-15));
#46435=DIRECTION('ref_axis',(0.581108581114918,4.28107450576588E-14,0.813826036051075));
#46436=DIRECTION('center_axis',(6.76186946307289E-14,-1.,8.61946552381525E-15));
#46437=DIRECTION('ref_axis',(2.76820162751153E-15,8.61946552381544E-15,
1.));
#46438=DIRECTION('center_axis',(-6.76186946307289E-14,1.,-8.61946552381525E-15));
#46439=DIRECTION('ref_axis',(-1.733985285455E-15,-8.61946552381537E-15,
-1.));
#46440=DIRECTION('center_axis',(6.76186946307289E-14,-1.,8.61946552381525E-15));
#46441=DIRECTION('ref_axis',(-3.63004857922531E-15,-8.6194655238155E-15,
-1.));
#46442=DIRECTION('center_axis',(6.76186946307289E-14,-1.,8.61946552381525E-15));
#46443=DIRECTION('ref_axis',(-3.63004857922531E-15,-8.6194655238155E-15,
-1.));
#46444=DIRECTION('',(-6.76186946307289E-14,1.,-8.61946552381525E-15));
#46445=DIRECTION('center_axis',(-6.81874306457619E-14,1.,-9.83494824371944E-15));
#46446=DIRECTION('ref_axis',(0.581108581114921,4.76282380163844E-14,0.813826036051073));
#46447=DIRECTION('',(-0.503254793602685,0.499999999999962,-0.704794021481423));
#46448=DIRECTION('center_axis',(-6.76186946307289E-14,1.,-8.61946552381525E-15));
#46449=DIRECTION('ref_axis',(-2.76820162751153E-15,-8.61946552381544E-15,
-1.));
#46450=DIRECTION('center_axis',(7.67012022460283E-14,-1.,8.61946552381523E-15));
#46451=DIRECTION('ref_axis',(-7.30945543516121E-15,-8.61946552381579E-15,
-1.));
#46452=DIRECTION('',(6.76186946307289E-14,-1.,8.61946552381525E-15));
#46453=DIRECTION('center_axis',(6.30774408230792E-14,-1.,8.61946552381526E-15));
#46454=DIRECTION('ref_axis',(-7.30945543516121E-15,-8.61946552381573E-15,
-1.));
#46455=DIRECTION('center_axis',(6.76186946307289E-14,-1.,8.61946552381525E-15));
#46456=DIRECTION('ref_axis',(2.76820162751153E-15,8.61946552381544E-15,
1.));
#46457=DIRECTION('center_axis',(6.82810966368524E-14,-1.,1.06870343811432E-14));
#46458=DIRECTION('ref_axis',(0.58110858111492,4.83761180111593E-14,0.813826036051075));
#46459=DIRECTION('center_axis',(6.76186946307289E-14,-1.,8.61946552381525E-15));
#46460=DIRECTION('ref_axis',(2.76820162751153E-15,8.61946552381544E-15,
1.));
#46461=DIRECTION('',(6.76186946307289E-14,-1.,8.61946552381525E-15));
#46462=DIRECTION('center_axis',(-6.69562926246054E-14,1.,-1.06870343811432E-14));
#46463=DIRECTION('ref_axis',(-0.581108581114923,-3.02114893762527E-14,0.813826036051073));
#46464=DIRECTION('center_axis',(-6.76186946307289E-14,1.,-8.61946552381525E-15));
#46465=DIRECTION('ref_axis',(-2.76820162751153E-15,-8.61946552381544E-15,
-1.));
#46466=DIRECTION('center_axis',(-6.50143608507664E-14,1.,-1.90373382615731E-14));
#46467=DIRECTION('ref_axis',(0.581108581114934,5.32734845204624E-14,0.813826036051064));
#46468=DIRECTION('center_axis',(-7.0376604876213E-14,1.,-8.61946552381524E-15));
#46469=DIRECTION('ref_axis',(-2.74761886345663E-15,8.61946552381505E-15,
1.));
#46470=DIRECTION('center_axis',(-7.0376604876213E-14,1.,-8.61946552381524E-15));
#46471=DIRECTION('ref_axis',(-2.74761886345663E-15,8.61946552381505E-15,
1.));
#46472=DIRECTION('',(0.410905818312139,-0.707106781186458,0.575461908797931));
#46473=DIRECTION('center_axis',(6.76186946307289E-14,-1.,8.61946552381525E-15));
#46474=DIRECTION('ref_axis',(0.58110858111492,4.63085491538314E-14,0.813826036051074));
#46475=DIRECTION('center_axis',(6.76186946307289E-14,-1.,8.61946552381525E-15));
#46476=DIRECTION('ref_axis',(2.76820162751153E-15,8.61946552381544E-15,
1.));
#46477=DIRECTION('center_axis',(-6.76186946307289E-14,1.,-8.61946552381525E-15));
#46478=DIRECTION('ref_axis',(-2.76820162751153E-15,-8.61946552381544E-15,
-1.));
#46479=DIRECTION('center_axis',(6.76186946307289E-14,-1.,8.61946552381525E-15));
#46480=DIRECTION('ref_axis',(-1.37998426094479E-14,-8.61946552381618E-15,
-1.));
#46481=DIRECTION('center_axis',(6.76186946307289E-14,-1.,8.61946552381525E-15));
#46482=DIRECTION('ref_axis',(-1.37998426094479E-14,-8.61946552381618E-15,
-1.));
#46483=DIRECTION('',(-6.76186946307289E-14,1.,-8.61946552381525E-15));
#46484=DIRECTION('center_axis',(-6.63187474944986E-14,1.,-8.81955372150551E-15));
#46485=DIRECTION('ref_axis',(0.581108581114964,4.57159757027617E-14,0.813826036051043));
#46486=DIRECTION('',(-0.503254793602721,0.499999999999963,-0.704794021481396));
#46487=DIRECTION('center_axis',(-6.76186946307289E-14,1.,-8.61946552381525E-15));
#46488=DIRECTION('ref_axis',(-2.76820162751153E-15,-8.61946552381544E-15,
-1.));
#46489=DIRECTION('',(-2.76820162751153E-15,-8.61946552381544E-15,-1.));
#46490=DIRECTION('',(1.,6.76186946307289E-14,-2.76820162751211E-15));
#46491=DIRECTION('',(-2.76820162751153E-15,-8.61946552381544E-15,-1.));
#46492=DIRECTION('',(1.,6.76186946307289E-14,-2.76820162751211E-15));
#46493=DIRECTION('',(-1.,-6.76186946307289E-14,2.76820162751211E-15));
#46494=DIRECTION('',(-0.70710678118655,-5.39085200304644E-14,-0.707106781186545));
#46495=DIRECTION('',(-2.76820162751153E-15,-8.61946552381544E-15,-1.));
#46496=DIRECTION('',(0.707106781186546,4.17187549862773E-14,-0.707106781186549));
#46497=DIRECTION('',(1.,6.76186946307289E-14,-2.76820162751211E-15));
#46498=DIRECTION('',(0.707106781186549,5.39085200304643E-14,0.707106781186546));
#46499=DIRECTION('',(2.76820162751153E-15,8.61946552381544E-15,1.));
#46500=DIRECTION('',(-0.707106781186542,-4.1718754986277E-14,0.707106781186553));
#46501=DIRECTION('',(0.532208296737218,4.32845857166654E-14,0.846613447143423));
#46502=DIRECTION('',(1.,6.76186946307289E-14,-2.76820162751211E-15));
#46503=DIRECTION('center_axis',(-6.17447804712825E-15,0.0512482385726126,
-0.998685945652188));
#46504=DIRECTION('ref_axis',(-0.111182235210154,0.992494128249466,0.0509305013131333));
#46505=DIRECTION('center_axis',(2.76820162751153E-15,8.61946552381544E-15,
1.));
#46506=DIRECTION('ref_axis',(-0.139174864659284,0.990267820868208,-8.15031525445884E-15));
#46507=DIRECTION('',(0.0050617559519412,-0.0872986470839505,0.996169325388006));
#46508=DIRECTION('center_axis',(-2.76820162751153E-15,-8.61946552381544E-15,
-1.));
#46509=DIRECTION('ref_axis',(0.139174864659155,0.990267820868226,-8.92084342817569E-15));
#46510=DIRECTION('',(0.00506175595192408,0.0872986470839512,-0.996169325388006));
#46511=DIRECTION('center_axis',(0.138643505293337,0.986499799769915,0.087155742747649));
#46512=DIRECTION('ref_axis',(-8.7256367158859E-15,0.0880056703438852,-0.996119973691585));
#46513=DIRECTION('',(0.99026806874158,-0.139173100959999,-1.54166393399594E-15));
#46514=DIRECTION('',(0.0121297349846599,0.0863075490504521,-0.996194698091746));
#46515=DIRECTION('',(-0.99026806874158,0.139173100959999,1.54166393399594E-15));
#46516=DIRECTION('center_axis',(-1.0957857610087E-16,-0.0512482385723115,
-0.998685945652203));
#46517=DIRECTION('ref_axis',(0.111182235210143,-0.992494128249482,0.0509305013128334));
#46518=DIRECTION('center_axis',(2.76820162751153E-15,8.61946552381544E-15,
1.));
#46519=DIRECTION('ref_axis',(0.139174864659253,-0.990267820868213,8.15031525445896E-15));
#46520=DIRECTION('',(-0.00506175595193837,0.0872986470839675,0.996169325388004));
#46521=DIRECTION('center_axis',(-2.76820162751272E-15,6.38329582726006E-15,
-1.));
#46522=DIRECTION('ref_axis',(-0.13917486465911,-0.990267820868233,-5.93590836195989E-15));
#46523=DIRECTION('',(-0.00506175595193187,-0.0872986470839681,-0.996169325388004));
#46524=DIRECTION('center_axis',(-0.138643505293338,-0.986499799769913,0.0871557427476672));
#46525=DIRECTION('ref_axis',(-3.15693842339108E-15,0.0880056703439027,0.996119973691583));
#46526=DIRECTION('',(-0.99026806874158,0.139173100959998,1.54166393399595E-15));
#46527=DIRECTION('',(-0.698023464708466,0.159770101811378,0.698023464708437));
#46528=DIRECTION('',(-0.532208296737254,-4.32845857166677E-14,-0.8466134471434));
#46529=DIRECTION('',(-0.012129734984676,-0.0863075490504701,-0.996194698091745));
#46530=DIRECTION('',(0.99026806874158,-0.139173100959997,-1.54166393399596E-15));
#46531=DIRECTION('center_axis',(-0.13864350529347,0.986499799769896,0.0871557427476489));
#46532=DIRECTION('ref_axis',(-8.76900480278526E-15,0.0880056703438843,-0.996119973691585));
#46533=DIRECTION('',(-0.990268068741561,-0.139173100960131,3.94085942513142E-15));
#46534=DIRECTION('',(-0.0121297349846877,0.0863075490504512,-0.996194698091746));
#46535=DIRECTION('',(0.698023464708433,0.159770101811467,-0.698023464708449));
#46536=DIRECTION('',(0.99026806874156,0.139173100960136,-3.94085942513146E-15));
#46537=DIRECTION('center_axis',(-2.76820162751153E-15,-8.61946552381544E-15,
-1.));
#46538=DIRECTION('ref_axis',(6.76186946307289E-14,-1.,8.61946552381525E-15));
#46539=DIRECTION('',(-6.76186946307289E-14,1.,-8.61946552381525E-15));
#46540=DIRECTION('',(1.,6.76186946307289E-14,-2.76820162751211E-15));
#46541=DIRECTION('',(-6.76186946307289E-14,1.,-8.61946552381525E-15));
#46542=DIRECTION('center_axis',(3.60302193317522E-14,1.60759898378342E-13,
-1.));
#46543=DIRECTION('ref_axis',(0.305752646092157,0.952110980614993,1.64077599388534E-13));
#46544=DIRECTION('center_axis',(-2.76820162751153E-15,-8.61946552381544E-15,
-1.));
#46545=DIRECTION('ref_axis',(6.76186946307289E-14,-1.,8.61946552381525E-15));
#46546=DIRECTION('',(-0.990268068741561,-0.139173100960133,3.94085942513144E-15));
#46547=DIRECTION('center_axis',(-4.15666225867972E-14,1.6075989837832E-13,
-1.));
#46548=DIRECTION('ref_axis',(0.139173100960163,-0.990268068741557,-1.64980349860033E-13));
#46549=DIRECTION('',(1.,6.76186946307289E-14,-2.76820162751211E-15));
#46550=DIRECTION('',(-6.76186946307289E-14,1.,-8.61946552381525E-15));
#46551=DIRECTION('',(1.,6.76186946307289E-14,-2.76820162751211E-15));
#46552=DIRECTION('',(-6.76186946307289E-14,1.,-8.61946552381525E-15));
#46553=DIRECTION('center_axis',(0.138643505293472,-0.986499799769894,0.0871557427476665));
#46554=DIRECTION('ref_axis',(-3.24020515023797E-15,0.0880056703439028,0.996119973691583));
#46555=DIRECTION('',(0.990268068741561,0.139173100960135,-3.94085942513146E-15));
#46556=DIRECTION('',(0.0121297349846716,-0.08630754905047,-0.996194698091745));
#46557=DIRECTION('center_axis',(-2.76820162751153E-15,-8.61946552381544E-15,
-1.));
#46558=DIRECTION('ref_axis',(6.76186946307289E-14,-1.,8.61946552381525E-15));
#46559=DIRECTION('center_axis',(1.261874465981E-15,8.2847073667892E-15,
1.));
#46560=DIRECTION('ref_axis',(0.139173100959999,0.99026806874158,-8.3797001466523E-15));
#46561=DIRECTION('',(-1.,-6.76186946307289E-14,2.76820162751211E-15));
#46562=DIRECTION('',(-6.76186946307289E-14,1.,-8.61946552381525E-15));
#46563=DIRECTION('',(1.,6.76186946307289E-14,-2.76820162751211E-15));
#46564=DIRECTION('center_axis',(-2.44452695549615E-16,9.28898183786753E-15,
1.));
#46565=DIRECTION('ref_axis',(0.545502031847834,0.838109499558312,-7.6518344774284E-15));
#46566=DIRECTION('center_axis',(2.76820162751153E-15,8.61946552381544E-15,
1.));
#46567=DIRECTION('ref_axis',(-0.139173100960041,-0.990268068741574,8.9208406824367E-15));
#46568=DIRECTION('',(1.,6.76186946307289E-14,-2.76820162751211E-15));
#46569=DIRECTION('',(6.76186946307289E-14,-1.,8.61946552381525E-15));
#46570=DIRECTION('',(-1.,-6.76186946307289E-14,2.76820162751211E-15));
#46571=DIRECTION('center_axis',(2.76820162751153E-15,8.61946552381544E-15,
1.));
#46572=DIRECTION('ref_axis',(-0.54550203184785,-0.838109499558302,8.73411554899706E-15));
#46573=DIRECTION('center_axis',(-2.86014741974442E-15,-8.33247325201429E-15,
-1.));
#46574=DIRECTION('ref_axis',(-0.581108581114976,0.813826036051034,-5.11912746832073E-15));
#46575=DIRECTION('center_axis',(-1.,-6.76186946307289E-14,2.76820162751211E-15));
#46576=DIRECTION('ref_axis',(6.76186946307289E-14,-1.,8.61946552381525E-15));
#46577=DIRECTION('center_axis',(-1.,-6.76186946307289E-14,2.76820162751211E-15));
#46578=DIRECTION('ref_axis',(5.34212284942708E-14,-0.813826036051078,-0.581108581114915));
#46579=DIRECTION('',(-1.,-6.76186946307289E-14,2.76820162751211E-15));
#46580=DIRECTION('center_axis',(1.,6.76186946307289E-14,-2.53239663548226E-15));
#46581=DIRECTION('ref_axis',(6.76186946307289E-14,-1.,4.84658565133759E-15));
#46582=DIRECTION('center_axis',(1.,6.76186946307289E-14,-2.53239663548226E-15));
#46583=DIRECTION('ref_axis',(6.76186946307289E-14,-1.,4.84658565133759E-15));
#46584=DIRECTION('center_axis',(-5.05637727264981E-14,0.719339800338649,
-0.694658370458999));
#46585=DIRECTION('ref_axis',(4.49806146187151E-14,-0.694658370458999,-0.719339800338649));
#46586=DIRECTION('center_axis',(-3.56199649102086E-14,0.719339800338649,
-0.694658370458999));
#46587=DIRECTION('ref_axis',(-4.85907466234332E-15,0.694658370458999,0.719339800338649));
#46588=DIRECTION('',(-4.49806146187153E-14,0.694658370459002,0.719339800338646));
#46589=DIRECTION('center_axis',(1.,6.76186946307289E-14,-2.76820162751211E-15));
#46590=DIRECTION('ref_axis',(-6.76186946307289E-14,1.,-8.61946552381525E-15));
#46591=DIRECTION('',(4.8963169830778E-14,-0.694658370458992,0.719339800338656));
#46592=DIRECTION('',(-6.76741119925271E-14,0.999390827019096,-0.0348994967025082));
#46593=DIRECTION('',(-6.74808943053847E-14,0.999390827019096,0.0348994967024911));
#46594=DIRECTION('',(4.49806146187149E-14,-0.694658370458996,-0.719339800338652));
#46595=DIRECTION('',(2.76820162751153E-15,8.61946552381544E-15,1.));
#46596=DIRECTION('',(4.89631698307778E-14,-0.694658370458988,0.71933980033866));
#46597=DIRECTION('center_axis',(-1.,-6.76186946307289E-14,2.76820162751211E-15));
#46598=DIRECTION('ref_axis',(5.34212284942709E-14,-0.813826036051079,-0.581108581114913));
#46599=DIRECTION('center_axis',(-1.,-6.76186946307289E-14,2.76820162751211E-15));
#46600=DIRECTION('ref_axis',(5.34212284942708E-14,-0.813826036051078,-0.581108581114915));
#46601=DIRECTION('center_axis',(-1.,-6.71637446241253E-14,6.1602351414295E-15));
#46602=DIRECTION('ref_axis',(5.10798385514284E-14,-0.813826036051077,-0.581108581114916));
#46603=DIRECTION('center_axis',(-1.,-6.76186946307289E-14,2.76820162751211E-15));
#46604=DIRECTION('ref_axis',(6.76186946307289E-14,-1.,8.61946552381525E-15));
#46605=DIRECTION('',(-1.,-6.76186946307289E-14,2.76820162751211E-15));
#46606=DIRECTION('center_axis',(1.,6.76186946307289E-14,-2.53239663548226E-15));
#46607=DIRECTION('ref_axis',(6.76186946307289E-14,-1.,6.73302558757642E-15));
#46608=DIRECTION('center_axis',(1.,6.76186946307289E-14,-2.53239663548226E-15));
#46609=DIRECTION('ref_axis',(6.76186946307289E-14,-1.,6.73302558757642E-15));
#46610=DIRECTION('center_axis',(4.67178638631601E-14,-0.719339800338664,
-0.694658370458984));
#46611=DIRECTION('ref_axis',(4.89631698307775E-14,-0.694658370458984,0.719339800338664));
#46612=DIRECTION('',(1.,6.76186946307289E-14,-2.76820162751211E-15));
#46613=DIRECTION('center_axis',(6.48738920511758E-14,-0.719339800338663,
-0.694658370458985));
#46614=DIRECTION('ref_axis',(7.79045361699332E-14,-0.694658370458985,0.719339800338663));
#46615=DIRECTION('center_axis',(5.12637372416684E-15,-0.0348994967024915,
0.999390827019096));
#46616=DIRECTION('ref_axis',(-6.74808943053847E-14,0.999390827019096,0.0348994967024915));
#46617=DIRECTION('',(1.,6.76186946307289E-14,-2.76820162751211E-15));
#46618=DIRECTION('',(1.,6.76186946307289E-14,-2.76820162751211E-15));
#46619=DIRECTION('center_axis',(-7.21499697121947E-15,-0.0348994967024795,
0.999390827019097));
#46620=DIRECTION('ref_axis',(2.54229873860636E-12,0.999390827019096,0.0348994967024795));
#46621=DIRECTION('',(1.,6.76186946307289E-14,-2.76820162751211E-15));
#46622=DIRECTION('center_axis',(3.92980782396055E-15,-0.0348994967025042,
0.999390827019096));
#46623=DIRECTION('ref_axis',(1.41395947801337E-12,0.999390827019096,0.0348994967025042));
#46624=DIRECTION('',(1.,6.76186946307289E-14,-2.76820162751211E-15));
#46625=DIRECTION('',(0.0174417781380274,0.999238800303652,0.0348941878126054));
#46626=DIRECTION('',(0.713036894919998,0.70069940513849,0.0244689624098382));
#46627=DIRECTION('',(1.,6.76186946307289E-14,-2.76820162751211E-15));
#46628=DIRECTION('',(-6.74808943053847E-14,0.999390827019096,0.0348994967024838));
#46629=DIRECTION('center_axis',(-1.,-6.76186946307289E-14,2.76820162751211E-15));
#46630=DIRECTION('ref_axis',(6.76186946307289E-14,-1.,8.61946552381525E-15));
#46631=DIRECTION('',(-1.,-6.76186946307289E-14,2.76820162751211E-15));
#46632=DIRECTION('center_axis',(1.,6.76186946307289E-14,-2.53239663548226E-15));
#46633=DIRECTION('ref_axis',(6.76186946307289E-14,-1.,1.05059054600541E-14));
#46634=DIRECTION('center_axis',(1.,6.76186946307289E-14,-2.53239663548226E-15));
#46635=DIRECTION('ref_axis',(6.76186946307289E-14,-1.,1.05059054600541E-14));
#46636=DIRECTION('center_axis',(5.03724005550908E-14,-0.719339800338648,
0.694658370459));
#46637=DIRECTION('ref_axis',(-4.49806146187152E-14,0.694658370459,0.719339800338648));
#46638=DIRECTION('',(-4.49806146187149E-14,0.694658370458996,0.719339800338652));
#46639=DIRECTION('',(1.,6.76186946307289E-14,-2.76820162751211E-15));
#46640=DIRECTION('center_axis',(-4.67178638631599E-14,0.71933980033866,
0.694658370458988));
#46641=DIRECTION('ref_axis',(-4.89631698307778E-14,0.694658370458988,-0.71933980033866));
#46642=DIRECTION('',(-4.8963169830778E-14,0.694658370458991,-0.719339800338657));
#46643=DIRECTION('',(1.,6.76186946307289E-14,-2.76820162751211E-15));
#46644=DIRECTION('center_axis',(-1.,-6.76186946307289E-14,2.76820162751211E-15));
#46645=DIRECTION('ref_axis',(6.76186946307289E-14,-1.,8.61946552381525E-15));
#46646=DIRECTION('',(-1.,-6.76186946307289E-14,2.76820162751211E-15));
#46647=DIRECTION('center_axis',(1.,6.76186946307289E-14,-2.53239663548226E-15));
#46648=DIRECTION('ref_axis',(6.76186946307289E-14,-1.,-2.69917409361775E-15));
#46649=DIRECTION('center_axis',(1.,6.76186946307289E-14,-2.53239663548226E-15));
#46650=DIRECTION('ref_axis',(6.76186946307289E-14,-1.,-2.69917409361775E-15));
#46651=DIRECTION('center_axis',(4.06656903581742E-16,0.0348994967025106,
0.999390827019095));
#46652=DIRECTION('ref_axis',(-6.76741119925271E-14,0.999390827019096,-0.0348994967025106));
#46653=DIRECTION('',(-6.7674111992527E-14,0.999390827019096,-0.0348994967025031));
#46654=DIRECTION('',(-1.,-6.76186946307289E-14,2.76820162751211E-15));
#46655=DIRECTION('',(-0.713036894920085,0.700699405138401,-0.0244689624098501));
#46656=DIRECTION('',(-0.0174417781381626,0.999238800303649,-0.0348941878126222));
#46657=DIRECTION('center_axis',(-9.8008354509373E-16,0.0348994967025452,
0.999390827019094));
#46658=DIRECTION('ref_axis',(-1.55020631512074E-12,-0.999390827019094,0.0348994967025452));
#46659=DIRECTION('center_axis',(3.48081291315565E-15,0.034899496702521,
0.999390827019095));
#46660=DIRECTION('ref_axis',(-4.33836829016131E-13,-0.999390827019095,0.034899496702521));
#46661=DIRECTION('center_axis',(6.76186946307289E-14,-1.,8.61946552381525E-15));
#46662=DIRECTION('ref_axis',(2.76820162751153E-15,8.61946552381544E-15,
1.));
#46663=DIRECTION('',(2.76820162751153E-15,8.61946552381544E-15,1.));
#46664=DIRECTION('center_axis',(6.42420170581153E-14,-1.,8.11391641182261E-15));
#46665=DIRECTION('ref_axis',(0.664254779227899,4.87382700579703E-14,0.747506246310287));
#46666=DIRECTION('',(2.76820162751153E-15,8.61946552381544E-15,1.));
#46667=DIRECTION('',(1.,6.76186946307289E-14,-2.76820162751211E-15));
#46668=DIRECTION('',(0.70710678118654,4.17187549862768E-14,-0.707106781186555));
#46669=DIRECTION('',(-2.76820162751153E-15,-8.61946552381544E-15,-1.));
#46670=DIRECTION('',(-0.707106781186549,-5.39085200304643E-14,-0.707106781186546));
#46671=DIRECTION('',(-1.,-6.76186946307289E-14,2.76820162751211E-15));
#46672=DIRECTION('',(-0.707106781186546,-4.17187549862773E-14,0.707106781186549));
#46673=DIRECTION('',(2.76820162751153E-15,8.61946552381544E-15,1.));
#46674=DIRECTION('',(0.707106781186549,5.39085200304643E-14,0.707106781186546));
#46675=DIRECTION('center_axis',(2.76820162751153E-15,8.61946552381544E-15,
1.));
#46676=DIRECTION('ref_axis',(-6.76186946307289E-14,1.,-8.61946552381525E-15));
#46677=DIRECTION('center_axis',(-5.20004799022464E-15,-4.34637833531572E-15,
-1.));
#46678=DIRECTION('ref_axis',(-6.57727994239961E-14,1.,-4.34637833531538E-15));
#46679=DIRECTION('',(2.76820162751153E-15,8.61946552381544E-15,1.));
#46680=DIRECTION('center_axis',(-2.15290322526726E-15,-8.6194655238154E-15,
-1.));
#46681=DIRECTION('ref_axis',(-6.82339930329732E-14,1.,-8.61946552381525E-15));
#46682=DIRECTION('center_axis',(-2.15290322526726E-15,-8.6194655238154E-15,
-1.));
#46683=DIRECTION('ref_axis',(-6.82339930329732E-14,1.,-8.61946552381525E-15));
#46684=DIRECTION('center_axis',(-5.20004799022464E-15,-4.34637833531572E-15,
-1.));
#46685=DIRECTION('ref_axis',(-6.57727994239961E-14,1.,-4.34637833531538E-15));
#46686=DIRECTION('',(-2.76820162751153E-15,-8.61946552381544E-15,-1.));
#46687=DIRECTION('center_axis',(5.12637372416674E-15,-0.0348994967024901,
0.999390827019096));
#46688=DIRECTION('ref_axis',(-6.74808943053847E-14,0.999390827019096,0.0348994967024901));
#46689=DIRECTION('center_axis',(4.06656903581789E-16,0.0348994967025099,
0.999390827019095));
#46690=DIRECTION('ref_axis',(-6.7674111992527E-14,0.999390827019095,-0.0348994967025099));
#46691=DIRECTION('',(2.76820162751153E-15,8.61946552381544E-15,1.));
#46692=DIRECTION('center_axis',(-2.76820162751153E-15,-8.61946552381544E-15,
-1.));
#46693=DIRECTION('ref_axis',(6.76186946307289E-14,-1.,8.61946552381525E-15));
#46694=DIRECTION('center_axis',(-3.27006405595157E-15,2.95336814164933E-15,
1.));
#46695=DIRECTION('ref_axis',(7.06970933615109E-14,-1.,2.95336814164956E-15));
#46696=DIRECTION('',(2.76820162751153E-15,8.61946552381544E-15,1.));
#46697=DIRECTION('center_axis',(-2.76820162751153E-15,-8.61946552381544E-15,
-1.));
#46698=DIRECTION('ref_axis',(-6.88500541230417E-14,1.,-8.61946552381525E-15));
#46699=DIRECTION('center_axis',(-3.27006405595157E-15,2.95336814164933E-15,
1.));
#46700=DIRECTION('ref_axis',(7.06970933615109E-14,-1.,2.95336814164956E-15));
#46701=DIRECTION('',(-2.76820162751153E-15,-8.61946552381544E-15,-1.));
#46702=DIRECTION('center_axis',(-4.06656903581438E-16,-0.0348994967025151,
-0.999390827019095));
#46703=DIRECTION('ref_axis',(6.7674111992527E-14,-0.999390827019095,0.0348994967025151));
#46704=DIRECTION('center_axis',(-5.12637372416635E-15,0.0348994967024843,
-0.999390827019096));
#46705=DIRECTION('ref_axis',(6.74808943053847E-14,-0.999390827019096,-0.0348994967024843));
#46706=DIRECTION('',(2.76820162751153E-15,8.61946552381544E-15,1.));
#46707=DIRECTION('center_axis',(-4.06656903581438E-16,-0.0348994967025151,
-0.999390827019095));
#46708=DIRECTION('ref_axis',(6.7674111992527E-14,-0.999390827019095,0.0348994967025151));
#46709=DIRECTION('',(-6.7674111992527E-14,0.999390827019096,-0.0348994967025004));
#46710=DIRECTION('',(-1.,-6.76186946307289E-14,2.76820162751211E-15));
#46711=DIRECTION('center_axis',(-5.12637372416635E-15,0.0348994967024843,
-0.999390827019096));
#46712=DIRECTION('ref_axis',(6.74808943053847E-14,-0.999390827019096,-0.0348994967024843));
#46713=DIRECTION('',(-6.74808943053847E-14,0.999390827019096,0.0348994967024933));
#46714=DIRECTION('center_axis',(0.500000000000092,4.12740234260384E-14,
0.866025403784385));
#46715=DIRECTION('ref_axis',(-6.76186946307289E-14,1.,-8.61946552381525E-15));
#46716=DIRECTION('',(0.866025403784435,5.42497745590457E-14,-0.500000000000006));
#46717=DIRECTION('',(6.76186946307289E-14,-1.,8.61946552381525E-15));
#46718=DIRECTION('',(0.866025403784435,5.42497745590457E-14,-0.500000000000006));
#46719=DIRECTION('',(6.76186946307289E-14,-1.,8.61946552381525E-15));
#46720=DIRECTION('center_axis',(1.,6.76186946307289E-14,-2.76820162751211E-15));
#46721=DIRECTION('ref_axis',(-6.76186946307289E-14,1.,-8.61946552381525E-15));
#46722=DIRECTION('',(-2.76820162751153E-15,-8.61946552381544E-15,-1.));
#46723=DIRECTION('',(6.76186946307289E-14,-1.,8.61946552381525E-15));
#46724=DIRECTION('',(-2.76820162751153E-15,-8.61946552381544E-15,-1.));
#46725=DIRECTION('center_axis',(0.500000000000088,2.63446712047027E-14,
-0.866025403784388));
#46726=DIRECTION('ref_axis',(6.76186946307289E-14,-1.,8.61946552381525E-15));
#46727=DIRECTION('',(-0.866025403784438,-6.28692400828612E-14,-0.500000000000002));
#46728=DIRECTION('',(6.76186946307289E-14,-1.,8.61946552381525E-15));
#46729=DIRECTION('',(-0.866025403784438,-6.28692400828612E-14,-0.500000000000002));
#46730=DIRECTION('center_axis',(2.76820162751153E-15,8.61946552381544E-15,
1.));
#46731=DIRECTION('ref_axis',(-6.76186946307289E-14,1.,-8.61946552381525E-15));
#46732=DIRECTION('',(-6.76186946307289E-14,1.,-8.61946552381525E-15));
#46733=DIRECTION('center_axis',(6.59733936268404E-14,-4.45999109629057E-16,
1.));
#46734=DIRECTION('ref_axis',(1.,5.89801867114909E-14,-6.59733936268404E-14));
#46735=DIRECTION('center_axis',(3.08914665434315E-15,8.61946552381546E-15,
1.));
#46736=DIRECTION('ref_axis',(-0.979681390452711,0.200560148585511,1.29765820345512E-15));
#46737=DIRECTION('center_axis',(-2.76820162751153E-15,-8.61946552381544E-15,
-1.));
#46738=DIRECTION('ref_axis',(6.76186946307289E-14,-1.,8.61946552381525E-15));
#46739=DIRECTION('',(6.76186946307289E-14,-1.,8.61946552381525E-15));
#46740=DIRECTION('center_axis',(3.58207973448846E-15,8.61946552381549E-15,
1.));
#46741=DIRECTION('ref_axis',(6.76186946307289E-14,-1.,8.61946552381525E-15));
#46742=DIRECTION('center_axis',(-1.,-6.76186946307289E-14,2.76820162751211E-15));
#46743=DIRECTION('ref_axis',(6.76186946307289E-14,-1.,8.61946552381525E-15));
#46744=DIRECTION('center_axis',(1.,6.76186946307288E-14,-6.54108149998981E-15));
#46745=DIRECTION('ref_axis',(6.7618694630729E-14,-1.,1.80516652050094E-14));
#46746=DIRECTION('center_axis',(1.,6.76186946307288E-14,-6.54108149998981E-15));
#46747=DIRECTION('ref_axis',(6.7618694630729E-14,-1.,1.80516652050094E-14));
#46748=DIRECTION('',(-1.,-6.76186946307289E-14,2.76820162751211E-15));
#46749=DIRECTION('center_axis',(1.,6.57782599518977E-14,-2.17856824283608E-15));
#46750=DIRECTION('ref_axis',(5.47980452554462E-14,-0.813826036051068,0.581108581114929));
#46751=DIRECTION('center_axis',(-1.,-6.76186946307289E-14,2.76820162751211E-15));
#46752=DIRECTION('ref_axis',(6.76186946307289E-14,-1.,8.61946552381525E-15));
#46753=DIRECTION('center_axis',(1.,6.76186946307288E-14,-6.54108149998976E-15));
#46754=DIRECTION('ref_axis',(6.76186946307289E-14,-1.,4.84658565133759E-15));
#46755=DIRECTION('center_axis',(1.,6.76186946307288E-14,-6.54108149998976E-15));
#46756=DIRECTION('ref_axis',(6.76186946307289E-14,-1.,4.84658565133759E-15));
#46757=DIRECTION('',(-1.,-6.76186946307289E-14,2.76820162751211E-15));
#46758=DIRECTION('center_axis',(1.,6.48270906338569E-14,-2.13515025569885E-14));
#46759=DIRECTION('ref_axis',(6.51655155548385E-14,-0.813826036051071,0.581108581114924));
#46760=DIRECTION('center_axis',(-1.,-6.76186946307289E-14,2.76820162751211E-15));
#46761=DIRECTION('ref_axis',(6.76186946307289E-14,-1.,8.61946552381525E-15));
#46762=DIRECTION('center_axis',(1.,6.76186946307288E-14,-6.54108149998976E-15));
#46763=DIRECTION('ref_axis',(6.76186946307289E-14,-1.,6.73302558757642E-15));
#46764=DIRECTION('center_axis',(1.,6.76186946307288E-14,-6.54108149998976E-15));
#46765=DIRECTION('ref_axis',(6.76186946307289E-14,-1.,6.73302558757642E-15));
#46766=DIRECTION('',(-1.,-6.76186946307289E-14,2.76820162751211E-15));
#46767=DIRECTION('center_axis',(1.,6.57576252994809E-14,-1.51570689138297E-14));
#46768=DIRECTION('ref_axis',(6.23231703479847E-14,-0.813826036051068,0.581108581114929));
#46769=DIRECTION('center_axis',(-1.,-6.76186946307289E-14,2.76820162751211E-15));
#46770=DIRECTION('ref_axis',(6.76186946307289E-14,-1.,8.61946552381525E-15));
#46771=DIRECTION('center_axis',(1.,6.76186946307288E-14,-6.54108149998981E-15));
#46772=DIRECTION('ref_axis',(6.7618694630729E-14,-1.,1.80516652050094E-14));
#46773=DIRECTION('center_axis',(1.,6.76186946307288E-14,-6.54108149998981E-15));
#46774=DIRECTION('ref_axis',(6.7618694630729E-14,-1.,1.80516652050094E-14));
#46775=DIRECTION('',(-1.,-6.76186946307289E-14,2.76820162751211E-15));
#46776=DIRECTION('center_axis',(1.,6.94384946571432E-14,-1.63363356831818E-14));
#46777=DIRECTION('ref_axis',(6.60040397056471E-14,-0.813826036051069,0.581108581114927));
#46778=DIRECTION('center_axis',(-1.,-6.76186946307289E-14,2.76820162751211E-15));
#46779=DIRECTION('ref_axis',(6.76186946307289E-14,-1.,8.61946552381525E-15));
#46780=DIRECTION('center_axis',(-4.06656903581789E-16,-0.0348994967025099,
-0.999390827019095));
#46781=DIRECTION('ref_axis',(6.7674111992527E-14,-0.999390827019096,0.0348994967025099));
#46782=DIRECTION('',(-1.,-6.76186946307289E-14,2.76820162751211E-15));
#46783=DIRECTION('',(-0.0174417781380384,-0.999238800303652,0.0348941878126222));
#46784=DIRECTION('',(-0.713036894919993,-0.700699405138495,0.0244689624098544));
#46785=DIRECTION('',(-1.,-6.76186946307289E-14,2.76820162751211E-15));
#46786=DIRECTION('',(-6.76741119925271E-14,0.999390827019096,-0.0348994967025096));
#46787=DIRECTION('center_axis',(-5.12637372416674E-15,0.0348994967024901,
-0.999390827019096));
#46788=DIRECTION('ref_axis',(6.74808943053847E-14,-0.999390827019096,-0.0348994967024901));
#46789=DIRECTION('',(-6.74808943053847E-14,0.999390827019096,0.0348994967024924));
#46790=DIRECTION('',(1.,6.76186946307289E-14,-2.76820162751211E-15));
#46791=DIRECTION('',(0.713036894920087,-0.700699405138399,-0.0244689624098423));
#46792=DIRECTION('',(0.0174417781381465,-0.99923880030365,-0.034894187812605));
#46793=DIRECTION('center_axis',(-6.76186946307289E-14,1.,-8.61946552381525E-15));
#46794=DIRECTION('ref_axis',(-2.76820162751153E-15,-8.61946552381544E-15,
-1.));
#46795=DIRECTION('',(2.76820162751153E-15,8.61946552381544E-15,1.));
#46796=DIRECTION('center_axis',(7.38750159181778E-14,-1.,1.0997592254033E-14));
#46797=DIRECTION('ref_axis',(0.664254779227879,4.08510634849217E-14,-0.747506246310305));
#46798=DIRECTION('center_axis',(7.38750159181778E-14,-1.,1.0997592254033E-14));
#46799=DIRECTION('ref_axis',(0.664254779227879,4.08510634849217E-14,-0.747506246310305));
#46800=DIRECTION('',(0.866025403784436,6.28692400828612E-14,0.500000000000004));
#46801=DIRECTION('',(2.76820162751153E-15,8.61946552381544E-15,1.));
#46802=DIRECTION('',(-0.866025403784434,-5.42497745590456E-14,0.500000000000009));
#46803=DIRECTION('center_axis',(-6.76186946307289E-14,1.,-8.61946552381525E-15));
#46804=DIRECTION('ref_axis',(-2.76820162751153E-15,-8.61946552381544E-15,
-1.));
#46805=DIRECTION('',(-2.76820162751153E-15,-8.61946552381544E-15,-1.));
#46806=DIRECTION('',(-1.,-6.76186946307289E-14,2.76820162751211E-15));
#46807=DIRECTION('center_axis',(-6.76186946307289E-14,1.,-8.61946552381525E-15));
#46808=DIRECTION('ref_axis',(0.973373605804438,6.77940443873129E-14,0.229224395567456));
#46809=DIRECTION('',(1.,6.76186946307289E-14,-2.76820162751211E-15));
#46810=DIRECTION('center_axis',(6.59789806251287E-14,-1.,8.3132822970341E-15));
#46811=DIRECTION('ref_axis',(-1.,-6.59789806251287E-14,2.7682016275121E-15));
#46812=DIRECTION('center_axis',(6.72378933645552E-14,-1.,1.14586580466301E-14));
#46813=DIRECTION('ref_axis',(-0.813826036051072,-4.80612237103423E-14,0.581108581114923));
#46814=DIRECTION('',(-6.59789806251287E-14,1.,-8.3132822970341E-15));
#46815=DIRECTION('center_axis',(-6.74261350511498E-14,1.,-8.55777381697828E-15));
#46816=DIRECTION('ref_axis',(-0.813826036051075,-5.98461400152083E-14,-0.58110858111492));
#46817=DIRECTION('center_axis',(6.76186946307289E-14,-1.,8.61946552381525E-15));
#46818=DIRECTION('ref_axis',(2.76820162751153E-15,8.61946552381544E-15,
1.));
#46819=DIRECTION('center_axis',(0.86602540378444,5.42497745590461E-14,-0.499999999999998));
#46820=DIRECTION('ref_axis',(-6.76186946307289E-14,1.,-8.61946552381525E-15));
#46821=DIRECTION('',(0.500000000000023,4.1274023426034E-14,0.866025403784425));
#46822=DIRECTION('',(6.76186946307289E-14,-1.,8.61946552381525E-15));
#46823=DIRECTION('',(0.500000000000005,4.12740234260329E-14,0.866025403784436));
#46824=DIRECTION('',(6.76186946307289E-14,-1.,8.61946552381525E-15));
#46825=DIRECTION('center_axis',(-2.76820162751153E-15,-8.61946552381544E-15,
-1.));
#46826=DIRECTION('ref_axis',(6.76186946307289E-14,-1.,8.61946552381525E-15));
#46827=DIRECTION('',(1.,6.76186946307289E-14,-2.76820162751211E-15));
#46828=DIRECTION('',(1.,6.76186946307289E-14,-2.76820162751211E-15));
#46829=DIRECTION('',(6.76186946307289E-14,-1.,8.61946552381525E-15));
#46830=DIRECTION('center_axis',(-0.86602540378444,-6.28692400828613E-14,
-0.499999999999998));
#46831=DIRECTION('ref_axis',(6.76186946307289E-14,-1.,8.61946552381525E-15));
#46832=DIRECTION('',(0.500000000000008,2.63446712046968E-14,-0.866025403784434));
#46833=DIRECTION('',(0.499999999999997,2.63446712046961E-14,-0.86602540378444));
#46834=DIRECTION('',(6.76186946307289E-14,-1.,8.61946552381525E-15));
#46835=DIRECTION('center_axis',(-0.866025403784437,-5.42497745590459E-14,
0.500000000000003));
#46836=DIRECTION('ref_axis',(-6.76186946307289E-14,1.,-8.61946552381525E-15));
#46837=DIRECTION('',(-0.500000000000012,-4.12740234260334E-14,-0.866025403784431));
#46838=DIRECTION('',(-0.500000000000003,-4.12740234260328E-14,-0.866025403784437));
#46839=DIRECTION('',(6.76186946307289E-14,-1.,8.61946552381525E-15));
#46840=DIRECTION('center_axis',(4.50475380710499E-14,-1.,4.08063979811324E-14));
#46841=DIRECTION('ref_axis',(-0.218698251317282,2.99667608013125E-14,0.975792536798044));
#46842=DIRECTION('center_axis',(8.99762615155132E-14,-1.,-3.01049762542494E-14));
#46843=DIRECTION('ref_axis',(-0.783876701585605,-8.92229719919495E-14,0.620916513479286));
#46844=DIRECTION('center_axis',(1.6283363940689E-13,-1.,6.3627469085968E-15));
#46845=DIRECTION('ref_axis',(-0.954410251348989,-1.53510827315915E-13,0.298498026995086));
#46846=DIRECTION('center_axis',(6.76186946307289E-14,-1.,8.61946552381525E-15));
#46847=DIRECTION('ref_axis',(-0.929667825095141,-6.60383262206062E-14,-0.368398880268208));
#46848=DIRECTION('center_axis',(1.01926724028163E-13,-1.,4.4055959896663E-14));
#46849=DIRECTION('ref_axis',(0.735712000031743,1.04827573753555E-13,0.677294509803005));
#46850=DIRECTION('center_axis',(4.52611277459444E-14,-1.,-3.01049762542494E-14));
#46851=DIRECTION('ref_axis',(0.145791123509555,-2.31846457713419E-14,0.989315393747526));
#46852=DIRECTION('center_axis',(-3.59257197464621E-14,-1.,1.00257629324988E-14));
#46853=DIRECTION('ref_axis',(0.954410251348985,-3.72805456675856E-14,-0.298498026995101));
#46854=DIRECTION('center_axis',(6.76186946307289E-14,-1.,8.61946552381525E-15));
#46855=DIRECTION('ref_axis',(0.929667825095138,6.60383262206061E-14,0.368398880268216));
#46856=DIRECTION('center_axis',(-5.66109027953888E-14,-1.,1.00181373700227E-13));
#46857=DIRECTION('ref_axis',(0.218698251317116,-1.10136942229696E-13,-0.975792536798082));
#46858=DIRECTION('center_axis',(8.99762615155134E-14,-1.,-3.01049762542516E-14));
#46859=DIRECTION('ref_axis',(0.783876701585584,8.922297199195E-14,-0.620916513479312));
#46860=DIRECTION('center_axis',(0.866025403784441,6.28692400828614E-14,
0.499999999999996));
#46861=DIRECTION('ref_axis',(-6.76186946307289E-14,1.,-8.61946552381525E-15));
#46862=DIRECTION('',(-0.500000000000018,-2.63446712046976E-14,0.866025403784428));
#46863=DIRECTION('',(6.76186946307289E-14,-1.,8.61946552381525E-15));
#46864=DIRECTION('',(-0.499999999999999,-2.63446712046962E-14,0.866025403784439));
#46865=DIRECTION('center_axis',(2.76820162751153E-15,8.61946552381544E-15,
1.));
#46866=DIRECTION('ref_axis',(-6.76186946307289E-14,1.,-8.61946552381525E-15));
#46867=DIRECTION('',(-1.,-6.76186946307289E-14,2.76820162751211E-15));
#46868=DIRECTION('',(-1.,-6.76186946307289E-14,2.76820162751211E-15));
#46869=DIRECTION('center_axis',(3.81897507906258E-14,-1.,-3.71109083284009E-14));
#46870=DIRECTION('ref_axis',(-0.735712000031729,-2.96164347025554E-15,-0.67729450980302));
#46871=DIRECTION('center_axis',(4.52611277459447E-14,-1.,-3.01049762542507E-14));
#46872=DIRECTION('ref_axis',(-0.145791123509541,2.31846457713439E-14,-0.989315393747528));
#46873=DIRECTION('center_axis',(-6.76186946307289E-14,1.,-8.61946552381525E-15));
#46874=DIRECTION('ref_axis',(-2.76820162751153E-15,-8.61946552381544E-15,
-1.));
#46875=DIRECTION('center_axis',(0.866025403784432,5.42497745590455E-14,
-0.500000000000011));
#46876=DIRECTION('ref_axis',(6.76186946307289E-14,-1.,8.61946552381525E-15));
#46877=DIRECTION('',(0.499999999999968,4.12740234260306E-14,0.866025403784457));
#46878=DIRECTION('',(6.76186946307289E-14,-1.,8.61946552381525E-15));
#46879=DIRECTION('',(0.5,4.12740234260326E-14,0.866025403784438));
#46880=DIRECTION('',(6.76186946307289E-14,-1.,8.61946552381525E-15));
#46881=DIRECTION('center_axis',(-2.76820162751153E-15,-8.61946552381544E-15,
-1.));
#46882=DIRECTION('ref_axis',(6.76186946307289E-14,-1.,8.61946552381525E-15));
#46883=DIRECTION('',(1.,6.76186946307289E-14,-2.76820162751211E-15));
#46884=DIRECTION('',(1.,6.76186946307289E-14,-2.76820162751211E-15));
#46885=DIRECTION('',(6.76186946307289E-14,-1.,8.61946552381525E-15));
#46886=DIRECTION('center_axis',(-0.866025403784448,-6.28692400828618E-14,
-0.499999999999984));
#46887=DIRECTION('ref_axis',(6.76186946307289E-14,-1.,8.61946552381525E-15));
#46888=DIRECTION('',(0.499999999999689,2.63446712046737E-14,-0.866025403784618));
#46889=DIRECTION('',(0.499999999999926,2.63446712046909E-14,-0.866025403784482));
#46890=DIRECTION('',(6.76186946307289E-14,-1.,8.61946552381525E-15));
#46891=DIRECTION('center_axis',(-0.866025403784445,-5.42497745590466E-14,
0.499999999999988));
#46892=DIRECTION('ref_axis',(6.76186946307289E-14,-1.,8.61946552381525E-15));
#46893=DIRECTION('',(-0.499999999999693,-4.12740234260134E-14,-0.866025403784616));
#46894=DIRECTION('',(-0.499999999999929,-4.12740234260282E-14,-0.866025403784479));
#46895=DIRECTION('',(6.76186946307289E-14,-1.,8.61946552381525E-15));
#46896=DIRECTION('center_axis',(-2.89017677254347E-14,-1.,-4.80410785544967E-13));
#46897=DIRECTION('ref_axis',(-0.218698251317561,-4.62460493070496E-13,0.975792536797982));
#46898=DIRECTION('center_axis',(6.76186946307289E-14,-1.,8.61946552381525E-15));
#46899=DIRECTION('ref_axis',(-0.78387670158548,-4.76527508315479E-14,0.620916513479444));
#46900=DIRECTION('center_axis',(5.90197180282114E-13,-1.,8.61724231507531E-15));
#46901=DIRECTION('ref_axis',(-0.954410251348957,-5.60718009349308E-13,0.29849802699519));
#46902=DIRECTION('center_axis',(6.76186946307289E-14,-1.,8.61946552381525E-15));
#46903=DIRECTION('ref_axis',(-0.929667825095052,-6.60383262206021E-14,-0.368398880268433));
#46904=DIRECTION('center_axis',(2.6777905538118E-13,-1.,2.85289344946059E-13));
#46905=DIRECTION('ref_axis',(0.735712000031681,3.90233171438362E-13,0.677294509803073));
#46906=DIRECTION('center_axis',(6.76186946307289E-14,-1.,8.61946552381525E-15));
#46907=DIRECTION('ref_axis',(0.145791123509563,1.83855753890505E-14,0.989315393747524));
#46908=DIRECTION('center_axis',(-3.756532448168E-13,-1.,8.55192630619435E-15));
#46909=DIRECTION('ref_axis',(0.95441025134894,-3.61080040935055E-13,-0.298498026995244));
#46910=DIRECTION('center_axis',(6.76186946307289E-14,-1.,8.61946552381525E-15));
#46911=DIRECTION('ref_axis',(0.929667825095137,6.6038326220606E-14,0.368398880268219));
#46912=DIRECTION('center_axis',(1.00002048887206E-13,-1.,-1.99696937105634E-15));
#46913=DIRECTION('ref_axis',(0.218698251317296,2.38189010282698E-14,-0.975792536798041));
#46914=DIRECTION('center_axis',(6.76186946307289E-14,-1.,8.61946552381525E-15));
#46915=DIRECTION('ref_axis',(0.783876701585569,4.76527508315549E-14,-0.620916513479332));
#46916=DIRECTION('center_axis',(0.866025403784435,6.28692400828611E-14,
0.500000000000006));
#46917=DIRECTION('ref_axis',(-6.76186946307289E-14,1.,-8.61946552381525E-15));
#46918=DIRECTION('',(-0.499999999999964,-2.63446712046937E-14,0.86602540378446));
#46919=DIRECTION('',(6.76186946307289E-14,-1.,8.61946552381525E-15));
#46920=DIRECTION('',(-0.499999999999995,-2.63446712046959E-14,0.866025403784442));
#46921=DIRECTION('center_axis',(2.76820162751153E-15,8.61946552381544E-15,
1.));
#46922=DIRECTION('ref_axis',(-6.76186946307289E-14,1.,-8.61946552381525E-15));
#46923=DIRECTION('',(-1.,-6.76186946307289E-14,2.76820162751211E-15));
#46924=DIRECTION('',(-1.,-6.76186946307289E-14,2.76820162751211E-15));
#46925=DIRECTION('center_axis',(-5.10570936524672E-13,-1.,-3.40477006188309E-13));
#46926=DIRECTION('ref_axis',(-0.735712000031916,6.06236371874177E-13,-0.677294509802817));
#46927=DIRECTION('center_axis',(6.76186946307289E-14,-1.,8.61946552381525E-15));
#46928=DIRECTION('ref_axis',(-0.145791123509724,-1.83855753890612E-14,-0.989315393747501));
#46929=DIRECTION('center_axis',(-6.76186946307289E-14,1.,-8.61946552381525E-15));
#46930=DIRECTION('ref_axis',(-2.76820162751153E-15,-8.61946552381544E-15,
-1.));
#46931=DIRECTION('center_axis',(-0.707106781186558,-5.39085200304648E-14,
-0.707106781186537));
#46932=DIRECTION('ref_axis',(6.76186946307289E-14,-1.,8.61946552381525E-15));
#46933=DIRECTION('',(0.707106781186545,4.17187549862772E-14,-0.70710678118655));
#46934=DIRECTION('',(-6.76186946307289E-14,1.,-8.61946552381525E-15));
#46935=DIRECTION('center_axis',(-1.,-6.76186946307289E-14,2.76820162751211E-15));
#46936=DIRECTION('ref_axis',(6.76186946307289E-14,-1.,8.61946552381525E-15));
#46937=DIRECTION('',(-6.76186946307289E-14,1.,-8.61946552381525E-15));
#46938=DIRECTION('',(-6.76186946307289E-14,1.,-8.61946552381525E-15));
#46939=DIRECTION('',(-2.76820162751153E-15,-8.61946552381544E-15,-1.));
#46940=DIRECTION('center_axis',(-0.707106781186553,-4.17187549862778E-14,
0.707106781186542));
#46941=DIRECTION('ref_axis',(-6.76186946307289E-14,1.,-8.61946552381525E-15));
#46942=DIRECTION('',(-6.76186946307289E-14,1.,-8.61946552381525E-15));
#46943=DIRECTION('',(-0.707106781186549,-5.39085200304643E-14,-0.707106781186546));
#46944=DIRECTION('center_axis',(2.76820162751153E-15,8.61946552381544E-15,
1.));
#46945=DIRECTION('ref_axis',(-6.76186946307289E-14,1.,-8.61946552381525E-15));
#46946=DIRECTION('',(-6.76186946307289E-14,1.,-8.61946552381525E-15));
#46947=DIRECTION('',(-1.,-6.76186946307289E-14,2.76820162751211E-15));
#46948=DIRECTION('center_axis',(0.707106781186549,5.39085200304643E-14,
0.707106781186546));
#46949=DIRECTION('ref_axis',(-6.76186946307289E-14,1.,-8.61946552381525E-15));
#46950=DIRECTION('',(-6.76186946307289E-14,1.,-8.61946552381525E-15));
#46951=DIRECTION('',(-0.707106781186546,-4.17187549862773E-14,0.707106781186549));
#46952=DIRECTION('center_axis',(1.,6.76186946307289E-14,-2.76820162751211E-15));
#46953=DIRECTION('ref_axis',(-6.76186946307289E-14,1.,-8.61946552381525E-15));
#46954=DIRECTION('',(-6.76186946307289E-14,1.,-8.61946552381525E-15));
#46955=DIRECTION('',(2.76820162751153E-15,8.61946552381544E-15,1.));
#46956=DIRECTION('center_axis',(0.707106781186547,4.17187549862773E-14,
-0.707106781186548));
#46957=DIRECTION('ref_axis',(6.76186946307289E-14,-1.,8.61946552381525E-15));
#46958=DIRECTION('',(0.70710678118655,5.39085200304644E-14,0.707106781186545));
#46959=DIRECTION('center_axis',(4.671786386316E-14,-0.719339800338662,-0.694658370458986));
#46960=DIRECTION('ref_axis',(4.89631698307776E-14,-0.694658370458986,0.719339800338662));
#46961=DIRECTION('center_axis',(2.74445416328055E-14,-0.719339800338663,
-0.694658370458985));
#46962=DIRECTION('ref_axis',(-4.40030170723143E-14,-0.694658370458985,0.719339800338663));
#46963=DIRECTION('',(4.89631698307777E-14,-0.694658370458988,0.719339800338661));
#46964=DIRECTION('center_axis',(-5.05637727264981E-14,0.719339800338649,
-0.694658370458999));
#46965=DIRECTION('ref_axis',(4.49806146187151E-14,-0.694658370458999,-0.719339800338649));
#46966=DIRECTION('',(4.49806146187153E-14,-0.694658370459002,-0.719339800338646));
#46967=DIRECTION('center_axis',(-6.62058893192496E-14,0.719339800338649,
-0.694658370458999));
#46968=DIRECTION('ref_axis',(-1.53038824229755E-13,0.694658370458999,0.719339800338649));
#46969=DIRECTION('center_axis',(-2.80868565487176E-15,-1.41842548064666E-14,
-1.));
#46970=DIRECTION('ref_axis',(-0.725826090825681,-0.687878249312123,1.17956576933031E-14));
#46971=DIRECTION('center_axis',(-6.72195880142588E-14,6.28549570584167E-14,
-1.));
#46972=DIRECTION('ref_axis',(-7.55372801463421E-14,1.,6.28549570584218E-14));
#46973=DIRECTION('center_axis',(-2.76820162751178E-15,-6.59025840835834E-15,
-1.));
#46974=DIRECTION('ref_axis',(0.723116678427596,-0.690725900325043,2.55032940638382E-15));
#46975=DIRECTION('center_axis',(2.93997442168891E-14,-8.30723103291069E-13,
-1.));
#46976=DIRECTION('ref_axis',(-0.60420794012745,0.796826684472191,-6.79705895003432E-13));
#46977=DIRECTION('center_axis',(-2.76820162751272E-15,2.47371373313956E-15,
-1.));
#46978=DIRECTION('ref_axis',(0.723116678427503,0.69072590032514,-2.93074620635121E-16));
#46979=DIRECTION('center_axis',(2.76820162751153E-15,8.61946552381544E-15,
1.));
#46980=DIRECTION('ref_axis',(-6.76186946307289E-14,1.,-8.61946552381525E-15));
#46981=DIRECTION('',(6.76186946307289E-14,-1.,8.61946552381525E-15));
#46982=DIRECTION('',(0.86602540378447,-0.499999999999946,1.91239982968476E-15));
#46983=DIRECTION('',(0.866025403784402,0.500000000000063,-6.70706569413058E-15));
#46984=DIRECTION('',(-6.76186946307289E-14,1.,-8.61946552381525E-15));
#46985=DIRECTION('',(-0.866025403784484,0.499999999999922,-1.9123998296845E-15));
#46986=DIRECTION('',(-0.866025403784416,-0.500000000000039,6.7070656941304E-15));
#46987=DIRECTION('center_axis',(0.500000000000052,-0.866025403784409,6.08057529691215E-15));
#46988=DIRECTION('ref_axis',(2.76820162751153E-15,8.61946552381544E-15,
1.));
#46989=DIRECTION('',(-0.866025403784416,-0.500000000000039,6.7070656941304E-15));
#46990=DIRECTION('',(2.76820162751153E-15,8.61946552381544E-15,1.));
#46991=DIRECTION('',(2.76820162751153E-15,8.61946552381544E-15,1.));
#46992=DIRECTION('center_axis',(-0.499999999999935,-0.866025403784476,8.84877692442422E-15));
#46993=DIRECTION('ref_axis',(2.76820162751153E-15,8.61946552381544E-15,
1.));
#46994=DIRECTION('',(-0.866025403784484,0.499999999999922,-1.9123998296845E-15));
#46995=DIRECTION('',(2.76820162751153E-15,8.61946552381544E-15,1.));
#46996=DIRECTION('center_axis',(-1.,-6.76186946307289E-14,2.76820162751211E-15));
#46997=DIRECTION('ref_axis',(6.76186946307289E-14,-1.,8.61946552381525E-15));
#46998=DIRECTION('',(2.76820162751153E-15,8.61946552381544E-15,1.));
#46999=DIRECTION('',(6.76186946307289E-14,-1.,8.61946552381525E-15));
#47000=DIRECTION('center_axis',(-0.500000000000052,0.866025403784409,-6.08057529691215E-15));
#47001=DIRECTION('ref_axis',(-2.76820162751153E-15,-8.61946552381544E-15,
-1.));
#47002=DIRECTION('',(0.866025403784402,0.500000000000063,-6.70706569413058E-15));
#47003=DIRECTION('',(2.76820162751153E-15,8.61946552381544E-15,1.));
#47004=DIRECTION('center_axis',(0.499999999999935,0.866025403784476,-8.84877692442422E-15));
#47005=DIRECTION('ref_axis',(-2.76820162751153E-15,-8.61946552381544E-15,
-1.));
#47006=DIRECTION('',(0.86602540378447,-0.499999999999946,1.91239982968476E-15));
#47007=DIRECTION('',(2.76820162751153E-15,8.61946552381544E-15,1.));
#47008=DIRECTION('center_axis',(1.,6.76186946307289E-14,-2.76820162751211E-15));
#47009=DIRECTION('ref_axis',(-6.76186946307289E-14,1.,-8.61946552381525E-15));
#47010=DIRECTION('',(6.76186946307289E-14,-1.,8.61946552381525E-15));
#47011=DIRECTION('center_axis',(1.81869877965002E-13,-7.82952713580378E-13,
-1.));
#47012=DIRECTION('ref_axis',(0.604207940126797,-0.796826684472686,7.33764839197491E-13));
#47013=DIRECTION('center_axis',(-2.76820162751153E-15,-8.61946552381544E-15,
-1.));
#47014=DIRECTION('ref_axis',(-0.723116678427418,-0.690725900325229,7.9554208503632E-15));
#47015=DIRECTION('center_axis',(2.76820162751153E-15,8.61946552381544E-15,
1.));
#47016=DIRECTION('ref_axis',(-6.76186946307289E-14,1.,-8.61946552381525E-15));
#47017=DIRECTION('center_axis',(2.76820162751153E-15,8.61946552381544E-15,
1.));
#47018=DIRECTION('ref_axis',(-6.76186946307289E-14,1.,-8.61946552381525E-15));
#47019=DIRECTION('',(6.76186946307289E-14,-1.,8.61946552381525E-15));
#47020=DIRECTION('',(0.86602540378447,-0.499999999999946,1.91239982968475E-15));
#47021=DIRECTION('',(0.866025403784403,0.500000000000063,-6.70706569413057E-15));
#47022=DIRECTION('',(-6.76186946307289E-14,1.,-8.61946552381525E-15));
#47023=DIRECTION('',(-0.866025403784483,0.499999999999923,-1.91239982968452E-15));
#47024=DIRECTION('',(-0.866025403784416,-0.50000000000004,6.70706569413041E-15));
#47025=DIRECTION('center_axis',(0.500000000000042,-0.866025403784415,6.08057529691222E-15));
#47026=DIRECTION('ref_axis',(2.76820162751153E-15,8.61946552381544E-15,
1.));
#47027=DIRECTION('',(-0.866025403784416,-0.50000000000004,6.70706569413041E-15));
#47028=DIRECTION('',(2.76820162751153E-15,8.61946552381544E-15,1.));
#47029=DIRECTION('',(2.76820162751153E-15,8.61946552381544E-15,1.));
#47030=DIRECTION('center_axis',(-0.499999999999925,-0.866025403784482,8.84877692442425E-15));
#47031=DIRECTION('ref_axis',(2.76820162751153E-15,8.61946552381544E-15,
1.));
#47032=DIRECTION('',(-0.866025403784483,0.499999999999923,-1.91239982968452E-15));
#47033=DIRECTION('',(2.76820162751153E-15,8.61946552381544E-15,1.));
#47034=DIRECTION('center_axis',(-1.,-6.76186946307289E-14,2.76820162751211E-15));
#47035=DIRECTION('ref_axis',(6.76186946307289E-14,-1.,8.61946552381525E-15));
#47036=DIRECTION('',(2.76820162751153E-15,8.61946552381544E-15,1.));
#47037=DIRECTION('',(6.76186946307289E-14,-1.,8.61946552381525E-15));
#47038=DIRECTION('center_axis',(-0.500000000000067,0.8660254037844,-6.08057529691203E-15));
#47039=DIRECTION('ref_axis',(-2.76820162751153E-15,-8.61946552381544E-15,
-1.));
#47040=DIRECTION('',(0.866025403784403,0.500000000000063,-6.70706569413057E-15));
#47041=DIRECTION('',(2.76820162751153E-15,8.61946552381544E-15,1.));
#47042=DIRECTION('center_axis',(0.499999999999949,0.866025403784468,-8.84877692442419E-15));
#47043=DIRECTION('ref_axis',(-2.76820162751153E-15,-8.61946552381544E-15,
-1.));
#47044=DIRECTION('',(0.86602540378447,-0.499999999999946,1.91239982968475E-15));
#47045=DIRECTION('',(2.76820162751153E-15,8.61946552381544E-15,1.));
#47046=DIRECTION('center_axis',(1.,6.76186946307289E-14,-2.76820162751211E-15));
#47047=DIRECTION('ref_axis',(-6.76186946307289E-14,1.,-8.61946552381525E-15));
#47048=DIRECTION('',(6.76186946307289E-14,-1.,8.61946552381525E-15));
#47049=DIRECTION('center_axis',(-1.41326950697088E-14,6.61744312041589E-15,
-1.));
#47050=DIRECTION('ref_axis',(1.00411787721427E-13,-1.,-6.61744312041731E-15));
#47051=DIRECTION('center_axis',(-2.76820162751153E-15,-8.61946552381544E-15,
-1.));
#47052=DIRECTION('ref_axis',(-0.723116678427638,0.690725900324999,-3.95195531815359E-15));
#47053=DIRECTION('center_axis',(2.76820162751153E-15,8.61946552381544E-15,
1.));
#47054=DIRECTION('ref_axis',(-6.76186946307289E-14,1.,-8.61946552381525E-15));
#47055=DIRECTION('center_axis',(-0.500000000000092,-4.12740234260384E-14,
-0.866025403784385));
#47056=DIRECTION('ref_axis',(6.76186946307289E-14,-1.,8.61946552381525E-15));
#47057=DIRECTION('',(6.76186946307289E-14,-1.,8.61946552381525E-15));
#47058=DIRECTION('',(-0.866025403784434,-5.42497745590456E-14,0.500000000000009));
#47059=DIRECTION('center_axis',(-1.,-6.76186946307289E-14,2.76820162751211E-15));
#47060=DIRECTION('ref_axis',(6.76186946307289E-14,-1.,8.61946552381525E-15));
#47061=DIRECTION('',(6.76186946307289E-14,-1.,8.61946552381525E-15));
#47062=DIRECTION('',(-2.76820162751153E-15,-8.61946552381544E-15,-1.));
#47063=DIRECTION('center_axis',(-0.500000000000086,-2.63446712047025E-14,
0.866025403784389));
#47064=DIRECTION('ref_axis',(-6.76186946307289E-14,1.,-8.61946552381525E-15));
#47065=DIRECTION('',(0.866025403784436,6.28692400828612E-14,0.500000000000004));
#47066=DIRECTION('center_axis',(6.76186946307289E-14,-1.,8.61946552381525E-15));
#47067=DIRECTION('ref_axis',(2.76820162751153E-15,8.61946552381544E-15,
1.));
#47068=DIRECTION('center_axis',(6.64065221755448E-14,-1.,9.21875409050844E-15));
#47069=DIRECTION('ref_axis',(0.581108581114921,4.60918619770155E-14,0.813826036051073));
#47070=DIRECTION('center_axis',(-9.65575655111783E-14,1.,-1.71288144210529E-13));
#47071=DIRECTION('ref_axis',(0.581108581115006,1.95509181315509E-13,0.813826036051013));
#47072=DIRECTION('',(0.404443987336382,-0.718054433443912,0.56641229834723));
#47073=DIRECTION('center_axis',(5.6099210001032E-16,9.3655835268151E-15,
1.));
#47074=DIRECTION('ref_axis',(0.581108581115001,-0.813826036051017,7.29595839367891E-15));
#47075=DIRECTION('',(-0.503254793602719,0.704794021481373,0.499999999999998));
#47076=DIRECTION('center_axis',(-2.76820162751153E-15,-8.61946552381544E-15,
-1.));
#47077=DIRECTION('ref_axis',(6.76186946307289E-14,-1.,8.61946552381525E-15));
#47078=DIRECTION('center_axis',(-2.76820162751153E-15,-8.61946552381544E-15,
-1.));
#47079=DIRECTION('ref_axis',(6.76186946307289E-14,-1.,8.61946552381525E-15));
#47080=DIRECTION('center_axis',(2.76820162751153E-15,8.61946552381544E-15,
1.));
#47081=DIRECTION('ref_axis',(-6.76186946307289E-14,1.,-8.61946552381525E-15));
#47082=DIRECTION('',(2.76820162751153E-15,8.61946552381544E-15,1.));
#47083=DIRECTION('center_axis',(3.69713693691E-15,-8.619465523815E-15,-1.));
#47084=DIRECTION('ref_axis',(-6.76186946307289E-14,1.,-8.61946552381525E-15));
#47085=DIRECTION('center_axis',(3.69713693691E-15,-8.619465523815E-15,-1.));
#47086=DIRECTION('ref_axis',(-6.76186946307289E-14,1.,-8.61946552381525E-15));
#47087=DIRECTION('center_axis',(4.30983829725209E-15,4.10806165286643E-16,
1.));
#47088=DIRECTION('ref_axis',(0.581108581114977,-0.813826036051033,-2.17015926467059E-15));
#47089=DIRECTION('',(-0.410905818312085,0.575461908797847,0.707106781186558));
#47090=DIRECTION('center_axis',(-2.76820162751153E-15,-8.61946552381544E-15,
-1.));
#47091=DIRECTION('ref_axis',(0.58110858111497,-0.813826036051039,5.40611974012193E-15));
#47092=DIRECTION('center_axis',(-3.59801443811168E-16,8.889746359504E-15,
1.));
#47093=DIRECTION('ref_axis',(0.581108581114948,-0.813826036051054,7.44379074775065E-15));
#47094=DIRECTION('',(-0.503254793602674,0.704794021481406,0.499999999999998));
#47095=DIRECTION('center_axis',(-2.76820162751153E-15,-8.61946552381544E-15,
-1.));
#47096=DIRECTION('ref_axis',(6.76186946307289E-14,-1.,8.61946552381525E-15));
#47097=DIRECTION('center_axis',(-2.76820162751153E-15,-8.61946552381544E-15,
-1.));
#47098=DIRECTION('ref_axis',(6.76186946307289E-14,-1.,8.61946552381525E-15));
#47099=DIRECTION('center_axis',(2.76820162751153E-15,8.61946552381544E-15,
1.));
#47100=DIRECTION('ref_axis',(-6.76186946307289E-14,1.,-8.61946552381525E-15));
#47101=DIRECTION('',(2.76820162751153E-15,8.61946552381544E-15,1.));
#47102=DIRECTION('center_axis',(3.69713693690996E-15,-8.619465523815E-15,
-1.));
#47103=DIRECTION('ref_axis',(-6.11533560663074E-14,1.,-8.61946552381523E-15));
#47104=DIRECTION('center_axis',(3.69713693690996E-15,-8.619465523815E-15,
-1.));
#47105=DIRECTION('ref_axis',(-6.11533560663074E-14,1.,-8.61946552381523E-15));
#47106=DIRECTION('center_axis',(3.29485372431133E-15,4.95596058581936E-15,
1.));
#47107=DIRECTION('ref_axis',(0.581108581114976,-0.813826036051034,2.11862198566658E-15));
#47108=DIRECTION('',(-0.410905818312097,0.575461908797867,0.707106781186535));
#47109=DIRECTION('center_axis',(-1.06388358038234E-14,-1.25106454085894E-14,
-1.));
#47110=DIRECTION('ref_axis',(0.581108581114972,-0.813826036051037,3.99917018263746E-15));
#47111=DIRECTION('center_axis',(5.88076910790884E-16,9.00223320092517E-15,
1.));
#47112=DIRECTION('ref_axis',(0.581108581115008,-0.813826036051012,6.98451522229955E-15));
#47113=DIRECTION('',(-0.503254793602725,0.704794021481369,0.499999999999999));
#47114=DIRECTION('center_axis',(-2.76820162751153E-15,-8.61946552381544E-15,
-1.));
#47115=DIRECTION('ref_axis',(6.76186946307289E-14,-1.,8.61946552381525E-15));
#47116=DIRECTION('center_axis',(-2.76820162751153E-15,-8.61946552381544E-15,
-1.));
#47117=DIRECTION('ref_axis',(6.76186946307289E-14,-1.,8.61946552381525E-15));
#47118=DIRECTION('center_axis',(2.76820162751153E-15,8.61946552381544E-15,
1.));
#47119=DIRECTION('ref_axis',(-6.76186946307289E-14,1.,-8.61946552381525E-15));
#47120=DIRECTION('',(2.76820162751153E-15,8.61946552381544E-15,1.));
#47121=DIRECTION('center_axis',(3.69713693691E-15,-8.619465523815E-15,-1.));
#47122=DIRECTION('ref_axis',(-6.76186946307289E-14,1.,-8.61946552381525E-15));
#47123=DIRECTION('center_axis',(3.69713693691E-15,-8.619465523815E-15,-1.));
#47124=DIRECTION('ref_axis',(-6.76186946307289E-14,1.,-8.61946552381525E-15));
#47125=DIRECTION('center_axis',(4.86521817410701E-15,-3.63808999178412E-15,
1.));
#47126=DIRECTION('ref_axis',(0.581108581114975,-0.813826036051035,-5.78799238678073E-15));
#47127=DIRECTION('',(-0.410905818312084,0.575461908797846,0.707106781186559));
#47128=DIRECTION('center_axis',(-1.06388358038235E-14,-1.25106454085894E-14,
-1.));
#47129=DIRECTION('ref_axis',(0.581108581114972,-0.813826036051037,3.99917018263743E-15));
#47130=DIRECTION('center_axis',(6.33479347696713E-14,-1.,5.11722901977433E-14));
#47131=DIRECTION('ref_axis',(0.581108581114944,-4.83331359671811E-15,-0.813826036051057));
#47132=DIRECTION('center_axis',(6.76186946307289E-14,-1.,8.61946552381525E-15));
#47133=DIRECTION('ref_axis',(-2.48314835913838E-14,-8.61946552381693E-15,
-1.));
#47134=DIRECTION('center_axis',(6.76186946307289E-14,-1.,8.61946552381525E-15));
#47135=DIRECTION('ref_axis',(-2.48314835913838E-14,-8.61946552381693E-15,
-1.));
#47136=DIRECTION('',(-0.410905818312021,-0.70710678118655,0.575461908797901));
#47137=DIRECTION('center_axis',(6.76186946307289E-14,-1.,8.61946552381525E-15));
#47138=DIRECTION('ref_axis',(2.76820162751153E-15,8.61946552381544E-15,
1.));
#47139=DIRECTION('center_axis',(-6.76186946307289E-14,1.,-8.61946552381525E-15));
#47140=DIRECTION('ref_axis',(-2.76820162751153E-15,-8.61946552381544E-15,
-1.));
#47141=DIRECTION('',(-6.76186946307289E-14,1.,-8.61946552381525E-15));
#47142=DIRECTION('center_axis',(6.76186946307289E-14,-1.,8.61946552381525E-15));
#47143=DIRECTION('ref_axis',(-2.48314835913838E-14,-8.61946552381693E-15,
-1.));
#47144=DIRECTION('center_axis',(6.76186946307289E-14,-1.,8.61946552381525E-15));
#47145=DIRECTION('ref_axis',(-2.48314835913838E-14,-8.61946552381693E-15,
-1.));
#47146=DIRECTION('center_axis',(7.65423745898236E-14,-1.,-2.05160675258287E-15));
#47147=DIRECTION('ref_axis',(0.581108581114976,4.61490816840534E-14,-0.813826036051034));
#47148=DIRECTION('',(-0.503254793602654,-0.500000000000061,0.704794021481375));
#47149=DIRECTION('center_axis',(6.53682722901527E-14,-1.,5.01484468347945E-14));
#47150=DIRECTION('ref_axis',(0.581108581114942,-2.82604774121214E-15,-0.813826036051058));
#47151=DIRECTION('center_axis',(6.76186946307289E-14,-1.,8.61946552381525E-15));
#47152=DIRECTION('ref_axis',(-3.63004857922531E-15,-8.6194655238155E-15,
-1.));
#47153=DIRECTION('center_axis',(6.76186946307289E-14,-1.,8.61946552381525E-15));
#47154=DIRECTION('ref_axis',(-3.63004857922531E-15,-8.6194655238155E-15,
-1.));
#47155=DIRECTION('',(-0.410905818312018,-0.707106781186553,0.5754619087979));
#47156=DIRECTION('center_axis',(6.76186946307289E-14,-1.,8.61946552381525E-15));
#47157=DIRECTION('ref_axis',(3.05202999048964E-15,8.61946552381546E-15,
1.));
#47158=DIRECTION('center_axis',(-6.76186946307289E-14,1.,-8.61946552381525E-15));
#47159=DIRECTION('ref_axis',(-1.733985285455E-15,-8.61946552381537E-15,
-1.));
#47160=DIRECTION('',(-6.76186946307289E-14,1.,-8.61946552381525E-15));
#47161=DIRECTION('center_axis',(6.76186946307289E-14,-1.,8.61946552381525E-15));
#47162=DIRECTION('ref_axis',(-3.63004857922531E-15,-8.6194655238155E-15,
-1.));
#47163=DIRECTION('center_axis',(6.76186946307289E-14,-1.,8.61946552381525E-15));
#47164=DIRECTION('ref_axis',(-3.63004857922531E-15,-8.6194655238155E-15,
-1.));
#47165=DIRECTION('center_axis',(6.78759665746252E-14,-1.,9.97879302069915E-15));
#47166=DIRECTION('ref_axis',(0.581108581114945,3.13223050593763E-14,-0.813826036051057));
#47167=DIRECTION('',(-0.503254793602635,-0.500000000000038,0.704794021481405));
#47168=DIRECTION('center_axis',(6.67758619002206E-14,-1.,4.14702793352544E-14));
#47169=DIRECTION('ref_axis',(0.581108581114937,5.05443331622382E-15,-0.813826036051062));
#47170=DIRECTION('center_axis',(6.76186946307289E-14,-1.,8.61946552381525E-15));
#47171=DIRECTION('ref_axis',(-9.49060785087889E-15,-8.61946552381589E-15,
-1.));
#47172=DIRECTION('center_axis',(6.76186946307289E-14,-1.,8.61946552381525E-15));
#47173=DIRECTION('ref_axis',(-9.49060785087889E-15,-8.61946552381589E-15,
-1.));
#47174=DIRECTION('',(-0.410905818312006,-0.707106781186571,0.575461908797887));
#47175=DIRECTION('center_axis',(6.76186946307289E-14,-1.,8.61946552381525E-15));
#47176=DIRECTION('ref_axis',(3.05202999048964E-15,8.61946552381546E-15,
1.));
#47177=DIRECTION('center_axis',(-6.76186946307289E-14,1.,-8.61946552381525E-15));
#47178=DIRECTION('ref_axis',(-2.76820162751153E-15,-8.61946552381544E-15,
-1.));
#47179=DIRECTION('',(-6.76186946307289E-14,1.,-8.61946552381525E-15));
#47180=DIRECTION('center_axis',(6.76186946307289E-14,-1.,8.61946552381525E-15));
#47181=DIRECTION('ref_axis',(-9.49060785087889E-15,-8.61946552381589E-15,
-1.));
#47182=DIRECTION('center_axis',(6.76186946307289E-14,-1.,8.61946552381525E-15));
#47183=DIRECTION('ref_axis',(-9.49060785087889E-15,-8.61946552381589E-15,
-1.));
#47184=DIRECTION('center_axis',(6.72666596076196E-14,-1.,3.72070857470792E-15));
#47185=DIRECTION('ref_axis',(0.581108581114906,3.60612236102673E-14,-0.813826036051084));
#47186=DIRECTION('',(-0.503254793602603,-0.500000000000039,0.704794021481428));
#47187=DIRECTION('center_axis',(6.32234636366842E-14,-1.,5.05743183170403E-14));
#47188=DIRECTION('ref_axis',(0.581108581114942,-4.41899975485568E-15,-0.813826036051059));
#47189=DIRECTION('center_axis',(6.76186946307289E-14,-1.,8.61946552381525E-15));
#47190=DIRECTION('ref_axis',(-1.37998426094478E-14,-8.61946552381618E-15,
-1.));
#47191=DIRECTION('center_axis',(6.76186946307289E-14,-1.,8.61946552381525E-15));
#47192=DIRECTION('ref_axis',(-1.37998426094478E-14,-8.61946552381618E-15,
-1.));
#47193=DIRECTION('',(-0.41090581831202,-0.707106781186551,0.575461908797902));
#47194=DIRECTION('center_axis',(6.76186946307289E-14,-1.,8.61946552381525E-15));
#47195=DIRECTION('ref_axis',(2.76820162751153E-15,8.61946552381544E-15,
1.));
#47196=DIRECTION('center_axis',(-6.76186946307289E-14,1.,-8.61946552381525E-15));
#47197=DIRECTION('ref_axis',(-2.76820162751153E-15,-8.61946552381544E-15,
-1.));
#47198=DIRECTION('',(-6.76186946307289E-14,1.,-8.61946552381525E-15));
#47199=DIRECTION('center_axis',(6.76186946307289E-14,-1.,8.61946552381525E-15));
#47200=DIRECTION('ref_axis',(-1.37998426094478E-14,-8.61946552381618E-15,
-1.));
#47201=DIRECTION('center_axis',(6.76186946307289E-14,-1.,8.61946552381525E-15));
#47202=DIRECTION('ref_axis',(-1.37998426094478E-14,-8.61946552381618E-15,
-1.));
#47203=DIRECTION('center_axis',(9.67592503490828E-14,-1.,2.54696229331101E-15));
#47204=DIRECTION('ref_axis',(0.581108581114985,5.41548464529684E-14,-0.813826036051028));
#47205=DIRECTION('',(-0.503254793602645,-0.500000000000086,0.704794021481363));
#47206=DIRECTION('center_axis',(1.,6.71040227609779E-14,-6.15348789557069E-15));
#47207=DIRECTION('ref_axis',(5.10351562267452E-14,-0.813826036051079,-0.581108581114913));
#47208=DIRECTION('',(0.499999999999963,0.704794021481455,0.503254793602639));
#47209=DIRECTION('center_axis',(1.,6.74942672049691E-14,2.10846237357168E-16));
#47210=DIRECTION('ref_axis',(5.50511164934163E-14,-0.813826036051077,-0.581108581114916));
#47211=DIRECTION('',(0.49999999999996,0.704794021481453,0.503254793602645));
#47212=DIRECTION('center_axis',(-1.,-6.76943554026594E-14,4.44730235615136E-15));
#47213=DIRECTION('ref_axis',(-5.76757944823519E-14,0.813826036051088,-0.581108581114901));
#47214=DIRECTION('',(-0.499999999999891,-0.704794021481494,0.503254793602656));
#47215=DIRECTION('center_axis',(-1.,-6.73743035966667E-14,2.51091843077615E-15));
#47216=DIRECTION('ref_axis',(-5.62900786743789E-14,0.813826036051049,-0.581108581114955));
#47217=DIRECTION('',(-0.499999999999892,-0.70479402148146,0.503254793602702));
#47218=DIRECTION('center_axis',(-1.,-6.88839483209371E-14,2.14531849659727E-15));
#47219=DIRECTION('ref_axis',(-5.7306213597172E-14,0.813826036051065,-0.581108581114932));
#47220=DIRECTION('',(-0.49999999999989,-0.704794021481476,0.503254793602683));
#47221=DIRECTION('center_axis',(-1.,-7.05708043906952E-14,8.00863989428406E-15));
#47222=DIRECTION('ref_axis',(-6.20862473638422E-14,0.813826036051061,-0.581108581114939));
#47223=DIRECTION('',(-0.499999999999883,-0.704794021481474,0.503254793602693));
#47224=DIRECTION('center_axis',(1.,6.77182365713367E-14,-5.15143991940756E-15));
#47225=DIRECTION('ref_axis',(5.21173180949558E-14,-0.813826036051097,-0.581108581114889));
#47226=DIRECTION('',(0.499999999999958,0.704794021481473,0.50325479360262));
#47227=DIRECTION('center_axis',(1.,6.61468802924239E-14,-1.56305132901373E-15));
#47228=DIRECTION('ref_axis',(5.29237508455151E-14,-0.813826036051071,-0.581108581114924));
#47229=DIRECTION('',(0.499999999999957,0.70479402148145,0.503254793602653));
#47230=DIRECTION('center_axis',(0.700909264299893,-0.71325044915414,4.20757949015711E-15));
#47231=DIRECTION('ref_axis',(2.76820162751153E-15,8.61946552381544E-15,
1.));
#47232=DIRECTION('',(-2.76820162751153E-15,-8.61946552381544E-15,-1.));
#47233=DIRECTION('',(-2.76820162751153E-15,-8.61946552381544E-15,-1.));
#47234=DIRECTION('',(0.713250449154132,0.700909264299901,-8.01588429312764E-15));
#47235=DIRECTION('center_axis',(0.999847695156392,-0.0174524064372163,-2.61734960140238E-15));
#47236=DIRECTION('ref_axis',(0.0174524064372163,0.999847695156392,-8.66646451737035E-15));
#47237=DIRECTION('',(-2.76820162751153E-15,-8.61946552381544E-15,-1.));
#47238=DIRECTION('',(0.0174524064372164,0.999847695156392,-8.66646451737035E-15));
#47239=DIRECTION('center_axis',(-0.99984769515639,-0.0174524064373646,2.91821043259005E-15));
#47240=DIRECTION('ref_axis',(0.0174524064373646,-0.99984769515639,8.56984095756293E-15));
#47241=DIRECTION('',(-2.76820162751153E-15,-8.61946552381544E-15,-1.));
#47242=DIRECTION('',(-2.76820162751153E-15,-8.61946552381544E-15,-1.));
#47243=DIRECTION('',(0.0174524064373627,-0.99984769515639,8.56984095756293E-15));
#47244=DIRECTION('center_axis',(0.99984769515639,0.0174524064373491,-2.91821043258992E-15));
#47245=DIRECTION('ref_axis',(-0.0174524064373491,0.99984769515639,-8.56984095756297E-15));
#47246=DIRECTION('',(-2.76820162751153E-15,-8.61946552381544E-15,-1.));
#47247=DIRECTION('',(-0.0174524064373516,0.99984769515639,-8.56984095756296E-15));
#47248=DIRECTION('center_axis',(0.700909264299797,0.713250449154235,-8.08809582250341E-15));
#47249=DIRECTION('ref_axis',(-2.76820162751153E-15,-8.61946552381544E-15,
-1.));
#47250=DIRECTION('',(-2.76820162751153E-15,-8.61946552381544E-15,-1.));
#47251=DIRECTION('',(-0.713250449154234,0.700909264299797,-4.06704218478287E-15));
#47252=DIRECTION('center_axis',(-6.76186946307289E-14,1.,-8.61946552381525E-15));
#47253=DIRECTION('ref_axis',(-2.76820162751153E-15,-8.61946552381544E-15,
-1.));
#47254=DIRECTION('',(-2.76820162751153E-15,-8.61946552381544E-15,-1.));
#47255=DIRECTION('',(-1.,-6.76186946307289E-14,2.76820162751211E-15));
#47256=DIRECTION('center_axis',(-0.700909264299919,0.713250449154115,-4.20757949015682E-15));
#47257=DIRECTION('ref_axis',(-2.76820162751153E-15,-8.61946552381544E-15,
-1.));
#47258=DIRECTION('',(-2.76820162751153E-15,-8.61946552381544E-15,-1.));
#47259=DIRECTION('',(-0.713250449154127,-0.700909264299906,8.01588429312767E-15));
#47260=DIRECTION('center_axis',(-0.999847695156392,0.0174524064372294,2.61734960140226E-15));
#47261=DIRECTION('ref_axis',(-0.0174524064372294,-0.999847695156392,8.66646451737038E-15));
#47262=DIRECTION('',(-0.0174524064372275,-0.999847695156392,8.66646451737038E-15));
#47263=DIRECTION('center_axis',(2.76820162751153E-15,8.61946552381544E-15,
1.));
#47264=DIRECTION('ref_axis',(-6.76186946307289E-14,1.,-8.61946552381525E-15));
#47265=DIRECTION('',(0.713250449154216,-0.700909264299816,4.06704218478308E-15));
#47266=DIRECTION('',(1.,6.76186946307289E-14,-2.76820162751211E-15));
#47267=DIRECTION('',(1.,6.76186946307289E-14,-2.76820162751211E-15));
#47268=DIRECTION('',(0.707106781186591,-0.707106781186504,4.13746837958802E-15));
#47269=DIRECTION('',(6.76186946307289E-14,-1.,8.61946552381525E-15));
#47270=DIRECTION('',(-0.707106781186496,-0.707106781186599,8.05229666459889E-15));
#47271=DIRECTION('',(-1.,-6.76186946307289E-14,2.76820162751211E-15));
#47272=DIRECTION('',(-0.707106781186596,0.707106781186499,-4.13746837958796E-15));
#47273=DIRECTION('',(-6.76186946307289E-14,1.,-8.61946552381525E-15));
#47274=DIRECTION('',(0.707106781186499,0.707106781186596,-8.05229666459888E-15));
#47275=DIRECTION('center_axis',(-6.76186946307289E-14,1.,-8.61946552381525E-15));
#47276=DIRECTION('ref_axis',(-2.76820162751153E-15,-8.61946552381544E-15,
-1.));
#47277=DIRECTION('center_axis',(-6.76186946307289E-14,1.,-8.61946552381525E-15));
#47278=DIRECTION('ref_axis',(2.63574839145508E-15,8.61946552381543E-15,
1.));
#47279=DIRECTION('center_axis',(-6.76186946307289E-14,1.,-8.61946552381525E-15));
#47280=DIRECTION('ref_axis',(2.38983587987361E-15,8.61946552381541E-15,
1.));
#47281=DIRECTION('center_axis',(6.76186946307289E-14,-1.,8.61946552381525E-15));
#47282=DIRECTION('ref_axis',(2.76820162751153E-15,8.61946552381544E-15,
1.));
#47283=DIRECTION('',(6.76186946307289E-14,-1.,8.61946552381525E-15));
#47284=DIRECTION('center_axis',(6.79293010634548E-14,-1.,8.57280588232624E-15));
#47285=DIRECTION('ref_axis',(0.581108581114923,4.64510723861615E-14,0.813826036051072));
#47286=DIRECTION('center_axis',(9.1381416771988E-14,-1.,1.06325780643712E-14));
#47287=DIRECTION('ref_axis',(0.581108581114925,4.44494565815108E-14,-0.813826036051071));
#47288=DIRECTION('center_axis',(-6.76186946307289E-14,1.,-8.61946552381525E-15));
#47289=DIRECTION('ref_axis',(0.581108581114916,3.22790582335802E-14,-0.813826036051077));
#47290=DIRECTION('',(-0.290554290557368,-0.866025403784476,0.406913018025524));
#47291=DIRECTION('center_axis',(-6.76186946307289E-14,1.,-8.61946552381525E-15));
#47292=DIRECTION('ref_axis',(0.581108581114917,3.22790582335802E-14,-0.813826036051077));
#47293=DIRECTION('center_axis',(-6.76186946307289E-14,1.,-8.61946552381525E-15));
#47294=DIRECTION('ref_axis',(0.581108581114916,3.22790582335802E-14,-0.813826036051077));
#47295=DIRECTION('center_axis',(-1.,-6.76186946307289E-14,2.76820162751211E-15));
#47296=DIRECTION('ref_axis',(6.76186946307289E-14,-1.,8.61946552381525E-15));
#47297=DIRECTION('center_axis',(-0.707106781186559,-5.39085200304649E-14,
-0.707106781186537));
#47298=DIRECTION('ref_axis',(6.76186946307289E-14,-1.,8.61946552381525E-15));
#47299=DIRECTION('',(0.707106781186545,4.17187549862772E-14,-0.70710678118655));
#47300=DIRECTION('center_axis',(0.707106781186545,4.17187549862772E-14,
-0.70710678118655));
#47301=DIRECTION('ref_axis',(6.76186946307289E-14,-1.,8.61946552381525E-15));
#47302=DIRECTION('',(-6.76186946307289E-14,1.,-8.61946552381525E-15));
#47303=DIRECTION('',(0.70710678118655,5.39085200304644E-14,0.707106781186545));
#47304=DIRECTION('center_axis',(1.,6.76186946307289E-14,-2.76820162751211E-15));
#47305=DIRECTION('ref_axis',(-6.76186946307289E-14,1.,-8.61946552381525E-15));
#47306=DIRECTION('',(-6.76186946307289E-14,1.,-8.61946552381525E-15));
#47307=DIRECTION('',(2.76820162751153E-15,8.61946552381544E-15,1.));
#47308=DIRECTION('center_axis',(0.707106781186549,5.39085200304643E-14,
0.707106781186546));
#47309=DIRECTION('ref_axis',(-6.76186946307289E-14,1.,-8.61946552381525E-15));
#47310=DIRECTION('',(-6.76186946307289E-14,1.,-8.61946552381525E-15));
#47311=DIRECTION('',(-0.707106781186546,-4.17187549862773E-14,0.707106781186549));
#47312=DIRECTION('center_axis',(2.76820162751153E-15,8.61946552381544E-15,
1.));
#47313=DIRECTION('ref_axis',(-6.76186946307289E-14,1.,-8.61946552381525E-15));
#47314=DIRECTION('',(-6.76186946307289E-14,1.,-8.61946552381525E-15));
#47315=DIRECTION('',(-1.,-6.76186946307289E-14,2.76820162751211E-15));
#47316=DIRECTION('center_axis',(-0.707106781186553,-4.17187549862778E-14,
0.707106781186542));
#47317=DIRECTION('ref_axis',(-6.76186946307289E-14,1.,-8.61946552381525E-15));
#47318=DIRECTION('',(-6.76186946307289E-14,1.,-8.61946552381525E-15));
#47319=DIRECTION('',(-0.707106781186549,-5.39085200304643E-14,-0.707106781186546));
#47320=DIRECTION('center_axis',(-1.,-6.76186946307289E-14,2.76820162751211E-15));
#47321=DIRECTION('ref_axis',(6.76186946307289E-14,-1.,8.61946552381525E-15));
#47322=DIRECTION('',(-2.76820162751153E-15,-8.61946552381544E-15,-1.));
#47323=DIRECTION('center_axis',(6.76186946307289E-14,-1.,8.61946552381525E-15));
#47324=DIRECTION('ref_axis',(2.76820162751153E-15,8.61946552381544E-15,
1.));
#47325=DIRECTION('center_axis',(6.76186946307289E-14,-1.,8.61946552381525E-15));
#47326=DIRECTION('ref_axis',(2.76820162751153E-15,8.61946552381544E-15,
1.));
#47327=DIRECTION('',(-2.76820162751153E-15,-8.61946552381544E-15,-1.));
#47328=DIRECTION('center_axis',(-0.700909264299829,-0.713250449154203,8.08809582250323E-15));
#47329=DIRECTION('ref_axis',(2.76820162751153E-15,8.61946552381544E-15,
1.));
#47330=DIRECTION('center_axis',(1.2292818201763E-14,7.4680920425664E-16,
-1.));
#47331=DIRECTION('ref_axis',(-0.366154256380766,-0.930554168511564,-5.19601412559431E-15));
#47332=DIRECTION('center_axis',(-2.39129758992329E-13,1.,-5.41905209207291E-14));
#47333=DIRECTION('ref_axis',(0.58110858111488,1.83062011782837E-13,0.813826036051103));
#47334=DIRECTION('center_axis',(-6.78836011028418E-14,1.,-8.61946552381525E-15));
#47335=DIRECTION('ref_axis',(2.63574839145508E-15,8.61946552381543E-15,
1.));
#47336=DIRECTION('center_axis',(-6.78836011028418E-14,1.,-8.61946552381525E-15));
#47337=DIRECTION('ref_axis',(2.63574839145508E-15,8.61946552381543E-15,
1.));
#47338=DIRECTION('',(-0.290554290557731,0.866025403784264,-0.406913018025715));
#47339=DIRECTION('center_axis',(-6.76186946307289E-14,1.,-8.61946552381525E-15));
#47340=DIRECTION('ref_axis',(-4.34309224384834E-15,-8.61946552381555E-15,
-1.));
#47341=DIRECTION('center_axis',(2.76820162751153E-15,8.61946552381544E-15,
1.));
#47342=DIRECTION('ref_axis',(-6.76186946307289E-14,1.,-8.61946552381525E-15));
#47343=DIRECTION('',(2.76820162751153E-15,8.61946552381544E-15,1.));
#47344=DIRECTION('center_axis',(1.50856361455885E-14,-2.19155353757076E-14,
1.));
#47345=DIRECTION('ref_axis',(0.581108581114967,-0.813826036051041,-2.66018258985281E-14));
#47346=DIRECTION('',(-0.290554290557446,0.406913018025467,0.866025403784476));
#47347=DIRECTION('center_axis',(-3.76067249290565E-15,-8.76855559371899E-15,
-1.));
#47348=DIRECTION('ref_axis',(0.581108581114973,-0.813826036051036,4.95071978433895E-15));
#47349=DIRECTION('center_axis',(6.76186946307289E-14,-1.,8.61946552381525E-15));
#47350=DIRECTION('ref_axis',(2.76820162751153E-15,8.61946552381544E-15,
1.));
#47351=DIRECTION('',(6.76186946307289E-14,-1.,8.61946552381525E-15));
#47352=DIRECTION('',(6.76186946307289E-14,-1.,8.61946552381525E-15));
#47353=DIRECTION('center_axis',(-4.04868893599724E-15,-9.20599848666658E-15,
-1.));
#47354=DIRECTION('ref_axis',(0.366154256380767,0.930554168511563,-1.00491249537558E-14));
#47355=DIRECTION('center_axis',(-1.72513257807643E-16,-8.12510286167748E-15,
-1.));
#47356=DIRECTION('ref_axis',(0.725826090825689,0.687878249312113,-5.71429615550167E-15));
#47357=DIRECTION('center_axis',(-6.76186946307289E-14,1.,-8.61946552381525E-15));
#47358=DIRECTION('ref_axis',(-2.76820162751153E-15,-8.61946552381544E-15,
-1.));
#47359=DIRECTION('center_axis',(6.76186946307289E-14,-1.,8.61946552381525E-15));
#47360=DIRECTION('ref_axis',(-3.14656737514945E-15,-8.61946552381546E-15,
-1.));
#47361=DIRECTION('',(-6.76186946307289E-14,1.,-8.61946552381525E-15));
#47362=DIRECTION('center_axis',(-6.76186946307289E-14,1.,-8.61946552381525E-15));
#47363=DIRECTION('ref_axis',(2.95738450133049E-15,8.61946552381545E-15,
1.));
#47364=DIRECTION('center_axis',(-4.60290999893993E-14,1.,2.77991799241815E-14));
#47365=DIRECTION('ref_axis',(0.581108581114917,4.1242085816692E-15,0.813826036051076));
#47366=DIRECTION('center_axis',(6.76186946307289E-14,-1.,8.61946552381525E-15));
#47367=DIRECTION('ref_axis',(-2.95738450133049E-15,-8.61946552381545E-15,
-1.));
#47368=DIRECTION('center_axis',(6.76186946307289E-14,-1.,8.61946552381525E-15));
#47369=DIRECTION('ref_axis',(-2.95738450133049E-15,-8.61946552381545E-15,
-1.));
#47370=DIRECTION('',(-0.290554290557484,0.866025403784451,-0.406913018025494));
#47371=DIRECTION('center_axis',(6.76771833175434E-14,-1.,8.8020274518373E-15));
#47372=DIRECTION('ref_axis',(0.58110858111492,4.64911110818535E-14,0.813826036051074));
#47373=DIRECTION('center_axis',(-6.76186946307289E-14,1.,-8.61946552381525E-15));
#47374=DIRECTION('ref_axis',(-2.76820162751153E-15,-8.61946552381544E-15,
-1.));
#47375=DIRECTION('',(0.500000000000004,4.12740234260329E-14,0.866025403784436));
#47376=DIRECTION('',(-0.499999999999999,-2.63446712046962E-14,0.866025403784439));
#47377=DIRECTION('',(-1.,-6.76186946307289E-14,2.76820162751211E-15));
#47378=DIRECTION('',(-0.500000000000002,-4.12740234260327E-14,-0.866025403784437));
#47379=DIRECTION('',(0.499999999999999,2.63446712046962E-14,-0.866025403784439));
#47380=DIRECTION('',(1.,6.76186946307289E-14,-2.76820162751211E-15));
#47381=DIRECTION('',(0.50000000000001,4.12740234260332E-14,0.866025403784433));
#47382=DIRECTION('',(-0.499999999999996,-2.6344671204696E-14,0.866025403784441));
#47383=DIRECTION('',(-1.,-6.76186946307289E-14,2.76820162751211E-15));
#47384=DIRECTION('',(-0.49999999999993,-4.12740234260283E-14,-0.866025403784479));
#47385=DIRECTION('',(0.499999999999925,2.63446712046908E-14,-0.866025403784482));
#47386=DIRECTION('',(1.,6.76186946307289E-14,-2.76820162751211E-15));
#47387=DIRECTION('center_axis',(6.76186946307289E-14,-1.,8.61946552381525E-15));
#47388=DIRECTION('ref_axis',(2.76820162751153E-15,8.61946552381544E-15,
1.));
#47389=DIRECTION('center_axis',(6.76186946307289E-14,-1.,8.61946552381525E-15));
#47390=DIRECTION('ref_axis',(-3.56323905882275E-15,-8.61946552381549E-15,
-1.));
#47391=DIRECTION('center_axis',(-6.76186946307289E-14,1.,-8.61946552381525E-15));
#47392=DIRECTION('ref_axis',(-2.76820162751153E-15,-8.61946552381544E-15,
-1.));
#47393=DIRECTION('center_axis',(-6.76186946307289E-14,1.,-8.61946552381525E-15));
#47394=DIRECTION('ref_axis',(-3.29822658171901E-15,-8.61946552381547E-15,
-1.));
#47395=DIRECTION('',(6.76186946307289E-14,-1.,8.61946552381525E-15));
#47396=DIRECTION('center_axis',(6.76186946307289E-14,-1.,8.61946552381525E-15));
#47397=DIRECTION('ref_axis',(2.76820162751153E-15,8.61946552381544E-15,
1.));
#47398=DIRECTION('center_axis',(-1.,-6.76186946307289E-14,2.76820162751211E-15));
#47399=DIRECTION('ref_axis',(2.76820162751153E-15,8.61946552381544E-15,
1.));
#47400=DIRECTION('center_axis',(1.,6.76186946307289E-14,-2.76820162751211E-15));
#47401=DIRECTION('ref_axis',(2.76820162751109E-15,1.5084804088237E-14,1.));
#47402=DIRECTION('center_axis',(1.,6.76186946307289E-14,-2.76820162751211E-15));
#47403=DIRECTION('ref_axis',(2.76820162751109E-15,1.5084804088237E-14,1.));
#47404=DIRECTION('',(-1.,-6.76186946307289E-14,2.76820162751211E-15));
#47405=DIRECTION('center_axis',(1.,6.43860253485181E-14,-2.76820162751208E-15));
#47406=DIRECTION('ref_axis',(2.76820162751111E-15,1.5084804088237E-14,1.));
#47407=DIRECTION('center_axis',(7.73833815973895E-14,-1.,3.53499671313689E-15));
#47408=DIRECTION('ref_axis',(0.581108581114921,4.20912747194277E-14,-0.813826036051074));
#47409=DIRECTION('center_axis',(-6.71511025994635E-14,1.,-8.61946552381525E-15));
#47410=DIRECTION('ref_axis',(1.13162951808259E-15,8.61946552381533E-15,
1.));
#47411=DIRECTION('center_axis',(-6.71511025994635E-14,1.,-8.61946552381525E-15));
#47412=DIRECTION('ref_axis',(1.13162951808259E-15,8.61946552381533E-15,
1.));
#47413=DIRECTION('',(0.290554290557414,0.86602540378444,-0.406913018025568));
#47414=DIRECTION('center_axis',(-6.83991273732483E-14,1.,-8.73670299263603E-15));
#47415=DIRECTION('ref_axis',(0.581108581114917,3.26371634927143E-14,-0.813826036051076));
#47416=DIRECTION('center_axis',(-6.76186946307289E-14,1.,-8.61946552381525E-15));
#47417=DIRECTION('ref_axis',(-2.76820162751153E-15,-8.61946552381544E-15,
-1.));
#47418=DIRECTION('',(-2.76820162751153E-15,-8.61946552381544E-15,-1.));
#47419=DIRECTION('',(-1.,-6.76186946307289E-14,2.76820162751211E-15));
#47420=DIRECTION('center_axis',(-6.8232481380125E-14,1.,-8.61946552381525E-15));
#47421=DIRECTION('ref_axis',(0.973373605804438,6.83914882087676E-14,0.229224395567456));
#47422=DIRECTION('',(-1.,-6.76186946307289E-14,2.76820162751211E-15));
#47423=DIRECTION('center_axis',(-7.77848709450126E-14,1.,-1.22269303430102E-14));
#47424=DIRECTION('ref_axis',(-1.,-7.77848709450126E-14,2.86757946494294E-15));
#47425=DIRECTION('center_axis',(-6.69464950962383E-14,1.,-8.61946552381525E-15));
#47426=DIRECTION('ref_axis',(0.968149047511612,6.69722803755674E-14,0.250374563009819));
#47427=DIRECTION('center_axis',(6.76186946307289E-14,-1.,8.61946552381525E-15));
#47428=DIRECTION('ref_axis',(2.76820162751153E-15,8.61946552381544E-15,
1.));
#47429=DIRECTION('center_axis',(-6.76670427534324E-14,1.,-8.468555544848E-15));
#47430=DIRECTION('ref_axis',(-0.581108581114919,-3.24299682125476E-14,0.813826036051075));
#47431=DIRECTION('center_axis',(6.76186946307289E-14,-1.,8.61946552381525E-15));
#47432=DIRECTION('ref_axis',(-1.,-6.76186946307288E-14,9.21957871251919E-15));
#47433=DIRECTION('',(6.76186946307289E-14,-1.,8.61946552381525E-15));
#47434=DIRECTION('center_axis',(-6.76186946307289E-14,1.,-8.61946552381525E-15));
#47435=DIRECTION('ref_axis',(0.968149047511612,6.76230697146222E-14,0.250374563009819));
#47436=DIRECTION('',(-6.76186946307289E-14,1.,-8.61946552381525E-15));
#47437=DIRECTION('center_axis',(-1.,-6.76186946307289E-14,2.76820162751211E-15));
#47438=DIRECTION('ref_axis',(2.76820162751153E-15,8.61946552381544E-15,
1.));
#47439=DIRECTION('center_axis',(1.,6.76186946307289E-14,-2.76820162751211E-15));
#47440=DIRECTION('ref_axis',(2.76820162751153E-15,8.61946552381544E-15,
1.));
#47441=DIRECTION('center_axis',(1.,6.76186946307289E-14,-2.76820162751211E-15));
#47442=DIRECTION('ref_axis',(2.76820162751153E-15,8.61946552381544E-15,
1.));
#47443=DIRECTION('',(-1.,-6.76186946307289E-14,2.76820162751211E-15));
#47444=DIRECTION('center_axis',(1.,6.43860253485181E-14,-2.76820162751208E-15));
#47445=DIRECTION('ref_axis',(2.76820162751153E-15,8.61946552381544E-15,
1.));
#47446=DIRECTION('center_axis',(-1.,-6.76186946307289E-14,2.76820162751211E-15));
#47447=DIRECTION('ref_axis',(6.76186946307289E-14,-1.,8.61946552381525E-15));
#47448=DIRECTION('',(6.76186946307289E-14,-1.,8.61946552381525E-15));
#47449=DIRECTION('',(6.76186946307289E-14,-1.,8.61946552381525E-15));
#47450=DIRECTION('center_axis',(-0.500000000000017,-4.12740234260337E-14,
-0.866025403784429));
#47451=DIRECTION('ref_axis',(6.76186946307289E-14,-1.,8.61946552381525E-15));
#47452=DIRECTION('',(6.76186946307289E-14,-1.,8.61946552381525E-15));
#47453=DIRECTION('',(-0.749999999999989,-0.499999999999975,0.433012701892267));
#47454=DIRECTION('',(-0.750000000000098,0.499999999999848,0.433012701892225));
#47455=DIRECTION('',(-6.76186946307289E-14,1.,-8.61946552381525E-15));
#47456=DIRECTION('',(0.749999999999838,0.500000000000272,-0.433012701892185));
#47457=DIRECTION('',(0.749999999999937,-0.50000000000015,-0.433012701892155));
#47458=DIRECTION('center_axis',(-0.433012701892109,-0.866025403784401,0.250000000000323));
#47459=DIRECTION('ref_axis',(-1.5567093557564E-14,0.277350098112963,0.960768922830422));
#47460=DIRECTION('',(0.749999999999939,-0.50000000000015,-0.433012701892152));
#47461=DIRECTION('',(-0.500000000000001,-4.12740234260327E-14,-0.866025403784438));
#47462=DIRECTION('',(-0.49999999999991,-4.12740234260269E-14,-0.866025403784491));
#47463=DIRECTION('center_axis',(0.433012701892224,-0.866025403784343,-0.250000000000326));
#47464=DIRECTION('ref_axis',(2.1760598381141E-14,-0.277350098112966,0.960768922830421));
#47465=DIRECTION('',(0.749999999999837,0.500000000000272,-0.433012701892187));
#47466=DIRECTION('',(-0.500000000000001,-4.12740234260327E-14,-0.866025403784438));
#47467=DIRECTION('center_axis',(0.866025403784435,5.42497745590457E-14,
-0.500000000000007));
#47468=DIRECTION('ref_axis',(6.76186946307289E-14,-1.,8.61946552381525E-15));
#47469=DIRECTION('',(-0.500000000000001,-4.12740234260327E-14,-0.866025403784438));
#47470=DIRECTION('',(6.76186946307289E-14,-1.,8.61946552381525E-15));
#47471=DIRECTION('center_axis',(0.433012701892244,0.866025403784463,-0.249999999999873));
#47472=DIRECTION('ref_axis',(1.56781158599937E-14,-0.277350098112484,-0.96076892283056));
#47473=DIRECTION('',(-0.750000000000077,0.499999999999834,0.433012701892277));
#47474=DIRECTION('',(-0.49999999999991,-4.12740234260269E-14,-0.866025403784491));
#47475=DIRECTION('center_axis',(-0.433012701892222,0.866025403784471,0.249999999999885));
#47476=DIRECTION('ref_axis',(-2.1552431563991E-14,0.277350098112477,-0.960768922830563));
#47477=DIRECTION('',(-0.750000000000017,-0.499999999999952,0.433012701892245));
#47478=DIRECTION('',(-0.500000000000001,-4.12740234260327E-14,-0.866025403784438));
#47479=DIRECTION('center_axis',(-0.866025403784462,-5.42497745590479E-14,
0.49999999999996));
#47480=DIRECTION('ref_axis',(6.76186946307289E-14,-1.,8.61946552381525E-15));
#47481=DIRECTION('',(6.76186946307289E-14,-1.,8.61946552381525E-15));
#47482=DIRECTION('center_axis',(1.,6.76186946307289E-14,-2.76820162751211E-15));
#47483=DIRECTION('ref_axis',(-6.76186946307289E-14,1.,-8.61946552381525E-15));
#47484=DIRECTION('',(6.76186946307289E-14,-1.,8.61946552381525E-15));
#47485=DIRECTION('',(3.14120143831326E-14,-0.499999999999871,-0.866025403784513));
#47486=DIRECTION('',(-3.62066802475778E-14,0.499999999999855,-0.866025403784522));
#47487=DIRECTION('',(-6.76186946307289E-14,1.,-8.61946552381525E-15));
#47488=DIRECTION('',(-3.14120143831563E-14,0.500000000000213,0.866025403784315));
#47489=DIRECTION('',(3.62066802476004E-14,-0.500000000000198,0.866025403784324));
#47490=DIRECTION('center_axis',(5.71754065071898E-14,-0.866025403784331,
-0.500000000000186));
#47491=DIRECTION('ref_axis',(3.62066802475997E-14,-0.500000000000186,0.866025403784331));
#47492=DIRECTION('',(3.62066802476004E-14,-0.500000000000198,0.866025403784324));
#47493=DIRECTION('',(1.,6.76186946307289E-14,-2.76820162751211E-15));
#47494=DIRECTION('',(1.,6.76186946307289E-14,-2.76820162751211E-15));
#47495=DIRECTION('center_axis',(5.99436081347026E-14,-0.866025403784325,
0.500000000000197));
#47496=DIRECTION('ref_axis',(-3.14120143831551E-14,0.500000000000197,0.866025403784325));
#47497=DIRECTION('',(-3.14120143831563E-14,0.500000000000213,0.866025403784315));
#47498=DIRECTION('',(1.,6.76186946307289E-14,-2.76820162751211E-15));
#47499=DIRECTION('center_axis',(2.76820162751153E-15,8.61946552381544E-15,
1.));
#47500=DIRECTION('ref_axis',(-6.76186946307289E-14,1.,-8.61946552381525E-15));
#47501=DIRECTION('',(1.,6.76186946307289E-14,-2.76820162751211E-15));
#47502=DIRECTION('',(6.76186946307289E-14,-1.,8.61946552381525E-15));
#47503=DIRECTION('center_axis',(-5.71754065072035E-14,0.866025403784521,
0.499999999999857));
#47504=DIRECTION('ref_axis',(-3.62066802475779E-14,0.499999999999857,-0.866025403784521));
#47505=DIRECTION('',(-3.62066802475778E-14,0.499999999999855,-0.866025403784522));
#47506=DIRECTION('',(1.,6.76186946307289E-14,-2.76820162751211E-15));
#47507=DIRECTION('center_axis',(-5.99436081347142E-14,0.86602540378451,
-0.499999999999877));
#47508=DIRECTION('ref_axis',(3.1412014383133E-14,-0.499999999999877,-0.86602540378451));
#47509=DIRECTION('',(3.14120143831326E-14,-0.499999999999871,-0.866025403784513));
#47510=DIRECTION('',(1.,6.76186946307289E-14,-2.76820162751211E-15));
#47511=DIRECTION('center_axis',(-2.76820162751153E-15,-8.61946552381544E-15,
-1.));
#47512=DIRECTION('ref_axis',(6.76186946307289E-14,-1.,8.61946552381525E-15));
#47513=DIRECTION('',(6.76186946307289E-14,-1.,8.61946552381525E-15));
#47514=DIRECTION('center_axis',(-0.500000000000004,-4.12740234260329E-14,
-0.866025403784436));
#47515=DIRECTION('ref_axis',(6.76186946307289E-14,-1.,8.61946552381525E-15));
#47516=DIRECTION('center_axis',(-0.500000000000004,-3.44554207439535E-14,
-0.866025403784436));
#47517=DIRECTION('ref_axis',(-0.704794021481385,-0.581108581114958,0.406913018025544));
#47518=DIRECTION('center_axis',(0.500000000000014,4.21542315225752E-14,
0.866025403784431));
#47519=DIRECTION('ref_axis',(-0.704794021481382,-0.581108581114953,0.406913018025557));
#47520=DIRECTION('center_axis',(-0.500000000000004,-4.71998124407273E-14,
-0.866025403784436));
#47521=DIRECTION('ref_axis',(0.866025403784436,4.89516451167878E-14,-0.500000000000004));
#47522=DIRECTION('center_axis',(-0.500000000000004,-4.71998124407273E-14,
-0.866025403784436));
#47523=DIRECTION('ref_axis',(0.866025403784436,4.89516451167878E-14,-0.500000000000004));
#47524=DIRECTION('',(-0.851918022522507,-0.410905818312109,-0.324641481296827));
#47525=DIRECTION('center_axis',(0.499999999999998,-1.34221383908382E-14,
0.86602540378444));
#47526=DIRECTION('ref_axis',(0.86602540378444,5.42497745590461E-14,-0.499999999999998));
#47527=DIRECTION('',(-0.499999999999998,1.34221383908382E-14,-0.86602540378444));
#47528=DIRECTION('center_axis',(-0.5000000000008,2.7339420210613E-14,-0.866025403783977));
#47529=DIRECTION('ref_axis',(0.704794021480816,-0.581108581115277,-0.406913018026075));
#47530=DIRECTION('center_axis',(-0.500000000000004,-3.93436929775028E-14,
-0.866025403784436));
#47531=DIRECTION('ref_axis',(0.866025403784436,5.42497745590458E-14,-0.500000000000004));
#47532=DIRECTION('center_axis',(-0.500000000000004,-3.93436929775028E-14,
-0.866025403784436));
#47533=DIRECTION('ref_axis',(0.866025403784436,5.42497745590458E-14,-0.500000000000004));
#47534=DIRECTION('',(0.851918022522704,-0.410905818312444,0.324641481295884));
#47535=DIRECTION('center_axis',(-0.500000000000002,-3.17573814987145E-14,
-0.866025403784437));
#47536=DIRECTION('ref_axis',(-0.866025403784437,1.84782918280226E-14,0.500000000000002));
#47537=DIRECTION('center_axis',(0.500000000000004,4.12740234260329E-14,
0.866025403784436));
#47538=DIRECTION('ref_axis',(-6.76186946307289E-14,1.,-8.61946552381525E-15));
#47539=DIRECTION('center_axis',(1.,6.76186946307289E-14,-2.76820162751211E-15));
#47540=DIRECTION('ref_axis',(-6.76186946307289E-14,1.,-8.61946552381525E-15));
#47541=DIRECTION('center_axis',(1.,6.75541145682558E-14,-2.96977669029757E-15));
#47542=DIRECTION('ref_axis',(3.68393940734127E-14,-0.581108581114928,-0.813826036051068));
#47543=DIRECTION('center_axis',(-1.,-6.78676766814992E-14,-1.7058558528147E-15));
#47544=DIRECTION('ref_axis',(4.08267592067223E-14,-0.581108581114911,-0.81382603605108));
#47545=DIRECTION('center_axis',(1.,6.72875615405878E-14,-2.76820162751211E-15));
#47546=DIRECTION('ref_axis',(2.76820162751153E-15,8.61946552381544E-15,
1.));
#47547=DIRECTION('center_axis',(1.,6.72875615405878E-14,-2.76820162751211E-15));
#47548=DIRECTION('ref_axis',(2.76820162751153E-15,8.61946552381544E-15,
1.));
#47549=DIRECTION('',(0.707106781186583,-0.410905818311995,-0.575461908797881));
#47550=DIRECTION('center_axis',(1.,6.76186946307289E-14,-2.76820162751211E-15));
#47551=DIRECTION('ref_axis',(-6.76186946307289E-14,1.,-8.61946552381525E-15));
#47552=DIRECTION('',(6.76186946307289E-14,-1.,8.61946552381525E-15));
#47553=DIRECTION('',(3.14120143831426E-14,-0.500000000000016,-0.866025403784429));
#47554=DIRECTION('',(-3.62066802475874E-14,0.500000000000001,-0.866025403784438));
#47555=DIRECTION('',(-6.76186946307289E-14,1.,-8.61946552381525E-15));
#47556=DIRECTION('',(-3.14120143831427E-14,0.500000000000017,0.866025403784429));
#47557=DIRECTION('',(3.62066802475875E-14,-0.500000000000002,0.866025403784437));
#47558=DIRECTION('center_axis',(5.71754065071974E-14,-0.866025403784436,
-0.500000000000004));
#47559=DIRECTION('ref_axis',(3.62066802475877E-14,-0.500000000000004,0.866025403784436));
#47560=DIRECTION('',(3.62066802475875E-14,-0.500000000000002,0.866025403784437));
#47561=DIRECTION('',(1.,6.76186946307289E-14,-2.76820162751211E-15));
#47562=DIRECTION('',(1.,6.76186946307289E-14,-2.76820162751211E-15));
#47563=DIRECTION('center_axis',(5.99436081347093E-14,-0.866025403784432,
0.500000000000012));
#47564=DIRECTION('ref_axis',(-3.14120143831423E-14,0.500000000000012,0.866025403784432));
#47565=DIRECTION('',(-3.14120143831427E-14,0.500000000000017,0.866025403784429));
#47566=DIRECTION('',(1.,6.76186946307289E-14,-2.76820162751211E-15));
#47567=DIRECTION('center_axis',(2.76820162751153E-15,8.61946552381544E-15,
1.));
#47568=DIRECTION('ref_axis',(-6.76186946307289E-14,1.,-8.61946552381525E-15));
#47569=DIRECTION('',(1.,6.76186946307289E-14,-2.76820162751211E-15));
#47570=DIRECTION('',(6.76186946307289E-14,-1.,8.61946552381525E-15));
#47571=DIRECTION('center_axis',(-5.71754065071978E-14,0.866025403784442,
0.499999999999995));
#47572=DIRECTION('ref_axis',(-3.6206680247587E-14,0.499999999999995,-0.866025403784442));
#47573=DIRECTION('',(-3.62066802475874E-14,0.500000000000001,-0.866025403784438));
#47574=DIRECTION('',(1.,6.76186946307289E-14,-2.76820162751211E-15));
#47575=DIRECTION('center_axis',(-5.99436081347093E-14,0.866025403784433,
-0.50000000000001));
#47576=DIRECTION('ref_axis',(3.14120143831422E-14,-0.50000000000001,-0.866025403784433));
#47577=DIRECTION('',(3.14120143831426E-14,-0.500000000000016,-0.866025403784429));
#47578=DIRECTION('',(1.,6.76186946307289E-14,-2.76820162751211E-15));
#47579=DIRECTION('center_axis',(-2.76820162751153E-15,-8.61946552381544E-15,
-1.));
#47580=DIRECTION('ref_axis',(6.76186946307289E-14,-1.,8.61946552381525E-15));
#47581=DIRECTION('',(6.76186946307289E-14,-1.,8.61946552381525E-15));
#47582=DIRECTION('center_axis',(-0.500000000000013,-2.63446712046972E-14,
0.866025403784431));
#47583=DIRECTION('ref_axis',(-6.76186946307289E-14,1.,-8.61946552381525E-15));
#47584=DIRECTION('',(6.76186946307289E-14,-1.,8.61946552381525E-15));
#47585=DIRECTION('',(0.750000000000005,-0.499999999999972,0.433012701892242));
#47586=DIRECTION('',(0.749999999999971,0.500000000000053,0.433012701892208));
#47587=DIRECTION('',(-6.76186946307289E-14,1.,-8.61946552381525E-15));
#47588=DIRECTION('',(-0.750000000000011,0.499999999999969,-0.433012701892236));
#47589=DIRECTION('',(-0.749999999999938,-0.500000000000081,-0.433012701892234));
#47590=DIRECTION('center_axis',(0.433012701892257,-0.866025403784422,0.249999999999993));
#47591=DIRECTION('ref_axis',(-1.60944494942364E-14,0.277350098112605,0.960768922830526));
#47592=DIRECTION('',(-0.749999999999961,-0.500000000000034,-0.433012701892248));
#47593=DIRECTION('',(-0.499999999999997,-2.63446712046961E-14,0.86602540378444));
#47594=DIRECTION('',(-0.499999999999907,-2.63446712046895E-14,0.866025403784493));
#47595=DIRECTION('center_axis',(-0.433012701892182,-0.866025403784465,-0.249999999999974));
#47596=DIRECTION('ref_axis',(2.15107982005752E-14,-0.277350098112591,0.96076892283053));
#47597=DIRECTION('',(-0.750000000000039,0.499999999999944,-0.433012701892216));
#47598=DIRECTION('',(-0.499999999999997,-2.63446712046961E-14,0.86602540378444));
#47599=DIRECTION('center_axis',(-0.866025403784437,-6.28692400828612E-14,
-0.500000000000004));
#47600=DIRECTION('ref_axis',(6.76186946307289E-14,-1.,8.61946552381525E-15));
#47601=DIRECTION('',(-0.499999999999997,-2.63446712046961E-14,0.86602540378444));
#47602=DIRECTION('',(6.76186946307289E-14,-1.,8.61946552381525E-15));
#47603=DIRECTION('center_axis',(-0.433012701892302,0.866025403784399,-0.249999999999994));
#47604=DIRECTION('ref_axis',(1.60389383430057E-14,-0.277350098112613,-0.960768922830523));
#47605=DIRECTION('',(0.749999999999971,0.500000000000053,0.433012701892208));
#47606=DIRECTION('',(-0.499999999999907,-2.63446712046895E-14,0.866025403784493));
#47607=DIRECTION('center_axis',(0.433012701892141,0.866025403784476,0.250000000000007));
#47608=DIRECTION('ref_axis',(-2.16079427152319E-14,0.277350098112621,-0.960768922830521));
#47609=DIRECTION('',(0.750000000000027,-0.499999999999986,0.433012701892189));
#47610=DIRECTION('',(-0.499999999999997,-2.63446712046961E-14,0.86602540378444));
#47611=DIRECTION('center_axis',(0.866025403784438,6.28692400828612E-14,
0.500000000000002));
#47612=DIRECTION('ref_axis',(-6.76186946307289E-14,1.,-8.61946552381525E-15));
#47613=DIRECTION('',(6.76186946307289E-14,-1.,8.61946552381525E-15));
#47614=DIRECTION('center_axis',(-0.500000000000015,-3.45211617413146E-14,
0.86602540378443));
#47615=DIRECTION('ref_axis',(-6.77071775113598E-14,1.,7.70846885918756E-16));
#47616=DIRECTION('center_axis',(-0.499999999999998,-2.0534737558427E-14,
0.86602540378444));
#47617=DIRECTION('ref_axis',(0.704794021481457,-0.581108581114873,0.406913018025541));
#47618=DIRECTION('center_axis',(0.500000000000006,2.76649833495093E-14,
-0.866025403784435));
#47619=DIRECTION('ref_axis',(0.704794021481461,-0.581108581114863,0.406913018025548));
#47620=DIRECTION('center_axis',(-0.5,-3.47395389755134E-14,0.866025403784439));
#47621=DIRECTION('ref_axis',(-0.866025403784439,-7.34654989673773E-14,-0.5));
#47622=DIRECTION('center_axis',(-0.5,-3.47395389755134E-14,0.866025403784439));
#47623=DIRECTION('ref_axis',(-0.866025403784439,-7.34654989673773E-14,-0.5));
#47624=DIRECTION('',(0.14481124133601,-0.410905818312037,0.900103390094738));
#47625=DIRECTION('center_axis',(0.500000000000089,-5.99318293989482E-14,
-0.866025403784387));
#47626=DIRECTION('ref_axis',(-0.866025403784387,-6.28692400828585E-14,-0.500000000000089));
#47627=DIRECTION('',(-0.500000000000089,5.99318293989482E-14,0.866025403784387));
#47628=DIRECTION('center_axis',(-0.500000000000155,-4.05319142052322E-14,
0.866025403784349));
#47629=DIRECTION('ref_axis',(-0.704794021481363,-0.581108581114877,-0.406913018025699));
#47630=DIRECTION('center_axis',(-0.499999999999999,-2.67123531948925E-14,
0.866025403784439));
#47631=DIRECTION('ref_axis',(-0.866025403784439,-6.61019093650721E-14,-0.499999999999999));
#47632=DIRECTION('center_axis',(-0.499999999999999,-2.67123531948925E-14,
0.866025403784439));
#47633=DIRECTION('ref_axis',(-0.866025403784439,-6.61019093650721E-14,-0.499999999999999));
#47634=DIRECTION('',(-0.144811241336241,-0.410905818312194,-0.900103390094629));
#47635=DIRECTION('center_axis',(-0.499999999999998,-1.72125400623194E-14,
0.86602540378444));
#47636=DIRECTION('ref_axis',(0.86602540378444,6.28692400828614E-14,0.499999999999998));
#47637=DIRECTION('center_axis',(0.5,2.63446712046963E-14,-0.866025403784439));
#47638=DIRECTION('ref_axis',(6.76186946307289E-14,-1.,8.61946552381525E-15));
#47639=DIRECTION('center_axis',(1.,6.76186946307289E-14,-2.76820162751211E-15));
#47640=DIRECTION('ref_axis',(-6.76186946307289E-14,1.,-8.61946552381525E-15));
#47641=DIRECTION('center_axis',(1.,6.62617941496609E-14,-2.56436653811211E-15));
#47642=DIRECTION('ref_axis',(3.64183489257448E-14,-0.581108581114924,-0.813826036051071));
#47643=DIRECTION('center_axis',(-1.,-6.70346188016559E-14,2.66648801027148E-15));
#47644=DIRECTION('ref_axis',(3.67843348498335E-14,-0.581108581114929,-0.813826036051068));
#47645=DIRECTION('center_axis',(1.,6.72875615405878E-14,-2.76820162751211E-15));
#47646=DIRECTION('ref_axis',(2.76820162751189E-15,3.32133608155747E-15,
1.));
#47647=DIRECTION('center_axis',(1.,6.72875615405878E-14,-2.76820162751211E-15));
#47648=DIRECTION('ref_axis',(2.76820162751189E-15,3.32133608155747E-15,
1.));
#47649=DIRECTION('',(0.707106781186578,-0.410905818312009,-0.575461908797876));
#47650=DIRECTION('center_axis',(-1.,-6.76186946307289E-14,2.76820162751211E-15));
#47651=DIRECTION('ref_axis',(2.76820162751153E-15,8.61946552381544E-15,
1.));
#47652=DIRECTION('',(1.,6.76186946307289E-14,-2.76820162751211E-15));
#47653=DIRECTION('center_axis',(1.,7.70213952838427E-14,-6.44756718319748E-15));
#47654=DIRECTION('ref_axis',(5.00049917717591E-14,-0.581108581114909,0.813826036051082));
#47655=DIRECTION('',(-0.707106781186518,-0.410905818312096,0.575461908797887));
#47656=DIRECTION('center_axis',(1.,6.76186946307289E-14,-2.76820162751211E-15));
#47657=DIRECTION('ref_axis',(-2.76820162751153E-15,-8.61946552381544E-15,
-1.));
#47658=DIRECTION('center_axis',(-1.,-6.76186946307289E-14,2.76820162751211E-15));
#47659=DIRECTION('ref_axis',(6.76186946307289E-14,-1.,8.61946552381525E-15));
#47660=DIRECTION('center_axis',(0.500000000000054,2.69910524079384E-14,
-0.866025403784408));
#47661=DIRECTION('ref_axis',(-0.866025403784408,-6.28692400828597E-14,-0.500000000000054));
#47662=DIRECTION('',(0.500000000000054,2.69910524079384E-14,-0.866025403784408));
#47663=DIRECTION('center_axis',(0.499999999999999,6.67723902414026E-15,
0.866025403784439));
#47664=DIRECTION('ref_axis',(0.866025403784439,5.42497745590461E-14,-0.499999999999999));
#47665=DIRECTION('',(0.499999999999999,6.67723902414026E-15,0.866025403784439));
#47666=DIRECTION('center_axis',(-1.,-6.76186946307289E-14,2.76820162751211E-15));
#47667=DIRECTION('ref_axis',(6.76186946307289E-14,-1.,8.61946552381525E-15));
#47668=DIRECTION('center_axis',(1.,6.76186946307289E-14,-2.76820162751211E-15));
#47669=DIRECTION('ref_axis',(2.76820162751108E-15,1.52311079226398E-14,
1.));
#47670=DIRECTION('center_axis',(1.,9.21118303677479E-14,-3.4270382691727E-14));
#47671=DIRECTION('ref_axis',(8.14171047488604E-14,-0.5811085811149,0.813826036051089));
#47672=DIRECTION('',(-0.707106781186463,-0.41090581831212,0.575461908797939));
#47673=DIRECTION('center_axis',(-1.,-6.76186946307289E-14,2.76820162751211E-15));
#47674=DIRECTION('ref_axis',(2.76820162751153E-15,8.61946552381544E-15,
1.));
#47675=DIRECTION('',(1.,6.76186946307289E-14,-2.76820162751211E-15));
#47676=DIRECTION('center_axis',(6.76186946307289E-14,-1.,8.61946552381525E-15));
#47677=DIRECTION('ref_axis',(2.76820162751153E-15,8.61946552381544E-15,
1.));
#47678=DIRECTION('center_axis',(-6.76186946307289E-14,1.,-8.61946552381525E-15));
#47679=DIRECTION('ref_axis',(1.13162951808259E-15,8.61946552381533E-15,
1.));
#47680=DIRECTION('center_axis',(-6.76186946307289E-14,1.,-8.61946552381525E-15));
#47681=DIRECTION('ref_axis',(1.13162951808259E-15,8.61946552381533E-15,
1.));
#47682=DIRECTION('',(-6.76186946307289E-14,1.,-8.61946552381525E-15));
#47683=DIRECTION('center_axis',(6.72348409290947E-14,-1.,8.67712845096488E-15));
#47684=DIRECTION('ref_axis',(0.581108581114924,4.61324160653485E-14,0.813826036051072));
#47685=DIRECTION('center_axis',(-6.88812930816633E-14,1.,-7.96699432180128E-15));
#47686=DIRECTION('ref_axis',(0.581108581114922,4.65112578961994E-14,0.813826036051073));
#47687=DIRECTION('',(0.290554290557519,-0.866025403784417,0.406913018025541));
#47688=DIRECTION('center_axis',(-2.76820162751153E-15,-8.61946552381544E-15,
-1.));
#47689=DIRECTION('ref_axis',(6.76186946307289E-14,-1.,8.61946552381525E-15));
#47690=DIRECTION('center_axis',(7.36346859522553E-14,-1.,2.89474361586495E-15));
#47691=DIRECTION('ref_axis',(-1.,-7.36346859522553E-14,1.39282431154371E-15));
#47692=DIRECTION('center_axis',(2.76820162751153E-15,8.61946552381544E-15,
1.));
#47693=DIRECTION('ref_axis',(-6.76186946307289E-14,1.,-8.61946552381525E-15));
#47694=DIRECTION('center_axis',(6.76186946307289E-14,-1.,8.61946552381525E-15));
#47695=DIRECTION('ref_axis',(2.76820162751153E-15,8.61946552381544E-15,
1.));
#47696=DIRECTION('center_axis',(-6.76186946307289E-14,1.,-8.61946552381525E-15));
#47697=DIRECTION('ref_axis',(-0.581108581114919,-3.22790582335804E-14,0.813826036051075));
#47698=DIRECTION('',(-6.76186946307289E-14,1.,-8.61946552381525E-15));
#47699=DIRECTION('center_axis',(-6.76186946307289E-14,1.,-8.61946552381525E-15));
#47700=DIRECTION('ref_axis',(-2.76820162751153E-15,-8.61946552381544E-15,
-1.));
#47701=DIRECTION('center_axis',(-6.76186946307289E-14,1.,-8.61946552381525E-15));
#47702=DIRECTION('ref_axis',(-0.581108581114919,-3.22790582335804E-14,0.813826036051075));
#47703=DIRECTION('center_axis',(6.76186946307289E-14,-1.,8.61946552381525E-15));
#47704=DIRECTION('ref_axis',(2.76820162751153E-15,8.61946552381544E-15,
1.));
#47705=DIRECTION('center_axis',(6.76186946307289E-14,-1.,8.61946552381525E-15));
#47706=DIRECTION('ref_axis',(-2.95738450133049E-15,-8.61946552381545E-15,
-1.));
#47707=DIRECTION('center_axis',(-6.76186946307289E-14,1.,-8.61946552381525E-15));
#47708=DIRECTION('ref_axis',(-2.76820162751153E-15,-8.61946552381544E-15,
-1.));
#47709=DIRECTION('',(6.76186946307289E-14,-1.,8.61946552381525E-15));
#47710=DIRECTION('center_axis',(6.76186946307289E-14,-1.,8.61946552381525E-15));
#47711=DIRECTION('ref_axis',(2.76820162751153E-15,8.61946552381544E-15,
1.));
#47712=DIRECTION('',(-6.76186946307289E-14,1.,-8.61946552381525E-15));
#47713=DIRECTION('center_axis',(6.76186946307289E-14,-1.,8.61946552381525E-15));
#47714=DIRECTION('ref_axis',(0.581108581114924,4.63085491538316E-14,0.813826036051072));
#47715=DIRECTION('center_axis',(6.76186946307289E-14,-1.,8.61946552381525E-15));
#47716=DIRECTION('ref_axis',(2.76820162751153E-15,8.61946552381544E-15,
1.));
#47717=DIRECTION('center_axis',(-6.76186946307289E-14,1.,-8.61946552381525E-15));
#47718=DIRECTION('ref_axis',(-2.76820162751153E-15,-8.61946552381544E-15,
-1.));
#47719=DIRECTION('center_axis',(-6.68619631354531E-14,1.,-8.61946552381525E-15));
#47720=DIRECTION('ref_axis',(-3.9032988704253E-15,-8.61946552381551E-15,
-1.));
#47721=DIRECTION('center_axis',(6.76186946307289E-14,-1.,8.61946552381525E-15));
#47722=DIRECTION('ref_axis',(-2.76820162751153E-15,-8.61946552381544E-15,
-1.));
#47723=DIRECTION('',(-6.76186946307289E-14,1.,-8.61946552381525E-15));
#47724=DIRECTION('center_axis',(-6.76186946307289E-14,1.,-8.61946552381525E-15));
#47725=DIRECTION('ref_axis',(-2.76820162751153E-15,-8.61946552381544E-15,
-1.));
#47726=DIRECTION('center_axis',(6.76186946307289E-14,-1.,8.61946552381525E-15));
#47727=DIRECTION('ref_axis',(-0.929667825095055,-6.60383262206023E-14,-0.368398880268426));
#47728=DIRECTION('',(-0.499999999999721,-4.12740234260151E-14,-0.8660254037846));
#47729=DIRECTION('center_axis',(6.76186946307289E-14,-1.,8.61946552381525E-15));
#47730=DIRECTION('ref_axis',(-0.783876701585503,-4.76527508315497E-14,0.620916513479415));
#47731=DIRECTION('',(-1.,-6.76186946307289E-14,2.76820162751211E-15));
#47732=DIRECTION('center_axis',(6.76186946307289E-14,-1.,8.61946552381525E-15));
#47733=DIRECTION('ref_axis',(0.145791123509562,1.83855753890504E-14,0.989315393747525));
#47734=DIRECTION('',(-0.499999999999992,-2.63446712046958E-14,0.866025403784443));
#47735=DIRECTION('center_axis',(6.76186946307289E-14,-1.,8.61946552381525E-15));
#47736=DIRECTION('ref_axis',(0.92966782509514,6.60383262206061E-14,0.368398880268212));
#47737=DIRECTION('',(0.499999999999997,4.12740234260324E-14,0.86602540378444));
#47738=DIRECTION('center_axis',(6.76186946307289E-14,-1.,8.61946552381525E-15));
#47739=DIRECTION('ref_axis',(0.783876701585575,4.76527508315554E-14,-0.620916513479323));
#47740=DIRECTION('',(1.,6.76186946307289E-14,-2.76820162751211E-15));
#47741=DIRECTION('center_axis',(6.76186946307289E-14,-1.,8.61946552381525E-15));
#47742=DIRECTION('ref_axis',(-0.145791123509716,-1.83855753890607E-14,-0.989315393747502));
#47743=DIRECTION('',(0.499999999999717,2.63446712046757E-14,-0.866025403784602));
#47744=DIRECTION('center_axis',(-4.76493972863412E-13,-1.,-2.89681359328052E-13));
#47745=DIRECTION('ref_axis',(-0.735712000031937,5.46761928043604E-13,-0.677294509802794));
#47746=DIRECTION('center_axis',(2.76820162751153E-15,8.61946552381544E-15,
1.));
#47747=DIRECTION('ref_axis',(-6.76186946307289E-14,1.,-8.61946552381525E-15));
#47748=DIRECTION('',(6.76186946307289E-14,-1.,8.61946552381525E-15));
#47749=DIRECTION('',(6.76186946307289E-14,-1.,8.61946552381525E-15));
#47750=DIRECTION('center_axis',(0.866025403784435,7.09853627648186E-14,
0.500000000000007));
#47751=DIRECTION('ref_axis',(-6.75709603676437E-14,1.,-2.49343890566557E-14));
#47752=DIRECTION('',(6.76186946307289E-14,-1.,8.61946552381525E-15));
#47753=DIRECTION('center_axis',(1.0103337148294E-13,-1.,-5.27593924421864E-15));
#47754=DIRECTION('ref_axis',(0.218698251317296,2.72440438071183E-14,-0.975792536798041));
#47755=DIRECTION('center_axis',(-3.69810843763156E-13,-1.,8.6039702248726E-15));
#47756=DIRECTION('ref_axis',(0.95441025134894,-3.55519528484008E-13,-0.298498026995243));
#47757=DIRECTION('center_axis',(3.12821769014316E-13,-1.,5.09998858760493E-13));
#47758=DIRECTION('ref_axis',(0.735712000031524,5.75566156379323E-13,0.677294509803243));
#47759=DIRECTION('center_axis',(6.05237314895677E-13,-1.,7.97499678325301E-15));
#47760=DIRECTION('ref_axis',(-0.954410251348955,-5.75264177030255E-13,0.298498026995197));
#47761=DIRECTION('center_axis',(-1.09246500362634E-13,-1.,-3.34895822000761E-13));
#47762=DIRECTION('ref_axis',(-0.21869825131763,-3.02896825121284E-13,0.975792536797966));
#47763=DIRECTION('center_axis',(-0.866025403784445,-5.42497745590466E-14,
0.499999999999989));
#47764=DIRECTION('ref_axis',(6.76186946307289E-14,-1.,8.61946552381525E-15));
#47765=DIRECTION('',(6.76186946307289E-14,-1.,8.61946552381525E-15));
#47766=DIRECTION('center_axis',(-0.866025403784448,-6.28692400828618E-14,
-0.499999999999984));
#47767=DIRECTION('ref_axis',(6.76186946307289E-14,-1.,8.61946552381525E-15));
#47768=DIRECTION('',(6.76186946307289E-14,-1.,8.61946552381525E-15));
#47769=DIRECTION('center_axis',(-2.76820162751153E-15,-8.61946552381544E-15,
-1.));
#47770=DIRECTION('ref_axis',(6.76186946307289E-14,-1.,8.61946552381525E-15));
#47771=DIRECTION('',(6.76186946307289E-14,-1.,8.61946552381525E-15));
#47772=DIRECTION('center_axis',(0.866025403784432,5.42497745590455E-14,
-0.500000000000011));
#47773=DIRECTION('ref_axis',(6.76186946307289E-14,-1.,8.61946552381525E-15));
#47774=DIRECTION('center_axis',(-6.76186946307289E-14,1.,-8.61946552381525E-15));
#47775=DIRECTION('ref_axis',(-2.76820162751153E-15,-8.61946552381544E-15,
-1.));
#47776=DIRECTION('center_axis',(6.76186946307289E-14,-1.,8.61946552381525E-15));
#47777=DIRECTION('ref_axis',(-0.929667825095138,-6.60383262206061E-14,-0.368398880268217));
#47778=DIRECTION('',(-0.499999999999984,-4.12740234260316E-14,-0.866025403784448));
#47779=DIRECTION('center_axis',(8.99762615155139E-14,-1.,-3.01049762542524E-14));
#47780=DIRECTION('ref_axis',(-0.783876701585578,-8.92229719919505E-14,0.62091651347932));
#47781=DIRECTION('',(-1.,-6.76186946307289E-14,2.76820162751211E-15));
#47782=DIRECTION('center_axis',(4.52611277459437E-14,-1.,-3.01049762542524E-14));
#47783=DIRECTION('ref_axis',(0.145791123509556,-2.3184645771345E-14,0.989315393747526));
#47784=DIRECTION('',(-0.49999999999999,-2.63446712046956E-14,0.866025403784444));
#47785=DIRECTION('center_axis',(6.76186946307289E-14,-1.,8.61946552381525E-15));
#47786=DIRECTION('ref_axis',(0.929667825095135,6.60383262206059E-14,0.368398880268225));
#47787=DIRECTION('',(0.499999999999995,4.12740234260323E-14,0.866025403784441));
#47788=DIRECTION('center_axis',(8.99762615155135E-14,-1.,-3.0104976254252E-14));
#47789=DIRECTION('ref_axis',(0.78387670158558,8.92229719919501E-14,-0.620916513479317));
#47790=DIRECTION('',(1.,6.76186946307289E-14,-2.76820162751211E-15));
#47791=DIRECTION('center_axis',(4.52611277459445E-14,-1.,-3.01049762542512E-14));
#47792=DIRECTION('ref_axis',(-0.145791123509541,2.31846457713444E-14,-0.989315393747528));
#47793=DIRECTION('',(0.49999999999998,2.63446712046948E-14,-0.86602540378445));
#47794=DIRECTION('center_axis',(5.32380487750437E-14,-1.,-1.68089829306692E-14));
#47795=DIRECTION('ref_axis',(-0.735712000031734,-2.77832394877596E-14,-0.677294509803015));
#47796=DIRECTION('center_axis',(2.76820162751153E-15,8.61946552381544E-15,
1.));
#47797=DIRECTION('ref_axis',(-6.76186946307289E-14,1.,-8.61946552381525E-15));
#47798=DIRECTION('',(6.76186946307289E-14,-1.,8.61946552381525E-15));
#47799=DIRECTION('',(6.76186946307289E-14,-1.,8.61946552381525E-15));
#47800=DIRECTION('center_axis',(0.866025403784442,6.28692400828615E-14,
0.499999999999994));
#47801=DIRECTION('ref_axis',(-6.76186946307289E-14,1.,-8.61946552381525E-15));
#47802=DIRECTION('',(6.76186946307289E-14,-1.,8.61946552381525E-15));
#47803=DIRECTION('center_axis',(1.07211551699132E-13,-1.,-6.00968993881945E-14));
#47804=DIRECTION('ref_axis',(0.218698251317293,8.20890847853168E-14,-0.975792536798042));
#47805=DIRECTION('center_axis',(-3.96535780483983E-13,-1.,9.14212791933769E-15));
#47806=DIRECTION('ref_axis',(0.954410251348937,-3.81186721067026E-13,-0.298498026995254));
#47807=DIRECTION('center_axis',(8.58897203906712E-14,-1.,1.09683518814373E-14));
#47808=DIRECTION('ref_axis',(0.735712000031756,7.06189024816738E-14,0.67729450980299));
#47809=DIRECTION('center_axis',(3.00772197614464E-14,-1.,7.50882472388858E-15));
#47810=DIRECTION('ref_axis',(-0.954410251349009,-2.64646375072693E-14,0.298498026995022));
#47811=DIRECTION('center_axis',(1.80859439608356E-14,-1.,6.05685967206475E-14));
#47812=DIRECTION('ref_axis',(-0.218698251317317,5.51470203266801E-14,0.975792536798037));
#47813=DIRECTION('center_axis',(-0.866025403784437,-5.42497745590459E-14,
0.500000000000003));
#47814=DIRECTION('ref_axis',(-6.76186946307289E-14,1.,-8.61946552381525E-15));
#47815=DIRECTION('',(6.76186946307289E-14,-1.,8.61946552381525E-15));
#47816=DIRECTION('center_axis',(-0.86602540378444,-6.28692400828613E-14,
-0.499999999999998));
#47817=DIRECTION('ref_axis',(6.76186946307289E-14,-1.,8.61946552381525E-15));
#47818=DIRECTION('',(6.76186946307289E-14,-1.,8.61946552381525E-15));
#47819=DIRECTION('center_axis',(-2.76820162751153E-15,-8.61946552381544E-15,
-1.));
#47820=DIRECTION('ref_axis',(6.76186946307289E-14,-1.,8.61946552381525E-15));
#47821=DIRECTION('',(6.76186946307289E-14,-1.,8.61946552381525E-15));
#47822=DIRECTION('center_axis',(0.86602540378444,5.42497745590461E-14,-0.499999999999998));
#47823=DIRECTION('ref_axis',(-6.76186946307289E-14,1.,-8.61946552381525E-15));
#47824=DIRECTION('center_axis',(2.76820162751153E-15,8.61946552381544E-15,
1.));
#47825=DIRECTION('ref_axis',(-6.76186946307289E-14,1.,-8.61946552381525E-15));
#47826=DIRECTION('center_axis',(3.53251163457694E-15,1.10051218976555E-14,
1.));
#47827=DIRECTION('ref_axis',(0.581108581114865,0.813826036051113,-1.1009027553969E-14));
#47828=DIRECTION('center_axis',(2.76820162751153E-15,8.61946552381544E-15,
1.));
#47829=DIRECTION('ref_axis',(-6.76186946307289E-14,1.,-8.61946552381525E-15));
#47830=DIRECTION('center_axis',(3.53251163457696E-15,1.10051218976555E-14,
1.));
#47831=DIRECTION('ref_axis',(0.581108581114867,0.813826036051112,-1.1009027553969E-14));
#47832=DIRECTION('center_axis',(2.76820162751153E-15,8.61946552381544E-15,
1.));
#47833=DIRECTION('ref_axis',(-6.76186946307289E-14,1.,-8.61946552381525E-15));
#47834=DIRECTION('center_axis',(-5.26130915768847E-15,9.82566750515049E-15,
1.));
#47835=DIRECTION('ref_axis',(0.581108581114855,0.813826036051121,-4.93899213784198E-15));
#47836=DIRECTION('center_axis',(-2.76820162751153E-15,-8.61946552381544E-15,
-1.));
#47837=DIRECTION('ref_axis',(6.76186946307289E-14,-1.,8.61946552381525E-15));
#47838=DIRECTION('center_axis',(2.76820162751153E-15,8.61946552381544E-15,
1.));
#47839=DIRECTION('ref_axis',(6.11533560663074E-14,-1.,8.61946552381527E-15));
#47840=DIRECTION('',(-2.76820162751153E-15,-8.61946552381544E-15,-1.));
#47841=DIRECTION('center_axis',(-3.69713693691004E-15,8.619465523815E-15,
1.));
#47842=DIRECTION('ref_axis',(6.11533560663074E-14,-1.,8.61946552381523E-15));
#47843=DIRECTION('center_axis',(-2.76820162751153E-15,-8.61946552381544E-15,
-1.));
#47844=DIRECTION('ref_axis',(6.76186946307289E-14,-1.,8.61946552381525E-15));
#47845=DIRECTION('center_axis',(2.76820162751153E-15,8.61946552381544E-15,
1.));
#47846=DIRECTION('ref_axis',(6.11533560663074E-14,-1.,8.61946552381527E-15));
#47847=DIRECTION('',(-2.76820162751153E-15,-8.61946552381544E-15,-1.));
#47848=DIRECTION('center_axis',(-3.69713693691004E-15,8.619465523815E-15,
1.));
#47849=DIRECTION('ref_axis',(6.11533560663074E-14,-1.,8.61946552381523E-15));
#47850=DIRECTION('center_axis',(-2.76820162751153E-15,-8.61946552381544E-15,
-1.));
#47851=DIRECTION('ref_axis',(6.76186946307289E-14,-1.,8.61946552381525E-15));
#47852=DIRECTION('center_axis',(-2.76820162751153E-15,-8.61946552381544E-15,
-1.));
#47853=DIRECTION('ref_axis',(6.84325727377058E-14,-1.,8.61946552381525E-15));
#47854=DIRECTION('',(-2.76820162751153E-15,-8.61946552381544E-15,-1.));
#47855=DIRECTION('center_axis',(-2.76820162751153E-15,-8.61946552381544E-15,
-1.));
#47856=DIRECTION('ref_axis',(6.76186946307289E-14,-1.,8.61946552381525E-15));
#47857=DIRECTION('center_axis',(2.76820162751153E-15,8.61946552381544E-15,
1.));
#47858=DIRECTION('ref_axis',(7.73998566779744E-14,-1.,8.61946552381522E-15));
#47859=DIRECTION('',(-2.76820162751153E-15,-8.61946552381544E-15,-1.));
#47860=DIRECTION('center_axis',(-2.12237939611116E-15,8.61946552381511E-15,
1.));
#47861=DIRECTION('ref_axis',(7.73998566779744E-14,-1.,8.61946552381527E-15));
#47862=DIRECTION('center_axis',(-2.76820162751153E-15,-8.61946552381544E-15,
-1.));
#47863=DIRECTION('ref_axis',(6.76186946307289E-14,-1.,8.61946552381525E-15));
#47864=DIRECTION('center_axis',(2.76820162751153E-15,8.61946552381544E-15,
1.));
#47865=DIRECTION('ref_axis',(7.73998566779744E-14,-1.,8.61946552381522E-15));
#47866=DIRECTION('',(-2.76820162751153E-15,-8.61946552381544E-15,-1.));
#47867=DIRECTION('center_axis',(-2.12237939611116E-15,8.61946552381511E-15,
1.));
#47868=DIRECTION('ref_axis',(7.73998566779744E-14,-1.,8.61946552381527E-15));
#47869=DIRECTION('center_axis',(-2.76820162751153E-15,-8.61946552381544E-15,
-1.));
#47870=DIRECTION('ref_axis',(6.76186946307289E-14,-1.,8.61946552381525E-15));
#47871=DIRECTION('center_axis',(2.76820162751153E-15,8.61946552381544E-15,
1.));
#47872=DIRECTION('ref_axis',(7.73998566779744E-14,-1.,8.61946552381522E-15));
#47873=DIRECTION('',(-2.76820162751153E-15,-8.61946552381544E-15,-1.));
#47874=DIRECTION('center_axis',(-2.12237939611118E-15,8.61946552381511E-15,
1.));
#47875=DIRECTION('ref_axis',(7.73998566779744E-14,-1.,8.61946552381527E-15));
#47876=DIRECTION('center_axis',(-2.76820162751153E-15,-8.61946552381544E-15,
-1.));
#47877=DIRECTION('ref_axis',(6.76186946307289E-14,-1.,8.61946552381525E-15));
#47878=DIRECTION('center_axis',(2.76820162751153E-15,8.61946552381544E-15,
1.));
#47879=DIRECTION('ref_axis',(6.76186946307289E-14,-1.,8.61946552381525E-15));
#47880=DIRECTION('',(-2.76820162751153E-15,-8.61946552381544E-15,-1.));
#47881=DIRECTION('center_axis',(-2.12237939611118E-15,8.61946552381511E-15,
1.));
#47882=DIRECTION('ref_axis',(6.76186946307289E-14,-1.,8.61946552381525E-15));
#47883=DIRECTION('center_axis',(2.76820162751153E-15,8.61946552381544E-15,
1.));
#47884=DIRECTION('ref_axis',(-6.76186946307289E-14,1.,-8.61946552381525E-15));
#47885=DIRECTION('center_axis',(8.99982368058718E-15,2.43000874453087E-14,
1.));
#47886=DIRECTION('ref_axis',(0.160984848484786,0.986956877760285,-2.54319736859329E-14));
#47887=DIRECTION('center_axis',(2.76820162751153E-15,8.61946552381544E-15,
1.));
#47888=DIRECTION('ref_axis',(0.7071067811866,-0.707106781186495,4.13746837958792E-15));
#47889=DIRECTION('',(0.7071067811865,0.707106781186595,-8.05229666459887E-15));
#47890=DIRECTION('center_axis',(-2.0472413176489E-14,6.65582873155231E-15,
1.));
#47891=DIRECTION('ref_axis',(0.578440307445775,0.815724715036904,6.41274497658531E-15));
#47892=DIRECTION('center_axis',(7.02512538336182E-15,1.92786462781398E-14,
1.));
#47893=DIRECTION('ref_axis',(0.142617449664349,0.989777885715395,-2.00834832183795E-14));
#47894=DIRECTION('center_axis',(-1.29309139275503E-14,2.67428077770542E-14,
1.));
#47895=DIRECTION('ref_axis',(-1.,6.4834541425706E-14,-1.2930913927552E-14));
#47896=DIRECTION('',(6.76186946307289E-14,-1.,8.61946552381525E-15));
#47897=DIRECTION('center_axis',(-2.37218282461776E-14,-1.38997923373325E-14,
1.));
#47898=DIRECTION('ref_axis',(-0.160984848484789,-0.986956877760285,-1.75373505727631E-14));
#47899=DIRECTION('center_axis',(-6.76186946307289E-14,1.,-8.61946552381525E-15));
#47900=DIRECTION('ref_axis',(-2.76820162751153E-15,-8.61946552381544E-15,
-1.));
#47901=DIRECTION('',(1.,6.76186946307289E-14,-2.76820162751211E-15));
#47902=DIRECTION('',(2.76820162751153E-15,8.61946552381544E-15,1.));
#47903=DIRECTION('',(1.,6.76186946307289E-14,-2.76820162751211E-15));
#47904=DIRECTION('',(2.76820162751153E-15,8.61946552381544E-15,1.));
#47905=DIRECTION('center_axis',(-2.76820162751153E-15,-8.61946552381544E-15,
-1.));
#47906=DIRECTION('ref_axis',(0.985823585943277,0.1677851524955,-4.17517679239051E-15));
#47907=DIRECTION('center_axis',(2.76820162751153E-15,8.61946552381544E-15,
1.));
#47908=DIRECTION('ref_axis',(0.985823585943276,0.167785152495509,-4.17517679239058E-15));
#47909=DIRECTION('',(2.76820162751153E-15,8.61946552381544E-15,1.));
#47910=DIRECTION('center_axis',(2.76820162751153E-15,8.61946552381544E-15,
1.));
#47911=DIRECTION('ref_axis',(0.985823585943265,0.16778515249557,-4.17517679239108E-15));
#47912=DIRECTION('center_axis',(-2.76820162751153E-15,-8.61946552381544E-15,
-1.));
#47913=DIRECTION('ref_axis',(0.815724610137237,0.578440455376742,-7.24393775608304E-15));
#47914=DIRECTION('center_axis',(2.76820162751153E-15,8.61946552381544E-15,
1.));
#47915=DIRECTION('ref_axis',(0.81572461013724,0.578440455376738,-7.24393775608301E-15));
#47916=DIRECTION('',(2.76820162751153E-15,8.61946552381544E-15,1.));
#47917=DIRECTION('center_axis',(2.76820162751153E-15,8.61946552381544E-15,
1.));
#47918=DIRECTION('ref_axis',(0.81572461013724,0.578440455376738,-7.24393775608301E-15));
#47919=DIRECTION('center_axis',(-2.76820162751153E-15,-8.61946552381544E-15,
-1.));
#47920=DIRECTION('ref_axis',(-0.7071067811866,0.707106781186495,-4.13746837958792E-15));
#47921=DIRECTION('center_axis',(2.76820162751153E-15,8.61946552381544E-15,
1.));
#47922=DIRECTION('ref_axis',(-0.70710678118656,0.707106781186535,-4.13746837958837E-15));
#47923=DIRECTION('',(2.76820162751153E-15,8.61946552381544E-15,1.));
#47924=DIRECTION('center_axis',(2.76820162751153E-15,8.61946552381544E-15,
1.));
#47925=DIRECTION('ref_axis',(-0.707106781186629,0.707106781186466,-4.13746837958759E-15));
#47926=DIRECTION('center_axis',(0.70710678118658,-0.707106781186515,4.13746837958814E-15));
#47927=DIRECTION('ref_axis',(2.76820162751153E-15,8.61946552381544E-15,
1.));
#47928=DIRECTION('',(-0.7071067811865,-0.707106781186595,8.05229666459887E-15));
#47929=DIRECTION('',(2.76820162751153E-15,8.61946552381544E-15,1.));
#47930=DIRECTION('',(-0.7071067811865,-0.707106781186595,8.05229666459887E-15));
#47931=DIRECTION('center_axis',(-2.76820162751153E-15,-8.61946552381544E-15,
-1.));
#47932=DIRECTION('ref_axis',(-0.828230928818615,-0.560386945376366,7.12294616077891E-15));
#47933=DIRECTION('center_axis',(2.76820162751153E-15,8.61946552381544E-15,
1.));
#47934=DIRECTION('ref_axis',(-0.828230928818613,-0.560386945376369,7.12294616077893E-15));
#47935=DIRECTION('',(2.76820162751153E-15,8.61946552381544E-15,1.));
#47936=DIRECTION('center_axis',(2.76820162751153E-15,8.61946552381544E-15,
1.));
#47937=DIRECTION('ref_axis',(-0.828230928818613,-0.560386945376369,7.12294616077893E-15));
#47938=DIRECTION('center_axis',(-2.76820162751153E-15,-8.61946552381544E-15,
-1.));
#47939=DIRECTION('ref_axis',(0.828230715013045,0.560387261372865,-7.12294829264291E-15));
#47940=DIRECTION('center_axis',(2.76820162751153E-15,8.61946552381544E-15,
1.));
#47941=DIRECTION('ref_axis',(0.828230715013044,0.560387261372867,-7.12294829264292E-15));
#47942=DIRECTION('',(2.76820162751153E-15,8.61946552381544E-15,1.));
#47943=DIRECTION('center_axis',(2.76820162751153E-15,8.61946552381544E-15,
1.));
#47944=DIRECTION('ref_axis',(0.828230715013044,0.560387261372867,-7.12294829264292E-15));
#47945=DIRECTION('center_axis',(-2.76820162751153E-15,-8.61946552381544E-15,
-1.));
#47946=DIRECTION('ref_axis',(-1.49010911433646E-8,-1.,8.61946556506466E-15));
#47947=DIRECTION('center_axis',(-2.02627530217484E-14,-1.92783289800561E-14,
1.));
#47948=DIRECTION('ref_axis',(-1.49010911433648E-8,-1.,-1.92783292819933E-14));
#47949=DIRECTION('center_axis',(-2.02627530217484E-14,-1.92783289800561E-14,
1.));
#47950=DIRECTION('ref_axis',(-1.49010911433648E-8,-1.,-1.92783292819933E-14));
#47951=DIRECTION('center_axis',(2.76820162751153E-15,8.61946552381544E-15,
1.));
#47952=DIRECTION('ref_axis',(-6.76186946307289E-14,1.,-8.61946552381525E-15));
#47953=DIRECTION('center_axis',(0.707106781186502,0.707106781186593,-8.05229666459886E-15));
#47954=DIRECTION('ref_axis',(-2.76820162751153E-15,-8.61946552381544E-15,
-1.));
#47955=DIRECTION('',(0.707106781186597,-0.707106781186498,4.13746837958795E-15));
#47956=DIRECTION('',(2.76820162751153E-15,8.61946552381544E-15,1.));
#47957=DIRECTION('',(0.707106781186597,-0.707106781186498,4.13746837958795E-15));
#47958=DIRECTION('',(2.76820162751153E-15,8.61946552381544E-15,1.));
#47959=DIRECTION('center_axis',(-2.76820162751153E-15,-8.61946552381544E-15,
-1.));
#47960=DIRECTION('ref_axis',(0.815724561786183,-0.578440523562051,2.72775809088321E-15));
#47961=DIRECTION('center_axis',(4.73183590111844E-15,-1.46211561682312E-14,
1.));
#47962=DIRECTION('ref_axis',(0.8157245617862,-0.578440523562027,-1.23173439959179E-14));
#47963=DIRECTION('',(2.76820162751153E-15,8.61946552381544E-15,1.));
#47964=DIRECTION('center_axis',(8.04567353904598E-16,3.18600872158624E-14,
1.));
#47965=DIRECTION('ref_axis',(0.815724561786194,-0.578440523562036,1.77728601776843E-14));
#47966=DIRECTION('center_axis',(-2.76820162751153E-15,-8.61946552381544E-15,
-1.));
#47967=DIRECTION('ref_axis',(0.985823571918322,-0.167785234899263,-1.28273936860405E-15));
#47968=DIRECTION('center_axis',(2.76820162751153E-15,8.61946552381544E-15,
1.));
#47969=DIRECTION('ref_axis',(0.985823571918322,-0.167785234899264,-1.28273936860404E-15));
#47970=DIRECTION('',(2.76820162751153E-15,8.61946552381544E-15,1.));
#47971=DIRECTION('center_axis',(1.46062076622723E-14,3.71600285032592E-15,
1.));
#47972=DIRECTION('ref_axis',(0.985823571918322,-0.167785234899264,-1.37756533986737E-14));
#47973=DIRECTION('center_axis',(-2.76820162751153E-15,-8.61946552381544E-15,
-1.));
#47974=DIRECTION('ref_axis',(-1.49013091640289E-8,1.,-8.61946548256561E-15));
#47975=DIRECTION('center_axis',(2.76820162751153E-15,8.61946552381544E-15,
1.));
#47976=DIRECTION('ref_axis',(-1.49012263807535E-8,1.,-8.61946548256584E-15));
#47977=DIRECTION('',(2.76820162751153E-15,8.61946552381544E-15,1.));
#47978=DIRECTION('center_axis',(2.76820162751153E-15,8.61946552381544E-15,
1.));
#47979=DIRECTION('ref_axis',(-1.49012263807535E-8,1.,-8.61946548256584E-15));
#47980=DIRECTION('center_axis',(6.76186946307289E-14,-1.,8.61946552381525E-15));
#47981=DIRECTION('ref_axis',(2.76820162751153E-15,8.61946552381544E-15,
1.));
#47982=DIRECTION('',(-1.,-6.76186946307289E-14,2.76820162751211E-15));
#47983=DIRECTION('',(2.76820162751153E-15,8.61946552381544E-15,1.));
#47984=DIRECTION('',(-1.,-6.76186946307289E-14,2.76820162751211E-15));
#47985=DIRECTION('center_axis',(-2.76820162751153E-15,-8.61946552381544E-15,
-1.));
#47986=DIRECTION('ref_axis',(-0.981901142050496,0.189394158410264,1.08562392065031E-15));
#47987=DIRECTION('center_axis',(2.57991596261325E-14,-1.92783397979622E-14,
1.));
#47988=DIRECTION('ref_axis',(-0.981901142050477,0.18939415841036,2.89834292424261E-14));
#47989=DIRECTION('',(2.76820162751153E-15,8.61946552381544E-15,1.));
#47990=DIRECTION('center_axis',(2.5799159626134E-14,-1.92783397979624E-14,
1.));
#47991=DIRECTION('ref_axis',(-0.981901142050477,0.189394158410364,2.89834292424276E-14));
#47992=DIRECTION('center_axis',(-2.76820162751153E-15,-8.61946552381544E-15,
-1.));
#47993=DIRECTION('ref_axis',(0.981901186307147,-0.189393928964519,-1.08562602086133E-15));
#47994=DIRECTION('center_axis',(-1.51165338862552E-14,1.60275656363945E-14,
1.));
#47995=DIRECTION('ref_axis',(0.981901186307147,-0.189393928964522,1.78784661833796E-14));
#47996=DIRECTION('',(2.76820162751153E-15,8.61946552381544E-15,1.));
#47997=DIRECTION('center_axis',(-3.30012694000219E-14,2.34356657489735E-14,
1.));
#47998=DIRECTION('ref_axis',(0.981901186307147,-0.189393928964522,3.68425583876206E-14));
#47999=DIRECTION('center_axis',(-2.92006984084315E-15,-8.46759731048387E-15,
-1.));
#48000=DIRECTION('ref_axis',(-0.707106781186433,-0.707106781186662,8.05229666459926E-15));
#48001=DIRECTION('center_axis',(3.87802855472544E-14,1.2060850989616E-14,
1.));
#48002=DIRECTION('ref_axis',(-0.707106781186464,-0.707106781186631,3.59501124084499E-14));
#48003=DIRECTION('center_axis',(3.87802855472544E-14,1.20608509896159E-14,
1.));
#48004=DIRECTION('ref_axis',(-0.707106781186467,-0.707106781186628,3.595011240845E-14));
#48005=DIRECTION('center_axis',(2.76820162751153E-15,8.61946552381544E-15,
1.));
#48006=DIRECTION('ref_axis',(-6.76186946307289E-14,1.,-8.61946552381525E-15));
#48007=DIRECTION('center_axis',(1.,6.76186946307289E-14,-2.76820162751211E-15));
#48008=DIRECTION('ref_axis',(-6.76186946307289E-14,1.,-8.61946552381525E-15));
#48009=DIRECTION('',(6.76186946307289E-14,-1.,8.61946552381525E-15));
#48010=DIRECTION('',(2.76820162751153E-15,8.61946552381544E-15,1.));
#48011=DIRECTION('',(6.76186946307289E-14,-1.,8.61946552381525E-15));
#48012=DIRECTION('',(2.76820162751153E-15,8.61946552381544E-15,1.));
#48013=DIRECTION('center_axis',(-2.76820162751153E-15,-8.61946552381544E-15,
-1.));
#48014=DIRECTION('ref_axis',(0.142617449664331,-0.989777885715397,8.13656250588646E-15));
#48015=DIRECTION('center_axis',(-1.29309139275495E-14,-9.50387672942742E-15,
1.));
#48016=DIRECTION('ref_axis',(0.142617449664151,-0.989777885715423,-7.56255304917892E-15));
#48017=DIRECTION('',(2.76820162751153E-15,8.61946552381544E-15,1.));
#48018=DIRECTION('center_axis',(2.76820162751153E-15,8.61946552381544E-15,
1.));
#48019=DIRECTION('ref_axis',(0.142617449664151,-0.989777885715423,8.13656250588718E-15));
#48020=DIRECTION('center_axis',(-2.76820162751153E-15,-8.61946552381544E-15,
-1.));
#48021=DIRECTION('ref_axis',(0.578440455376734,-0.815724610137243,5.42987034401337E-15));
#48022=DIRECTION('center_axis',(7.02512529519986E-15,-2.03971490112667E-15,
1.));
#48023=DIRECTION('ref_axis',(0.578440455376738,-0.81572461013724,-5.72746231734672E-15));
#48024=DIRECTION('',(2.76820162751153E-15,8.61946552381544E-15,1.));
#48025=DIRECTION('center_axis',(-1.4887220401768E-15,1.92786459487576E-14,
1.));
#48026=DIRECTION('ref_axis',(0.578440455376738,-0.81572461013724,1.65872030053734E-14));
#48027=DIRECTION('center_axis',(-2.76820162751153E-15,-8.61946552381544E-15,
-1.));
#48028=DIRECTION('ref_axis',(0.707106781186598,0.707106781186497,-8.0522966645983E-15));
#48029=DIRECTION('center_axis',(7.2490060184047E-14,2.72856031906688E-15,
1.));
#48030=DIRECTION('ref_axis',(0.707106781186564,0.707106781186531,-5.31875966292505E-14));
#48031=DIRECTION('',(2.76820162751153E-15,8.61946552381544E-15,1.));
#48032=DIRECTION('center_axis',(2.60088211463569E-14,6.65583045556597E-15,
1.));
#48033=DIRECTION('ref_axis',(0.707106781186583,0.707106781186512,-2.30973966528164E-14));
#48034=DIRECTION('center_axis',(-0.707106781186506,-0.707106781186589,8.05229666459883E-15));
#48035=DIRECTION('ref_axis',(2.76820162751153E-15,8.61946552381544E-15,
1.));
#48036=DIRECTION('',(-0.707106781186597,0.707106781186498,-4.13746837958795E-15));
#48037=DIRECTION('',(2.76820162751153E-15,8.61946552381544E-15,1.));
#48038=DIRECTION('',(-0.707106781186588,0.707106781186507,-4.13746837958805E-15));
#48039=DIRECTION('center_axis',(-2.76820162751153E-15,-8.61946552381544E-15,
-1.));
#48040=DIRECTION('ref_axis',(-0.560387030549914,0.828230871189579,-5.58764314997358E-15));
#48041=DIRECTION('center_axis',(-6.73179990625715E-16,-2.73926102301024E-14,
1.));
#48042=DIRECTION('ref_axis',(-0.560387030549925,0.828230871189572,2.23101640990617E-14));
#48043=DIRECTION('',(2.76820162751153E-15,8.61946552381544E-15,1.));
#48044=DIRECTION('center_axis',(-6.73179990625995E-16,-2.73926102301055E-14,
1.));
#48045=DIRECTION('ref_axis',(-0.560387030549879,0.828230871189603,2.2310164099065E-14));
#48046=DIRECTION('center_axis',(-2.76820162751153E-15,-8.61946552381544E-15,
-1.));
#48047=DIRECTION('ref_axis',(0.560387257316999,-0.828230717757276,5.58764119973211E-15));
#48048=DIRECTION('center_axis',(2.76820162751153E-15,8.61946552381544E-15,
1.));
#48049=DIRECTION('ref_axis',(0.560387257316998,-0.828230717757276,5.58764119973212E-15));
#48050=DIRECTION('',(2.76820162751153E-15,8.61946552381544E-15,1.));
#48051=DIRECTION('center_axis',(2.76820162751153E-15,8.61946552381544E-15,
1.));
#48052=DIRECTION('ref_axis',(0.560387257316998,-0.828230717757276,5.58764119973212E-15));
#48053=DIRECTION('center_axis',(-2.76820162751153E-15,-8.61946552381544E-15,
-1.));
#48054=DIRECTION('ref_axis',(-1.,-6.34795310039648E-14,2.76820162751208E-15));
#48055=DIRECTION('center_axis',(2.76820162751153E-15,8.61946552381544E-15,
1.));
#48056=DIRECTION('ref_axis',(-1.,-2.00183129229455E-14,2.7682016275117E-15));
#48057=DIRECTION('center_axis',(-2.37218282461825E-14,3.11387233849614E-14,
1.));
#48058=DIRECTION('ref_axis',(-1.,-2.00183129229458E-14,-2.37218282461819E-14));
#48059=DIRECTION('center_axis',(2.76820162751153E-15,8.61946552381544E-15,
1.));
#48060=DIRECTION('ref_axis',(-6.76186946307289E-14,1.,-8.61946552381525E-15));
#48061=DIRECTION('center_axis',(2.76820162751153E-15,8.61946552381544E-15,
1.));
#48062=DIRECTION('ref_axis',(-6.76186946307289E-14,1.,-8.61946552381525E-15));
#48063=DIRECTION('',(2.76820162751153E-15,8.61946552381544E-15,1.));
#48064=DIRECTION('center_axis',(-2.76820162751153E-15,-8.61946552381544E-15,
-1.));
#48065=DIRECTION('ref_axis',(-0.581108581114972,0.813826036051037,-5.40611974012191E-15));
#48066=DIRECTION('center_axis',(2.99566356165988E-15,8.72176871572695E-15,
1.));
#48067=DIRECTION('ref_axis',(-6.76186946307289E-14,1.,-8.72176871572675E-15));
#48068=DIRECTION('',(2.99566356165988E-15,8.72176871572695E-15,1.));
#48069=DIRECTION('center_axis',(-2.76820162751153E-15,-8.61946552381544E-15,
-1.));
#48070=DIRECTION('ref_axis',(-0.581108581114972,0.813826036051037,-5.40611974012191E-15));
#48071=DIRECTION('center_axis',(2.71915890354096E-15,8.72176871572693E-15,
1.));
#48072=DIRECTION('ref_axis',(-6.76186946307289E-14,1.,-8.72176871572675E-15));
#48073=DIRECTION('',(2.71915890354096E-15,8.72176871572693E-15,1.));
#48074=DIRECTION('center_axis',(-2.76820162751153E-15,-8.61946552381544E-15,
-1.));
#48075=DIRECTION('ref_axis',(-0.581108581114971,0.813826036051038,-5.40611974012192E-15));
#48076=DIRECTION('center_axis',(-2.76820162751153E-15,-8.61946552381544E-15,
-1.));
#48077=DIRECTION('ref_axis',(0.715652996595046,0.698456003241816,-8.00138922975266E-15));
#48078=DIRECTION('center_axis',(1.20008912487007E-15,8.61946552381533E-15,
1.));
#48079=DIRECTION('ref_axis',(0.71856952465566,0.695455130282421,-6.85679899083214E-15));
#48080=DIRECTION('center_axis',(0.999390826289479,-5.82068180765387E-7,
-0.0348995175911332));
#48081=DIRECTION('ref_axis',(0.0348985180651857,-0.00755166584133485,0.999362329578154));
#48082=DIRECTION('center_axis',(1.21617314918329E-15,8.61946552381533E-15,
1.));
#48083=DIRECTION('ref_axis',(0.715652996595047,0.698456003241815,-6.89067539843613E-15));
#48084=DIRECTION('center_axis',(0.999390826289723,5.81873952209323E-7,-0.0348995175841439));
#48085=DIRECTION('ref_axis',(0.0348985217095042,0.00753783529609301,0.999362433865482));
#48086=DIRECTION('center_axis',(2.76820162751153E-15,8.61946552381544E-15,
1.));
#48087=DIRECTION('ref_axis',(-6.76186946307289E-14,1.,-8.61946552381525E-15));
#48088=DIRECTION('',(6.76186946307289E-14,-1.,8.61946552381525E-15));
#48089=DIRECTION('center_axis',(-2.76820162751153E-15,-8.61946552381544E-15,
-1.));
#48090=DIRECTION('ref_axis',(-0.338105122691879,0.941108349771433,-7.17590782412406E-15));
#48091=DIRECTION('center_axis',(2.76820162751206E-15,7.35344329979148E-16,
1.));
#48092=DIRECTION('ref_axis',(-0.329874263976707,0.944024877832055,2.18975133141604E-16));
#48093=DIRECTION('center_axis',(1.50207726725875E-6,0.999390821854869,-0.0348996445539642));
#48094=DIRECTION('ref_axis',(-0.995051211909553,0.00346924114795279,0.0993028199155812));
#48095=DIRECTION('center_axis',(2.76820162751153E-15,8.61946552381544E-15,
1.));
#48096=DIRECTION('ref_axis',(-0.338105122691878,0.941108349771433,-7.17590782412407E-15));
#48097=DIRECTION('center_axis',(-1.50215001892545E-6,0.999390821854616,
-0.0348996445611993));
#48098=DIRECTION('ref_axis',(0.995316427551229,0.00337526453063588,0.0966116796045264));
#48099=DIRECTION('center_axis',(2.76820162751153E-15,8.61946552381544E-15,
1.));
#48100=DIRECTION('ref_axis',(-6.76186946307289E-14,1.,-8.61946552381525E-15));
#48101=DIRECTION('',(1.,6.76186946307289E-14,-2.76820162751211E-15));
#48102=DIRECTION('center_axis',(-2.76820162751153E-15,-8.61946552381544E-15,
-1.));
#48103=DIRECTION('ref_axis',(-0.715652996595035,-0.698456003241827,8.00138922975273E-15));
#48104=DIRECTION('center_axis',(-0.999390826288683,-5.82701798186421E-7,
-0.0348995176139201));
#48105=DIRECTION('ref_axis',(-0.0348985190951373,-0.00754783375989079,0.999362358491903));
#48106=DIRECTION('center_axis',(4.33631413015298E-15,8.61946552381554E-15,
1.));
#48107=DIRECTION('ref_axis',(-0.718569524655658,-0.695455130282423,9.11039470209163E-15));
#48108=DIRECTION('center_axis',(-0.999390826289037,5.82420313152883E-7,
-0.0348995176037821));
#48109=DIRECTION('ref_axis',(-0.034898520434395,0.00754272883685878,0.999362396987791));
#48110=DIRECTION('center_axis',(2.76820162751153E-15,8.61946552381544E-15,
1.));
#48111=DIRECTION('ref_axis',(-0.715652996595031,-0.69845600324183,8.00138922975275E-15));
#48112=DIRECTION('center_axis',(2.76820162751153E-15,8.61946552381544E-15,
1.));
#48113=DIRECTION('ref_axis',(-6.76186946307289E-14,1.,-8.61946552381525E-15));
#48114=DIRECTION('',(-6.76186946307289E-14,1.,-8.61946552381525E-15));
#48115=DIRECTION('center_axis',(2.76820162751153E-15,8.61946552381544E-15,
1.));
#48116=DIRECTION('ref_axis',(-6.76186946307289E-14,1.,-8.61946552381525E-15));
#48117=DIRECTION('',(-1.,-6.76186946307289E-14,2.76820162751211E-15));
#48118=DIRECTION('',(6.76186946307289E-14,-1.,8.61946552381525E-15));
#48119=DIRECTION('center_axis',(-2.02835435550342E-15,3.82290954079985E-15,
1.));
#48120=DIRECTION('ref_axis',(-6.56318960898822E-14,1.,-3.82290954079999E-15));
#48121=DIRECTION('',(1.,6.6593023648202E-14,-2.7682016275121E-15));
#48122=DIRECTION('',(-6.76186946307289E-14,1.,-8.61946552381525E-15));
#48123=DIRECTION('center_axis',(-7.79286212482761E-15,-1.36441260211324E-14,
-1.));
#48124=DIRECTION('ref_axis',(-1.,-8.20575921431216E-14,7.79286212482873E-15));
#48125=DIRECTION('center_axis',(2.76820162751153E-15,8.61946552381544E-15,
1.));
#48126=DIRECTION('ref_axis',(-6.76186946307289E-14,1.,-8.61946552381525E-15));
#48127=DIRECTION('',(1.,6.76186946307289E-14,-2.76820162751211E-15));
#48128=DIRECTION('center_axis',(-2.76820162751153E-15,-8.61946552381544E-15,
-1.));
#48129=DIRECTION('ref_axis',(-5.72122820091847E-14,1.,-8.61946552381528E-15));
#48130=DIRECTION('',(-6.76186946307289E-14,1.,-8.61946552381525E-15));
#48131=DIRECTION('',(-1.,-6.76186946307289E-14,2.76820162751211E-15));
#48132=DIRECTION('center_axis',(2.76820162751153E-15,8.61946552381544E-15,
1.));
#48133=DIRECTION('ref_axis',(1.,6.96054931715756E-14,-2.76820162751213E-15));
#48134=DIRECTION('',(6.76186946307289E-14,-1.,8.61946552381525E-15));
#48135=DIRECTION('center_axis',(2.76820162751153E-15,8.61946552381544E-15,
1.));
#48136=DIRECTION('ref_axis',(-6.76186946307289E-14,1.,-8.61946552381525E-15));
#48137=DIRECTION('',(6.76186946307289E-14,-1.,8.61946552381525E-15));
#48138=DIRECTION('center_axis',(-2.76820162751153E-15,-8.61946552381544E-15,
-1.));
#48139=DIRECTION('ref_axis',(1.,5.72122820091843E-14,-2.76820162751202E-15));
#48140=DIRECTION('',(1.,6.76186946307289E-14,-2.76820162751211E-15));
#48141=DIRECTION('',(-6.76186946307289E-14,1.,-8.61946552381525E-15));
#48142=DIRECTION('center_axis',(7.56475761052649E-15,1.3416021506831E-14,
1.));
#48143=DIRECTION('ref_axis',(6.56318960898822E-14,-1.,1.34160215068305E-14));
#48144=DIRECTION('',(-1.,-6.76186946307289E-14,2.76820162751211E-15));
#48145=DIRECTION('center_axis',(3.16808364362118E-15,-7.7277101918449E-15,
-1.));
#48146=DIRECTION('ref_axis',(-0.581108581114974,0.813826036051036,-8.13001234417858E-15));
#48147=DIRECTION('center_axis',(2.99361242701923E-14,-6.76685568622446E-16,
1.));
#48148=DIRECTION('ref_axis',(0.581108581114944,-0.813826036051057,-1.7946843032697E-14));
#48149=DIRECTION('center_axis',(2.76820162751153E-15,8.61946552381544E-15,
1.));
#48150=DIRECTION('ref_axis',(6.57847267468704E-14,-1.,8.61946552381526E-15));
#48151=DIRECTION('',(0.0101417431417703,-0.0142032227503904,-0.999847695156392));
#48152=DIRECTION('center_axis',(2.76820162751153E-15,8.61946552381544E-15,
1.));
#48153=DIRECTION('ref_axis',(-6.39448049203062E-14,1.,-8.61946552381526E-15));
#48154=DIRECTION('center_axis',(2.76820162751153E-15,8.61946552381544E-15,
1.));
#48155=DIRECTION('ref_axis',(-6.39448049203062E-14,1.,-8.61946552381526E-15));
#48156=DIRECTION('center_axis',(-0.500000000000034,0.499999999999961,-0.707106781186551));
#48157=DIRECTION('ref_axis',(5.400078907659E-14,-0.81649658092773,-0.577350269189619));
#48158=DIRECTION('',(0.809436869760785,-0.0204932255811562,-0.586849198327085));
#48159=DIRECTION('',(-0.0204932255813507,0.809436869760778,0.586849198327087));
#48160=DIRECTION('',(0.707106781186508,0.707106781186587,-8.05229666459882E-15));
#48161=DIRECTION('center_axis',(0.499999999999975,0.500000000000019,-0.707106781186552));
#48162=DIRECTION('ref_axis',(5.34456775642777E-14,-0.816496580927735,-0.577350269189613));
#48163=DIRECTION('',(0.809436869760787,0.0204932255812656,0.586849198327078));
#48164=DIRECTION('',(0.707106781186619,-0.707106781186476,4.1374683795877E-15));
#48165=DIRECTION('',(-0.020493225581152,-0.809436869760773,-0.586849198327101));
#48166=DIRECTION('center_axis',(-0.499999999999967,-0.500000000000045,-0.707106781186539));
#48167=DIRECTION('ref_axis',(5.67531437763696E-14,-0.816496580927717,0.577350269189638));
#48168=DIRECTION('',(0.020493225581241,0.809436869760761,-0.586849198327114));
#48169=DIRECTION('',(-0.809436869760783,-0.0204932255812548,0.586849198327084));
#48170=DIRECTION('',(-0.707106781186604,0.707106781186491,-4.13746837958787E-15));
#48171=DIRECTION('center_axis',(0.500000000000041,-0.499999999999962,-0.707106781186545));
#48172=DIRECTION('ref_axis',(5.68364105032171E-14,-0.816496580927727,0.577350269189624));
#48173=DIRECTION('',(-0.809436869760727,0.0204932255811478,-0.586849198327164));
#48174=DIRECTION('',(0.0204932255812648,-0.809436869760761,0.586849198327114));
#48175=DIRECTION('',(-0.707106781186518,-0.707106781186577,8.05229666459876E-15));
#48176=DIRECTION('center_axis',(0.999390827019098,6.78783181575812E-14,
0.0348994967024421));
#48177=DIRECTION('ref_axis',(-6.76186946307289E-14,1.,-8.61946552381525E-15));
#48178=DIRECTION('',(6.76186946307289E-14,-1.,8.61946552381525E-15));
#48179=DIRECTION('',(6.76186946307289E-14,-1.,8.61946552381525E-15));
#48180=DIRECTION('',(-0.034899496702468,6.254356368018E-15,0.999390827019097));
#48181=DIRECTION('',(0.0348994967024809,-8.11584534007077E-15,-0.999390827019096));
#48182=DIRECTION('',(6.76186946307289E-14,-1.,8.61946552381525E-15));
#48183=DIRECTION('',(-0.0348994967024809,6.25435636801712E-15,0.999390827019096));
#48184=DIRECTION('',(-0.034899496702468,6.254356368018E-15,0.999390827019097));
#48185=DIRECTION('center_axis',(1.10105900386719E-14,4.42832088979503E-14,
1.));
#48186=DIRECTION('ref_axis',(-0.144919489023215,0.98944345048176,-4.22200819281441E-14));
#48187=DIRECTION('',(4.06656903582202E-16,0.0348994967025038,0.999390827019096));
#48188=DIRECTION('center_axis',(7.56475761052712E-15,3.82290954080049E-15,
1.));
#48189=DIRECTION('ref_axis',(-1.,-6.66252953603055E-14,7.56475761052737E-15));
#48190=DIRECTION('center_axis',(6.7674111992527E-14,-0.999390827019096,
0.0348994967025072));
#48191=DIRECTION('ref_axis',(4.06656903581971E-16,0.0348994967025072,0.999390827019096));
#48192=DIRECTION('',(-1.,-6.76186946307289E-14,2.76820162751211E-15));
#48193=DIRECTION('',(-1.,-6.76186946307289E-14,2.76820162751211E-15));
#48194=DIRECTION('',(-4.06656903581526E-16,-0.0348994967025138,-0.999390827019095));
#48195=DIRECTION('',(-1.,-6.76186946307289E-14,2.76820162751211E-15));
#48196=DIRECTION('',(4.06656903581526E-16,0.0348994967025138,0.999390827019095));
#48197=DIRECTION('',(4.06656903581634E-16,0.0348994967025122,0.999390827019095));
#48198=DIRECTION('center_axis',(3.34855224867282E-15,8.43325952165753E-15,
1.));
#48199=DIRECTION('ref_axis',(0.989443450481758,0.144919489023225,-4.53534675172414E-15));
#48200=DIRECTION('',(0.0348994967024996,1.09740731886008E-14,0.999390827019096));
#48201=DIRECTION('center_axis',(-2.02835435550348E-15,3.82290954079984E-15,
1.));
#48202=DIRECTION('ref_axis',(-6.16582990081887E-14,1.,-3.82290954079997E-15));
#48203=DIRECTION('center_axis',(-0.999390827019096,-6.72766881403301E-14,
0.0348994967025019));
#48204=DIRECTION('ref_axis',(6.76186946307289E-14,-1.,8.61946552381525E-15));
#48205=DIRECTION('',(-6.76186946307289E-14,1.,-8.61946552381525E-15));
#48206=DIRECTION('',(-6.76186946307289E-14,1.,-8.61946552381525E-15));
#48207=DIRECTION('',(-0.0348994967025063,-1.09740731886012E-14,-0.999390827019096));
#48208=DIRECTION('',(-6.76186946307289E-14,1.,-8.61946552381525E-15));
#48209=DIRECTION('',(0.0348994967025063,1.28355621606549E-14,0.999390827019096));
#48210=DIRECTION('',(6.76186946307289E-14,-1.,8.61946552381525E-15));
#48211=DIRECTION('',(0.0348994967025071,1.09740731886013E-14,0.999390827019096));
#48212=DIRECTION('center_axis',(4.9279827061289E-15,1.80927121643866E-14,
1.));
#48213=DIRECTION('ref_axis',(0.144919489023234,-0.989443450481757,1.71875548168164E-14));
#48214=DIRECTION('center_axis',(2.25645886980557E-15,-1.36441260211317E-14,
-1.));
#48215=DIRECTION('ref_axis',(7.80251072522735E-14,-1.,1.36441260211319E-14));
#48216=DIRECTION('',(5.12637372416654E-15,-0.034899496702487,0.999390827019096));
#48217=DIRECTION('center_axis',(7.56475761052717E-15,3.82290954080049E-15,
1.));
#48218=DIRECTION('ref_axis',(1.,7.34549153444662E-14,-7.56475761052745E-15));
#48219=DIRECTION('center_axis',(-6.74808943053846E-14,0.999390827019096,
0.0348994967024958));
#48220=DIRECTION('ref_axis',(-5.12637372416713E-15,0.0348994967024958,-0.999390827019096));
#48221=DIRECTION('',(1.,6.76186946307289E-14,-2.76820162751211E-15));
#48222=DIRECTION('center_axis',(3.48068716811668E-13,-0.999390827019095,
-0.0348994967025218));
#48223=DIRECTION('ref_axis',(-0.995316427483098,-0.00337375605847328,0.0966117329952275));
#48224=DIRECTION('',(-1.,-6.76186946307289E-14,2.76820162751211E-15));
#48225=DIRECTION('center_axis',(-2.01883415239548E-13,-0.999390827019095,
-0.0348994967025223));
#48226=DIRECTION('ref_axis',(0.995051211981761,-0.00346773269898284,0.0993028718797044));
#48227=DIRECTION('',(1.,6.76186946307289E-14,-2.76820162751211E-15));
#48228=DIRECTION('',(-1.,-6.76186946307289E-14,2.76820162751211E-15));
#48229=DIRECTION('',(-5.1263737241671E-15,0.0348994967024954,-0.999390827019096));
#48230=DIRECTION('',(1.,6.76186946307289E-14,-2.76820162751211E-15));
#48231=DIRECTION('',(5.1263737241671E-15,-0.0348994967024954,0.999390827019096));
#48232=DIRECTION('',(5.12637372416711E-15,-0.0348994967024956,0.999390827019096));
#48233=DIRECTION('center_axis',(3.8368846416151E-14,-1.48709733737763E-16,
1.));
#48234=DIRECTION('ref_axis',(-0.989443450481756,-0.144919489023242,3.7942252850375E-14));
#48235=DIRECTION('center_axis',(-2.02835435550344E-15,3.82290954079982E-15,
1.));
#48236=DIRECTION('ref_axis',(6.16582990081887E-14,-1.,3.82290954079995E-15));
#48237=DIRECTION('center_axis',(2.76820162751153E-15,8.61946552381544E-15,
1.));
#48238=DIRECTION('ref_axis',(-6.76186946307289E-14,1.,-8.61946552381525E-15));
#48239=DIRECTION('',(6.76186946307289E-14,-1.,8.61946552381525E-15));
#48240=DIRECTION('',(6.76186946307289E-14,-1.,8.61946552381525E-15));
#48241=DIRECTION('center_axis',(7.56475761052712E-15,3.8229095408005E-15,
1.));
#48242=DIRECTION('ref_axis',(-1.,-6.87362688099551E-14,7.56475761052739E-15));
#48243=DIRECTION('',(1.,6.76186946307289E-14,-2.76820162751211E-15));
#48244=DIRECTION('',(1.,6.76186946307289E-14,-2.76820162751211E-15));
#48245=DIRECTION('center_axis',(-2.02835435550342E-15,3.82290954079985E-15,
1.));
#48246=DIRECTION('ref_axis',(6.76186946307289E-14,-1.,3.82290954079999E-15));
#48247=DIRECTION('',(-6.76186946307289E-14,1.,-8.61946552381525E-15));
#48248=DIRECTION('',(-6.76186946307289E-14,1.,-8.61946552381525E-15));
#48249=DIRECTION('center_axis',(2.76820162751153E-15,8.61946552381544E-15,
1.));
#48250=DIRECTION('ref_axis',(1.,6.76186946307289E-14,-2.76820162751211E-15));
#48251=DIRECTION('',(-1.,-6.76186946307289E-14,2.76820162751211E-15));
#48252=DIRECTION('',(-1.,-6.76186946307289E-14,2.76820162751211E-15));
#48253=DIRECTION('center_axis',(-2.02835435550342E-15,3.82290954079985E-15,
1.));
#48254=DIRECTION('ref_axis',(-6.56318960898822E-14,1.,-3.82290954079999E-15));
#48255=DIRECTION('center_axis',(-1.,-6.76186946307289E-14,2.76820162751211E-15));
#48256=DIRECTION('ref_axis',(6.76186946307289E-14,-1.,8.61946552381525E-15));
#48257=DIRECTION('',(-6.76186946307289E-14,1.,-8.61946552381525E-15));
#48258=DIRECTION('',(-2.76820162751153E-15,-8.61946552381544E-15,-1.));
#48259=DIRECTION('center_axis',(4.40730523866621E-15,1.04820891558594E-14,
1.));
#48260=DIRECTION('ref_axis',(-6.56318960898822E-14,1.,-1.04820891558591E-14));
#48261=DIRECTION('center_axis',(7.56475761052712E-15,3.8229095408005E-15,
1.));
#48262=DIRECTION('ref_axis',(-1.,-6.87362688099551E-14,7.56475761052739E-15));
#48263=DIRECTION('',(-2.76820162751153E-15,-8.61946552381544E-15,-1.));
#48264=DIRECTION('center_axis',(-6.76186946307289E-14,1.,-8.61946552381525E-15));
#48265=DIRECTION('ref_axis',(-2.76820162751153E-15,-8.61946552381544E-15,
-1.));
#48266=DIRECTION('',(1.,6.76186946307289E-14,-2.76820162751211E-15));
#48267=DIRECTION('center_axis',(6.76186946307289E-14,-1.,8.61946552381525E-15));
#48268=DIRECTION('ref_axis',(2.76820162751153E-15,8.61946552381544E-15,
1.));
#48269=DIRECTION('',(-2.76820162751153E-15,-8.61946552381544E-15,-1.));
#48270=DIRECTION('center_axis',(2.76820162751153E-15,8.61946552381544E-15,
1.));
#48271=DIRECTION('ref_axis',(-1.,-6.86120939011522E-14,2.76820162751212E-15));
#48272=DIRECTION('',(-2.76820162751153E-15,-8.61946552381544E-15,-1.));
#48273=DIRECTION('center_axis',(-1.,-6.76186946307289E-14,2.76820162751211E-15));
#48274=DIRECTION('ref_axis',(6.76186946307289E-14,-1.,8.61946552381525E-15));
#48275=DIRECTION('center_axis',(1.,6.76186946307289E-14,-2.76820162751211E-15));
#48276=DIRECTION('ref_axis',(-6.76186946307289E-14,1.,-8.61946552381525E-15));
#48277=DIRECTION('',(-2.76820162751153E-15,-8.61946552381544E-15,-1.));
#48278=DIRECTION('center_axis',(2.76820162751153E-15,8.61946552381544E-15,
1.));
#48279=DIRECTION('ref_axis',(6.76186946307289E-14,-1.,8.61946552381525E-15));
#48280=DIRECTION('',(-2.76820162751153E-15,-8.61946552381544E-15,-1.));
#48281=DIRECTION('center_axis',(6.76186946307289E-14,-1.,8.61946552381525E-15));
#48282=DIRECTION('ref_axis',(2.76820162751153E-15,8.61946552381544E-15,
1.));
#48283=DIRECTION('center_axis',(-6.65967751777163E-14,1.,-8.61946552381525E-15));
#48284=DIRECTION('ref_axis',(-2.76820162751153E-15,-8.61946552381544E-15,
-1.));
#48285=DIRECTION('',(-2.76820162751153E-15,-8.61946552381544E-15,-1.));
#48286=DIRECTION('center_axis',(2.76820162751152E-15,8.84298554470447E-15,
1.));
#48287=DIRECTION('ref_axis',(1.,6.83637440835464E-14,-2.76820162751212E-15));
#48288=DIRECTION('',(-2.76820162751153E-15,-8.61946552381544E-15,-1.));
#48289=DIRECTION('center_axis',(1.,6.76186946307289E-14,-2.76820162751211E-15));
#48290=DIRECTION('ref_axis',(-6.76186946307289E-14,1.,-8.61946552381525E-15));
#48291=DIRECTION('center_axis',(2.76820162751153E-15,8.61946552381544E-15,
1.));
#48292=DIRECTION('ref_axis',(-6.76186946307289E-14,1.,-8.61946552381525E-15));
#48293=DIRECTION('center_axis',(-2.76820162751153E-15,-8.61946552381544E-15,
-1.));
#48294=DIRECTION('ref_axis',(0.338105122691878,-0.941108349771433,7.17590782412407E-15));
#48295=DIRECTION('center_axis',(2.76820162751206E-15,7.35344329979309E-16,
1.));
#48296=DIRECTION('ref_axis',(0.329874263976713,-0.944024877832053,-2.18975133141472E-16));
#48297=DIRECTION('center_axis',(2.76820162751153E-15,8.61946552381544E-15,
1.));
#48298=DIRECTION('ref_axis',(0.338105122691879,-0.941108349771433,7.17590782412406E-15));
#48299=DIRECTION('center_axis',(2.76820162751153E-15,8.61946552381544E-15,
1.));
#48300=DIRECTION('ref_axis',(-6.76186946307289E-14,1.,-8.61946552381525E-15));
#48301=DIRECTION('center_axis',(-2.76820162751153E-15,-8.61946552381544E-15,
-1.));
#48302=DIRECTION('ref_axis',(6.76186946307289E-14,-1.,8.61946552381525E-15));
#48303=DIRECTION('center_axis',(2.76820162751153E-15,8.61946552381544E-15,
1.));
#48304=DIRECTION('ref_axis',(1.83515276180121E-13,-1.,8.61946552381493E-15));
#48305=DIRECTION('',(2.76820162751153E-15,8.61946552381544E-15,1.));
#48306=DIRECTION('center_axis',(2.76820162751153E-15,8.61946552381544E-15,
1.));
#48307=DIRECTION('ref_axis',(1.17288658151894E-13,-1.,8.61946552381511E-15));
#48308=DIRECTION('',(2.76820162751153E-15,8.61946552381544E-15,1.));
#48309=DIRECTION('center_axis',(-6.76186946307289E-14,1.,-8.61946552381525E-15));
#48310=DIRECTION('ref_axis',(-2.76820162751153E-15,-8.61946552381544E-15,
-1.));
#48311=DIRECTION('',(1.,6.76186946307289E-14,-2.76820162751211E-15));
#48312=DIRECTION('',(2.76820162751153E-15,8.61946552381544E-15,1.));
#48313=DIRECTION('',(1.,6.76186946307289E-14,-2.76820162751211E-15));
#48314=DIRECTION('center_axis',(-2.76820162751153E-15,-8.61946552381544E-15,
-1.));
#48315=DIRECTION('ref_axis',(0.981901184295549,-0.189393939393524,-1.08562592540037E-15));
#48316=DIRECTION('center_axis',(-2.02627523364964E-14,3.65172596209946E-14,
1.));
#48317=DIRECTION('ref_axis',(0.981901184295513,-0.189393939393713,2.68121681717756E-14));
#48318=DIRECTION('',(2.76820162751153E-15,8.61946552381544E-15,1.));
#48319=DIRECTION('center_axis',(-2.02627523364964E-14,3.65172596209946E-14,
1.));
#48320=DIRECTION('ref_axis',(0.981901184295513,-0.189393939393713,2.68121681717756E-14));
#48321=DIRECTION('center_axis',(-2.76820162751153E-15,-8.61946552381544E-15,
-1.));
#48322=DIRECTION('ref_axis',(-0.981901184295477,0.1893939393939,1.08562592539693E-15));
#48323=DIRECTION('center_axis',(2.76820162751153E-15,8.61946552381544E-15,
1.));
#48324=DIRECTION('ref_axis',(-0.981901184295475,0.189393939393907,1.08562592539687E-15));
#48325=DIRECTION('',(2.76820162751153E-15,8.61946552381544E-15,1.));
#48326=DIRECTION('center_axis',(-1.51165366653243E-14,1.60275666842004E-14,
1.));
#48327=DIRECTION('ref_axis',(-0.981901184295476,0.189393939393906,-1.78784692473471E-14));
#48328=DIRECTION('center_axis',(-2.76820162751153E-15,-8.61946552381544E-15,
-1.));
#48329=DIRECTION('ref_axis',(0.707106781186593,0.707106781186502,-8.05229666459833E-15));
#48330=DIRECTION('center_axis',(3.87802647389425E-14,1.20608411849333E-14,
1.));
#48331=DIRECTION('ref_axis',(0.707106781186678,0.707106781186417,-3.59500907617996E-14));
#48332=DIRECTION('',(2.76820162751153E-15,8.61946552381544E-15,1.));
#48333=DIRECTION('center_axis',(2.76820162751153E-15,8.61946552381544E-15,
1.));
#48334=DIRECTION('ref_axis',(0.707106781186678,0.707106781186417,-8.05229666459783E-15));
#48335=DIRECTION('center_axis',(-0.707106781186549,-0.707106781186546,8.05229666459858E-15));
#48336=DIRECTION('ref_axis',(2.76820162751153E-15,8.61946552381544E-15,
1.));
#48337=DIRECTION('',(-0.707106781186631,0.707106781186464,-4.13746837958756E-15));
#48338=DIRECTION('',(2.76820162751153E-15,8.61946552381544E-15,1.));
#48339=DIRECTION('',(-0.707106781186631,0.707106781186464,-4.13746837958756E-15));
#48340=DIRECTION('center_axis',(-2.76820162751153E-15,-8.61946552381544E-15,
-1.));
#48341=DIRECTION('ref_axis',(-0.815724561786088,0.578440523562185,-2.72775809088462E-15));
#48342=DIRECTION('center_axis',(2.76820162751153E-15,8.61946552381544E-15,
1.));
#48343=DIRECTION('ref_axis',(-0.815724561786174,0.578440523562064,-2.72775809088334E-15));
#48344=DIRECTION('',(2.76820162751153E-15,8.61946552381544E-15,1.));
#48345=DIRECTION('center_axis',(2.76820162751153E-15,8.61946552381544E-15,
1.));
#48346=DIRECTION('ref_axis',(-0.815724561786174,0.578440523562064,-2.72775809088334E-15));
#48347=DIRECTION('center_axis',(-2.76820162751153E-15,-8.61946552381544E-15,
-1.));
#48348=DIRECTION('ref_axis',(-0.985823571918317,0.167785234899295,1.28273936860376E-15));
#48349=DIRECTION('center_axis',(1.4606207662274E-14,3.71600285032521E-15,
1.));
#48350=DIRECTION('ref_axis',(-0.985823571918316,0.167785234899296,1.37756533986753E-14));
#48351=DIRECTION('center_axis',(2.76820162751153E-15,8.61946552381544E-15,
1.));
#48352=DIRECTION('ref_axis',(-0.985823571918316,0.167785234899296,1.28273936860375E-15));
#48353=DIRECTION('center_axis',(2.76820162751153E-15,8.61946552381544E-15,
1.));
#48354=DIRECTION('ref_axis',(-6.76186946307289E-14,1.,-8.61946552381525E-15));
#48355=DIRECTION('center_axis',(0.70710678118645,0.707106781186645,-8.05229666459916E-15));
#48356=DIRECTION('ref_axis',(-2.76820162751153E-15,-8.61946552381544E-15,
-1.));
#48357=DIRECTION('',(0.707106781186554,-0.707106781186541,4.13746837958844E-15));
#48358=DIRECTION('',(2.76820162751153E-15,8.61946552381544E-15,1.));
#48359=DIRECTION('',(0.707106781186554,-0.707106781186541,4.13746837958844E-15));
#48360=DIRECTION('',(2.76820162751153E-15,8.61946552381544E-15,1.));
#48361=DIRECTION('center_axis',(-2.76820162751153E-15,-8.61946552381544E-15,
-1.));
#48362=DIRECTION('ref_axis',(0.560387247009387,-0.828230724731485,5.58764128837962E-15));
#48363=DIRECTION('center_axis',(-6.73174033601705E-16,-2.73925975876096E-14,
1.));
#48364=DIRECTION('ref_axis',(0.560387247009324,-0.828230724731527,-2.23101528088168E-14));
#48365=DIRECTION('',(2.76820162751153E-15,8.61946552381544E-15,1.));
#48366=DIRECTION('center_axis',(2.76820162751153E-15,8.61946552381544E-15,
1.));
#48367=DIRECTION('ref_axis',(0.560387247009278,-0.828230724731558,5.58764128838055E-15));
#48368=DIRECTION('center_axis',(-2.76820162751153E-15,-8.61946552381544E-15,
-1.));
#48369=DIRECTION('ref_axis',(-0.560387247009416,0.828230724731465,-5.58764128837936E-15));
#48370=DIRECTION('center_axis',(-3.46342042556553E-15,2.43000874453061E-14,
1.));
#48371=DIRECTION('ref_axis',(-0.560387247009403,0.828230724731474,-2.20669356733829E-14));
#48372=DIRECTION('',(2.76820162751153E-15,8.61946552381544E-15,1.));
#48373=DIRECTION('center_axis',(2.76820162751153E-15,8.61946552381544E-15,
1.));
#48374=DIRECTION('ref_axis',(-0.560387247009409,0.82823072473147,-5.58764128837942E-15));
#48375=DIRECTION('center_axis',(-2.76820162751153E-15,-8.61946552381544E-15,
-1.));
#48376=DIRECTION('ref_axis',(1.,6.76186946307289E-14,-2.76820162751211E-15));
#48377=DIRECTION('center_axis',(-2.37218282461811E-14,3.11387233849611E-14,
1.));
#48378=DIRECTION('ref_axis',(1.,3.86445492433809E-14,2.37218282461799E-14));
#48379=DIRECTION('',(2.76820162751153E-15,8.61946552381544E-15,1.));
#48380=DIRECTION('center_axis',(-2.37218282461811E-14,3.11387233849611E-14,
1.));
#48381=DIRECTION('ref_axis',(1.,3.86445492433809E-14,2.37218282461799E-14));
#48382=DIRECTION('center_axis',(-1.,-6.76186946307289E-14,2.76820162751211E-15));
#48383=DIRECTION('ref_axis',(6.76186946307289E-14,-1.,8.61946552381525E-15));
#48384=DIRECTION('',(-6.76186946307289E-14,1.,-8.61946552381525E-15));
#48385=DIRECTION('',(2.76820162751153E-15,8.61946552381544E-15,1.));
#48386=DIRECTION('',(-6.76186946307289E-14,1.,-8.61946552381525E-15));
#48387=DIRECTION('center_axis',(-2.76820162751153E-15,-8.61946552381544E-15,
-1.));
#48388=DIRECTION('ref_axis',(-0.14261736693024,0.989777897636579,-8.13656283766531E-15));
#48389=DIRECTION('center_axis',(-1.293091612144E-14,-9.50387773154572E-15,
1.));
#48390=DIRECTION('ref_axis',(-0.142617366930127,0.989777897636595,7.56255491129047E-15));
#48391=DIRECTION('',(2.76820162751153E-15,8.61946552381544E-15,1.));
#48392=DIRECTION('center_axis',(-1.293091612144E-14,-9.50387773154572E-15,
1.));
#48393=DIRECTION('ref_axis',(-0.142617366930127,0.989777897636595,7.56255491129047E-15));
#48394=DIRECTION('center_axis',(-2.76820162751153E-15,-8.61946552381544E-15,
-1.));
#48395=DIRECTION('ref_axis',(-0.578440455376734,0.815724610137243,-5.42987034401337E-15));
#48396=DIRECTION('center_axis',(2.76820162751153E-15,8.61946552381544E-15,
1.));
#48397=DIRECTION('ref_axis',(-0.578440455376735,0.815724610137242,-5.42987034401336E-15));
#48398=DIRECTION('',(2.76820162751153E-15,8.61946552381544E-15,1.));
#48399=DIRECTION('center_axis',(2.76820162751153E-15,8.61946552381544E-15,
1.));
#48400=DIRECTION('ref_axis',(-0.578440455376735,0.815724610137242,-5.42987034401336E-15));
#48401=DIRECTION('center_axis',(-2.76820162751153E-15,-8.61946552381544E-15,
-1.));
#48402=DIRECTION('ref_axis',(-0.707106781186599,-0.707106781186496,8.05229666459829E-15));
#48403=DIRECTION('center_axis',(2.76820162751153E-15,8.61946552381544E-15,
1.));
#48404=DIRECTION('ref_axis',(-0.707106781186148,-0.707106781186947,8.05229666460093E-15));
#48405=DIRECTION('center_axis',(2.76820162751153E-15,8.61946552381544E-15,
1.));
#48406=DIRECTION('ref_axis',(-0.707106781186148,-0.707106781186947,8.05229666460093E-15));
#48407=DIRECTION('center_axis',(2.76820162751153E-15,8.61946552381544E-15,
1.));
#48408=DIRECTION('ref_axis',(-6.76186946307289E-14,1.,-8.61946552381525E-15));
#48409=DIRECTION('center_axis',(-2.76820162751153E-15,-8.61946552381544E-15,
-1.));
#48410=DIRECTION('ref_axis',(-0.815724610137212,-0.578440455376777,7.24393775608327E-15));
#48411=DIRECTION('center_axis',(-9.06980458537594E-15,3.71600279897938E-15,
1.));
#48412=DIRECTION('ref_axis',(-0.815724610137216,-0.578440455376772,-5.24897645820353E-15));
#48413=DIRECTION('',(2.76820162751153E-15,8.61946552381544E-15,1.));
#48414=DIRECTION('center_axis',(-9.06980458537584E-15,3.7160027989794E-15,
1.));
#48415=DIRECTION('ref_axis',(-0.815724610137217,-0.578440455376771,-5.24897645820345E-15));
#48416=DIRECTION('',(2.76820162751153E-15,8.61946552381544E-15,1.));
#48417=DIRECTION('center_axis',(-2.76820162751153E-15,-8.61946552381544E-15,
-1.));
#48418=DIRECTION('ref_axis',(0.707106781186686,-0.707106781186409,4.13746837958694E-15));
#48419=DIRECTION('center_axis',(8.04566559262691E-16,-1.46211539950285E-14,
1.));
#48420=DIRECTION('ref_axis',(0.707106781186663,-0.707106781186432,-1.09076316086264E-14));
#48421=DIRECTION('',(2.76820162751153E-15,8.61946552381544E-15,1.));
#48422=DIRECTION('center_axis',(4.73183669576037E-15,3.18600850426594E-14,
1.));
#48423=DIRECTION('ref_axis',(0.707106781186663,-0.707106781186432,1.91825683678008E-14));
#48424=DIRECTION('center_axis',(-0.707106781186641,0.707106781186454,-4.13746837958745E-15));
#48425=DIRECTION('ref_axis',(-2.76820162751153E-15,-8.61946552381544E-15,
-1.));
#48426=DIRECTION('',(0.707106781186536,0.707106781186559,-8.05229666459866E-15));
#48427=DIRECTION('',(2.76820162751153E-15,8.61946552381544E-15,1.));
#48428=DIRECTION('',(0.707106781186536,0.707106781186559,-8.05229666459866E-15));
#48429=DIRECTION('center_axis',(-2.76820162751153E-15,-8.61946552381544E-15,
-1.));
#48430=DIRECTION('ref_axis',(0.82823072473152,0.560387247009334,-7.12294819573965E-15));
#48431=DIRECTION('center_axis',(3.87802647389429E-14,5.17808986270238E-15,
1.));
#48432=DIRECTION('ref_axis',(0.828230724731499,0.560387247009366,-3.50207422929409E-14));
#48433=DIRECTION('',(2.76820162751153E-15,8.61946552381544E-15,1.));
#48434=DIRECTION('center_axis',(7.47923278503742E-14,1.73671420158932E-15,
1.));
#48435=DIRECTION('ref_axis',(0.828230724731499,0.560387247009366,-6.2918536390142E-14));
#48436=DIRECTION('center_axis',(-2.76820162751153E-15,-8.61946552381544E-15,
-1.));
#48437=DIRECTION('ref_axis',(-0.828230724731476,-0.560387247009399,7.12294819574009E-15));
#48438=DIRECTION('center_axis',(2.76820162751153E-15,8.61946552381544E-15,
1.));
#48439=DIRECTION('ref_axis',(-0.828230724731477,-0.560387247009398,7.12294819574008E-15));
#48440=DIRECTION('',(2.76820162751153E-15,8.61946552381544E-15,1.));
#48441=DIRECTION('center_axis',(2.06529399203462E-14,1.60275666842028E-14,
1.));
#48442=DIRECTION('ref_axis',(-0.828230724731477,-0.560387247009398,2.6087043368484E-14));
#48443=DIRECTION('center_axis',(-2.76820162751153E-15,-8.61946552381544E-15,
-1.));
#48444=DIRECTION('ref_axis',(-6.76186946307289E-14,1.,-8.61946552381525E-15));
#48445=DIRECTION('center_axis',(2.57991555915155E-14,3.6517259620996E-14,
1.));
#48446=DIRECTION('ref_axis',(-3.32525166743677E-13,1.,-3.65172596209874E-14));
#48447=DIRECTION('',(2.76820162751153E-15,8.61946552381544E-15,1.));
#48448=DIRECTION('center_axis',(2.76820162751153E-15,8.61946552381544E-15,
1.));
#48449=DIRECTION('ref_axis',(-3.32525166743677E-13,1.,-8.61946552381452E-15));
#48450=DIRECTION('center_axis',(6.76186946307289E-14,-1.,8.61946552381525E-15));
#48451=DIRECTION('ref_axis',(2.76820162751153E-15,8.61946552381544E-15,
1.));
#48452=DIRECTION('',(-1.,-6.76186946307289E-14,2.76820162751211E-15));
#48453=DIRECTION('',(2.76820162751153E-15,8.61946552381544E-15,1.));
#48454=DIRECTION('',(-1.,-6.76186946307289E-14,2.76820162751211E-15));
#48455=DIRECTION('center_axis',(-2.76820162751153E-15,-8.61946552381544E-15,
-1.));
#48456=DIRECTION('ref_axis',(-0.985823571918217,-0.167785234899881,4.17517746384804E-15));
#48457=DIRECTION('center_axis',(2.0590300960797E-14,-6.42563446439966E-15,
1.));
#48458=DIRECTION('ref_axis',(-0.98582357191831,-0.167785234899333,1.92202774520594E-14));
#48459=DIRECTION('center_axis',(2.76820162751153E-15,8.61946552381544E-15,
1.));
#48460=DIRECTION('ref_axis',(-0.985823571918306,-0.167785234899355,4.17517746384375E-15));
#48461=DIRECTION('center_axis',(2.76820162751153E-15,8.61946552381544E-15,
1.));
#48462=DIRECTION('ref_axis',(-6.76186946307289E-14,1.,-8.61946552381525E-15));
#48463=DIRECTION('center_axis',(-2.76820162751153E-15,-8.61946552381544E-15,
-1.));
#48464=DIRECTION('ref_axis',(-0.142617449664351,-0.989777885715394,8.92615021843118E-15));
#48465=DIRECTION('center_axis',(7.02512529519804E-15,1.92786459487573E-14,
1.));
#48466=DIRECTION('ref_axis',(-0.142617449664345,-0.989777885715395,2.00834828797903E-14));
#48467=DIRECTION('',(2.76820162751153E-15,8.61946552381544E-15,1.));
#48468=DIRECTION('center_axis',(7.02512529519795E-15,1.92786459487572E-14,
1.));
#48469=DIRECTION('ref_axis',(-0.142617449664338,-0.989777885715396,2.00834828797902E-14));
#48470=DIRECTION('',(2.76820162751153E-15,8.61946552381544E-15,1.));
#48471=DIRECTION('center_axis',(-2.76820162751153E-15,-8.61946552381544E-15,
-1.));
#48472=DIRECTION('ref_axis',(1.,4.27837128701397E-14,-2.7682016275119E-15));
#48473=DIRECTION('center_axis',(2.76820162751153E-15,8.61946552381544E-15,
1.));
#48474=DIRECTION('ref_axis',(1.,-1.04156595879955E-13,-2.76820162751063E-15));
#48475=DIRECTION('',(2.76820162751153E-15,8.61946552381544E-15,1.));
#48476=DIRECTION('center_axis',(2.76820162751153E-15,8.61946552381544E-15,
1.));
#48477=DIRECTION('ref_axis',(1.,-1.04156595879955E-13,-2.76820162751063E-15));
#48478=DIRECTION('center_axis',(-1.,-6.76186946307289E-14,2.76820162751211E-15));
#48479=DIRECTION('ref_axis',(6.76186946307289E-14,-1.,8.61946552381525E-15));
#48480=DIRECTION('',(-6.76186946307289E-14,1.,-8.61946552381525E-15));
#48481=DIRECTION('',(2.76820162751153E-15,8.61946552381544E-15,1.));
#48482=DIRECTION('',(-6.76186946307289E-14,1.,-8.61946552381525E-15));
#48483=DIRECTION('center_axis',(-2.76820162751153E-15,-8.61946552381544E-15,
-1.));
#48484=DIRECTION('ref_axis',(0.160984739080998,0.986956895605387,-8.95267915189108E-15));
#48485=DIRECTION('center_axis',(2.76820162751153E-15,8.61946552381544E-15,
1.));
#48486=DIRECTION('ref_axis',(0.160984739081009,0.986956895605385,-8.9526791518911E-15));
#48487=DIRECTION('',(2.76820162751153E-15,8.61946552381544E-15,1.));
#48488=DIRECTION('center_axis',(2.76820162751153E-15,8.61946552381544E-15,
1.));
#48489=DIRECTION('ref_axis',(0.160984739080975,0.986956895605391,-8.95267915189105E-15));
#48490=DIRECTION('center_axis',(-2.76820162751153E-15,-8.61946552381544E-15,
-1.));
#48491=DIRECTION('ref_axis',(-0.160984853694478,-0.98695687691052,8.95267930802455E-15));
#48492=DIRECTION('center_axis',(2.76820162751153E-15,8.61946552381544E-15,
1.));
#48493=DIRECTION('ref_axis',(-0.160984853694478,-0.98695687691052,8.95267930802455E-15));
#48494=DIRECTION('',(2.76820162751153E-15,8.61946552381544E-15,1.));
#48495=DIRECTION('center_axis',(2.76820162751153E-15,8.61946552381544E-15,
1.));
#48496=DIRECTION('ref_axis',(-0.16098485369447,-0.986956876910521,8.95267930802453E-15));
#48497=DIRECTION('center_axis',(-2.76820162751153E-15,-8.61946552381544E-15,
-1.));
#48498=DIRECTION('ref_axis',(-0.707106781186625,0.70710678118647,-4.13746837958763E-15));
#48499=DIRECTION('center_axis',(2.76820162751153E-15,8.61946552381544E-15,
1.));
#48500=DIRECTION('ref_axis',(-0.707106781186618,0.707106781186477,-4.13746837958771E-15));
#48501=DIRECTION('',(2.76820162751153E-15,8.61946552381544E-15,1.));
#48502=DIRECTION('center_axis',(-6.73183838288935E-16,4.46315494435653E-14,
1.));
#48503=DIRECTION('ref_axis',(-0.707106781186618,0.707106781186477,-3.20352841234439E-14));
#48504=DIRECTION('center_axis',(0.707106781186635,-0.70710678118646,4.13746837958752E-15));
#48505=DIRECTION('ref_axis',(2.76820162751153E-15,8.61946552381544E-15,
1.));
#48506=DIRECTION('',(-0.707106781186539,-0.707106781186556,8.05229666459864E-15));
#48507=DIRECTION('',(2.76820162751153E-15,8.61946552381544E-15,1.));
#48508=DIRECTION('',(-0.707106781186539,-0.707106781186556,8.05229666459864E-15));
#48509=DIRECTION('center_axis',(-2.76820162751153E-15,-8.61946552381544E-15,
-1.));
#48510=DIRECTION('ref_axis',(-0.578440455376605,-0.815724610137334,8.63234996399857E-15));
#48511=DIRECTION('center_axis',(2.76820162751153E-15,8.61946552381544E-15,
1.));
#48512=DIRECTION('ref_axis',(-0.57844045537632,-0.815724610137536,8.63234996399952E-15));
#48513=DIRECTION('center_axis',(2.76820162751153E-15,8.61946552381544E-15,
1.));
#48514=DIRECTION('ref_axis',(-0.57844045537632,-0.815724610137536,8.63234996399952E-15));
#48515=DIRECTION('center_axis',(2.76820162751153E-15,8.61946552381544E-15,
1.));
#48516=DIRECTION('ref_axis',(-6.76186946307289E-14,1.,-8.61946552381525E-15));
#48517=DIRECTION('center_axis',(-2.76820162751153E-15,-8.61946552381544E-15,
-1.));
#48518=DIRECTION('ref_axis',(0.160984848484789,0.986956877760285,-8.95267930092759E-15));
#48519=DIRECTION('center_axis',(2.76820162751153E-15,8.61946552381544E-15,
1.));
#48520=DIRECTION('ref_axis',(0.160984848484786,0.986956877760285,-8.95267930092759E-15));
#48521=DIRECTION('',(2.76820162751153E-15,8.61946552381544E-15,1.));
#48522=DIRECTION('',(2.76820162751153E-15,8.61946552381544E-15,1.));
#48523=DIRECTION('center_axis',(-2.76820162751153E-15,-8.61946552381544E-15,
-1.));
#48524=DIRECTION('ref_axis',(-0.160984848484817,-0.98695687776028,8.95267930092763E-15));
#48525=DIRECTION('center_axis',(2.76820162751153E-15,8.61946552381544E-15,
1.));
#48526=DIRECTION('ref_axis',(-0.160984848484789,-0.986956877760285,8.95267930092759E-15));
#48527=DIRECTION('',(2.76820162751153E-15,8.61946552381544E-15,1.));
#48528=DIRECTION('center_axis',(1.,6.76186946307289E-14,-2.76820162751211E-15));
#48529=DIRECTION('ref_axis',(-6.76186946307289E-14,1.,-8.61946552381525E-15));
#48530=DIRECTION('',(6.76186946307289E-14,-1.,8.61946552381525E-15));
#48531=DIRECTION('',(2.76820162751153E-15,8.61946552381544E-15,1.));
#48532=DIRECTION('center_axis',(-2.76820162751153E-15,-8.61946552381544E-15,
-1.));
#48533=DIRECTION('ref_axis',(-1.,-5.93403673771998E-14,2.76820162751204E-15));
#48534=DIRECTION('center_axis',(-1.29309139275491E-14,2.67428077770537E-14,
1.));
#48535=DIRECTION('ref_axis',(-1.,3.5860396038368E-14,-1.29309139275501E-14));
#48536=DIRECTION('',(2.76820162751153E-15,8.61946552381544E-15,1.));
#48537=DIRECTION('center_axis',(-2.76820162751153E-15,-8.61946552381544E-15,
-1.));
#48538=DIRECTION('ref_axis',(0.142617449664357,0.989777885715393,-8.92615021843119E-15));
#48539=DIRECTION('center_axis',(7.02512538336182E-15,1.92786462781398E-14,
1.));
#48540=DIRECTION('ref_axis',(0.142617449664349,0.989777885715395,-2.00834832183795E-14));
#48541=DIRECTION('',(2.76820162751153E-15,8.61946552381544E-15,1.));
#48542=DIRECTION('center_axis',(-2.76820162751153E-15,-8.61946552381544E-15,
-1.));
#48543=DIRECTION('ref_axis',(0.578440307445746,0.815724715036924,-8.63235045867452E-15));
#48544=DIRECTION('center_axis',(-2.04724131764889E-14,6.65582873155238E-15,
1.));
#48545=DIRECTION('ref_axis',(0.578440307445796,0.815724715036889,6.41274497658572E-15));
#48546=DIRECTION('',(2.76820162751153E-15,8.61946552381544E-15,1.));
#48547=DIRECTION('center_axis',(-2.76820162751153E-15,-8.61946552381544E-15,
-1.));
#48548=DIRECTION('ref_axis',(0.7071067811866,-0.707106781186495,4.13746837958792E-15));
#48549=DIRECTION('center_axis',(-6.73174033609845E-16,4.46315286352391E-14,
1.));
#48550=DIRECTION('ref_axis',(0.7071067811866,-0.707106781186495,3.20352624767811E-14));
#48551=DIRECTION('',(2.76820162751153E-15,8.61946552381544E-15,1.));
#48552=DIRECTION('center_axis',(-0.707106781186595,0.7071067811865,-4.13746837958797E-15));
#48553=DIRECTION('ref_axis',(-2.76820162751153E-15,-8.61946552381544E-15,
-1.));
#48554=DIRECTION('',(0.7071067811865,0.707106781186595,-8.05229666459887E-15));
#48555=DIRECTION('center_axis',(3.77043884608029E-15,9.11212513897563E-15,
1.));
#48556=DIRECTION('ref_axis',(-6.75992533669751E-14,1.,-9.79699324159059E-15));
#48557=DIRECTION('center_axis',(1.,6.79666406135347E-14,-3.77043884608091E-15));
#48558=DIRECTION('ref_axis',(6.79666406135348E-14,-1.,8.57236908639177E-15));
#48559=DIRECTION('center_axis',(2.76820162751153E-15,8.61946552381544E-15,
1.));
#48560=DIRECTION('ref_axis',(-6.54074540654431E-14,1.,-8.61946552381526E-15));
#48561=DIRECTION('center_axis',(-2.76820162751153E-15,-8.61946552381544E-15,
-1.));
#48562=DIRECTION('ref_axis',(6.76186946307289E-14,-1.,8.61946552381525E-15));
#48563=DIRECTION('',(6.76186946307289E-14,-1.,8.61946552381525E-15));
#48564=DIRECTION('',(0.707106781186591,-0.707106781186504,4.13746837958802E-15));
#48565=DIRECTION('',(1.,6.76186946307289E-14,-2.76820162751211E-15));
#48566=DIRECTION('',(0.707106781186484,0.707106781186611,-8.05229666459896E-15));
#48567=DIRECTION('',(-6.76186946307289E-14,1.,-8.61946552381525E-15));
#48568=DIRECTION('',(-0.707106781186581,0.707106781186514,-4.13746837958813E-15));
#48569=DIRECTION('',(-1.,-6.76186946307289E-14,2.76820162751211E-15));
#48570=DIRECTION('',(-0.707106781186495,-0.7071067811866,8.0522966645989E-15));
#48571=DIRECTION('center_axis',(-0.706676030840845,0.706676030840825,-0.03489949670248));
#48572=DIRECTION('ref_axis',(6.53747871958143E-16,-0.0493253122022489,-0.99878276595872));
#48573=DIRECTION('',(0.0348958507746445,-0.0144543346614283,-0.999286421306829));
#48574=DIRECTION('',(0.0144543346614127,-0.0348958507746925,-0.999286421306828));
#48575=DIRECTION('center_axis',(0.706676030840779,0.706676030840889,-0.0348994967025111));
#48576=DIRECTION('ref_axis',(4.83744971315161E-16,-0.0493253122022894,-0.998782765958718));
#48577=DIRECTION('',(-0.0144543346614135,-0.0348958507747033,-0.999286421306827));
#48578=DIRECTION('',(-0.0348958507746963,-0.0144543346614329,-0.999286421306827));
#48579=DIRECTION('center_axis',(-6.7674111992527E-14,0.999390827019095,
-0.0348994967025096));
#48580=DIRECTION('ref_axis',(-4.0665690358181E-16,-0.0348994967025096,-0.999390827019096));
#48581=DIRECTION('center_axis',(6.74808943053847E-14,-0.999390827019096,
-0.0348994967024927));
#48582=DIRECTION('ref_axis',(5.12637372416692E-15,-0.0348994967024927,0.999390827019096));
#48583=DIRECTION('',(-0.0144543346614183,0.0348958507746843,-0.999286421306828));
#48584=DIRECTION('',(0.0144543346614081,0.0348958507746774,-0.999286421306828));
#48585=DIRECTION('center_axis',(-0.706676030840789,-0.70667603084088,-0.0348994967024987));
#48586=DIRECTION('ref_axis',(6.04463415039793E-15,-0.0493253122022781,0.998782765958718));
#48587=DIRECTION('',(0.0348958507746425,0.0144543346614176,-0.999286421306829));
#48588=DIRECTION('center_axis',(2.76820162751153E-15,8.61946552381544E-15,
1.));
#48589=DIRECTION('ref_axis',(-6.76186946307289E-14,1.,-8.61946552381525E-15));
#48590=DIRECTION('center_axis',(0.999390827019096,6.72766881403301E-14,
-0.034899496702505));
#48591=DIRECTION('ref_axis',(-6.76186946307289E-14,1.,-8.61946552381525E-15));
#48592=DIRECTION('',(-0.0348958507746983,0.0144543346614128,-0.999286421306827));
#48593=DIRECTION('center_axis',(-0.999390827019097,-6.78783181575814E-14,
-0.034899496702471));
#48594=DIRECTION('ref_axis',(6.76186946307289E-14,-1.,8.61946552381525E-15));
#48595=DIRECTION('center_axis',(0.706676030840878,-0.706676030840792,-0.0348994967024981));
#48596=DIRECTION('ref_axis',(6.10708419553262E-15,-0.0493253122022712,0.998782765958719));
#48597=DIRECTION('center_axis',(-2.76820162751153E-15,-8.61946552381544E-15,
-1.));
#48598=DIRECTION('ref_axis',(6.76186946307289E-14,-1.,8.61946552381525E-15));
#48599=DIRECTION('center_axis',(-1.57236108655672E-14,-6.56288797468043E-14,
-1.));
#48600=DIRECTION('ref_axis',(-0.581108581114844,-0.813826036051129,6.25476162549096E-14));
#48601=DIRECTION('center_axis',(-6.30343034787932E-15,-8.61946552381568E-15,
-1.));
#48602=DIRECTION('ref_axis',(4.99425510288896E-14,-1.,8.61946552381536E-15));
#48603=DIRECTION('center_axis',(-6.30343034787932E-15,-8.61946552381568E-15,
-1.));
#48604=DIRECTION('ref_axis',(4.99425510288896E-14,-1.,8.61946552381536E-15));
#48605=DIRECTION('',(-0.410905818311989,-0.575461908797876,0.707106781186589));
#48606=DIRECTION('center_axis',(-2.76820162751153E-15,-8.61946552381544E-15,
-1.));
#48607=DIRECTION('ref_axis',(-7.14991605308202E-14,1.,-8.61946552381524E-15));
#48608=DIRECTION('center_axis',(2.76820162751153E-15,8.61946552381544E-15,
1.));
#48609=DIRECTION('ref_axis',(6.76186946307289E-14,-1.,8.61946552381525E-15));
#48610=DIRECTION('',(-2.76820162751153E-15,-8.61946552381544E-15,-1.));
#48611=DIRECTION('center_axis',(-9.83865906824712E-15,-8.61946552381592E-15,
-1.));
#48612=DIRECTION('ref_axis',(4.99425510288896E-14,-1.,8.61946552381543E-15));
#48613=DIRECTION('center_axis',(-9.83865906824712E-15,-8.61946552381592E-15,
-1.));
#48614=DIRECTION('ref_axis',(4.99425510288896E-14,-1.,8.61946552381543E-15));
#48615=DIRECTION('center_axis',(-3.19797012705699E-14,2.80182790159477E-14,
1.));
#48616=DIRECTION('ref_axis',(-0.581108581114993,0.813826036051022,-4.13856837783424E-14));
#48617=DIRECTION('',(-0.410905818312099,0.575461908797849,-0.707106781186548));
#48618=DIRECTION('center_axis',(1.,6.76186946307289E-14,-2.76820162751211E-15));
#48619=DIRECTION('ref_axis',(-6.76186946307289E-14,1.,-8.61946552381525E-15));
#48620=DIRECTION('',(6.76186946307289E-14,-1.,8.61946552381525E-15));
#48621=DIRECTION('',(2.76820162751153E-15,8.61946552381544E-15,1.));
#48622=DIRECTION('',(6.76186946307289E-14,-1.,8.61946552381525E-15));
#48623=DIRECTION('',(2.76820162751153E-15,8.61946552381544E-15,1.));
#48624=DIRECTION('center_axis',(0.500000000000024,0.866025403784425,-8.84877692442402E-15));
#48625=DIRECTION('ref_axis',(-2.76820162751153E-15,-8.61946552381544E-15,
-1.));
#48626=DIRECTION('',(0.866025403784471,-0.499999999999943,1.91239982968473E-15));
#48627=DIRECTION('',(2.76820162751153E-15,8.61946552381544E-15,1.));
#48628=DIRECTION('',(0.866025403784471,-0.499999999999943,1.91239982968473E-15));
#48629=DIRECTION('center_axis',(-0.500000000000142,0.866025403784357,1.33116358653071E-14));
#48630=DIRECTION('ref_axis',(-2.61873825433902E-15,1.38590238642998E-14,
-1.));
#48631=DIRECTION('',(0.866025403784404,0.500000000000061,-6.70706569413056E-15));
#48632=DIRECTION('',(2.76820162751153E-15,8.61946552381544E-15,1.));
#48633=DIRECTION('',(0.866025403784404,0.500000000000061,-6.70706569413056E-15));
#48634=DIRECTION('center_axis',(-1.,-6.76186946307289E-14,2.76820162751211E-15));
#48635=DIRECTION('ref_axis',(6.76186946307289E-14,-1.,8.61946552381525E-15));
#48636=DIRECTION('',(6.76186946307289E-14,-1.,8.61946552381525E-15));
#48637=DIRECTION('',(2.76820162751153E-15,8.61946552381544E-15,1.));
#48638=DIRECTION('',(-6.76186946307289E-14,1.,-8.61946552381525E-15));
#48639=DIRECTION('center_axis',(-0.500000000000026,-0.866025403784423,8.84877692442402E-15));
#48640=DIRECTION('ref_axis',(2.76820162751153E-15,8.61946552381544E-15,
1.));
#48641=DIRECTION('',(-0.866025403784473,0.499999999999941,-1.9123998296847E-15));
#48642=DIRECTION('',(2.76820162751153E-15,8.61946552381544E-15,1.));
#48643=DIRECTION('',(-0.866025403784473,0.499999999999941,-1.9123998296847E-15));
#48644=DIRECTION('center_axis',(2.76820162751153E-15,8.61946552381544E-15,
1.));
#48645=DIRECTION('ref_axis',(-6.76186946307289E-14,1.,-8.61946552381525E-15));
#48646=DIRECTION('',(-0.866025403784405,-0.500000000000058,6.70706569413054E-15));
#48647=DIRECTION('center_axis',(0.500000000000166,-0.866025403784343,6.08057529691127E-15));
#48648=DIRECTION('ref_axis',(2.76820162751153E-15,8.61946552381544E-15,
1.));
#48649=DIRECTION('',(-0.866025403784405,-0.500000000000058,6.70706569413054E-15));
#48650=DIRECTION('center_axis',(2.76820162751153E-15,8.61946552381544E-15,
1.));
#48651=DIRECTION('ref_axis',(-6.76186946307289E-14,1.,-8.61946552381525E-15));
#48652=DIRECTION('axis',(0.,0.,1.));
#48653=DIRECTION('refdir',(1.,0.,0.));
#48654=DIRECTION('center_axis',(-7.56024872335536E-14,1.,-6.79969489730031E-15));
#48655=DIRECTION('ref_axis',(-1.,-7.56024872335536E-14,-2.77555756156749E-16));
#48656=DIRECTION('center_axis',(-7.56239704097264E-14,1.,-6.79973512277291E-15));
#48657=DIRECTION('ref_axis',(-1.,-7.56239704097264E-14,-2.77555756156749E-16));
#48658=DIRECTION('',(-7.56024872335536E-14,1.,-6.79969489730031E-15));
#48659=DIRECTION('center_axis',(6.72435353857335E-14,-1.,5.37013150103301E-15));
#48660=DIRECTION('ref_axis',(-1.,-6.72435353857335E-14,-2.77555756156794E-16));
#48661=DIRECTION('center_axis',(-2.7755575615629E-16,-6.07241588737381E-15,
1.));
#48662=DIRECTION('ref_axis',(-1.,-1.66533453693771E-16,-2.77555756156291E-16));
#48663=DIRECTION('',(-2.7755575615629E-16,-6.07241588737381E-15,1.));
#48664=DIRECTION('center_axis',(-2.7755575615629E-16,-6.07241588737381E-15,
1.));
#48665=DIRECTION('ref_axis',(-1.,-1.66533453693771E-16,-2.77555756156291E-16));
#48666=DIRECTION('',(-2.7755575615629E-16,-6.07241588737381E-15,1.));
#48667=DIRECTION('center_axis',(-2.7755575615629E-16,-6.07241588737381E-15,
1.));
#48668=DIRECTION('ref_axis',(-1.,-1.66533453693771E-16,-2.77555756156291E-16));
#48669=DIRECTION('',(-2.7755575615629E-16,-6.07241588737381E-15,1.));
#48670=DIRECTION('center_axis',(-2.7755575615629E-16,-6.07241588737381E-15,
1.));
#48671=DIRECTION('ref_axis',(-1.,-1.66533453693771E-16,-2.77555756156291E-16));
#48672=DIRECTION('',(-2.7755575615629E-16,-6.07241588737381E-15,1.));
#48673=DIRECTION('center_axis',(-6.72435353857335E-14,1.,-5.37013150103301E-15));
#48674=DIRECTION('ref_axis',(-2.77555756156297E-16,5.37013150103299E-15,
1.));
#48675=DIRECTION('center_axis',(-7.25862069473908E-14,1.,-6.26042944676291E-15));
#48676=DIRECTION('ref_axis',(-0.813826036051072,-6.27105343449563E-14,-0.581108581114923));
#48677=DIRECTION('center_axis',(-7.40629779727442E-14,1.,-6.07998716438531E-15));
#48678=DIRECTION('ref_axis',(-1.,-7.40629779727442E-14,-2.77555756156744E-16));
#48679=DIRECTION('',(-7.40629779727442E-14,1.,-6.07998716438531E-15));
#48680=DIRECTION('center_axis',(6.87609227137152E-14,-1.,-8.76572429925892E-16));
#48681=DIRECTION('ref_axis',(-0.813826036051074,-5.64688129283158E-14,0.581108581114921));
#48682=DIRECTION('center_axis',(7.42659901829614E-14,-1.,6.84057719202601E-15));
#48683=DIRECTION('ref_axis',(-1.,-7.42659901829614E-14,-2.77555756156738E-16));
#48684=DIRECTION('center_axis',(7.5080331238299E-14,-1.,-7.2741312686569E-16));
#48685=DIRECTION('ref_axis',(-0.813826036051074,-6.15250343671038E-14,0.58110858111492));
#48686=DIRECTION('center_axis',(7.5080331238299E-14,-1.,-7.2741312686569E-16));
#48687=DIRECTION('ref_axis',(-0.813826036051074,-6.15250343671038E-14,0.58110858111492));
#48688=DIRECTION('',(-7.42659901829614E-14,1.,-6.84057719202601E-15));
#48689=DIRECTION('center_axis',(-8.11684053303452E-14,1.,-3.37179773151922E-14));
#48690=DIRECTION('ref_axis',(-1.,-8.11684053303452E-14,-9.06219543850778E-16));
#48691=DIRECTION('center_axis',(-8.11684053303452E-14,1.,-3.37179773151922E-14));
#48692=DIRECTION('ref_axis',(-1.,-8.11684053303452E-14,-9.06219543850778E-16));
#48693=DIRECTION('center_axis',(-4.77076649660703E-14,1.,-1.51365987155128E-14));
#48694=DIRECTION('ref_axis',(-0.813826036051047,-4.76217472710665E-14,-0.581108581114958));
#48695=DIRECTION('',(-0.57546190879782,-0.707106781186592,-0.410905818312063));
#48696=DIRECTION('center_axis',(-7.86398561629848E-14,1.,1.45566060036366E-14));
#48697=DIRECTION('ref_axis',(-0.813826036051073,-5.55401937561262E-14,-0.581108581114922));
#48698=DIRECTION('center_axis',(7.56239704097264E-14,-1.,6.79973512277291E-15));
#48699=DIRECTION('ref_axis',(2.77555756156191E-16,-6.79973512277289E-15,
-1.));
#48700=DIRECTION('center_axis',(7.6307102664867E-14,-1.,1.38622525122371E-14));
#48701=DIRECTION('ref_axis',(-0.813826036051067,-5.40452329958475E-14,0.58110858111493));
#48702=DIRECTION('center_axis',(-7.39721188273472E-14,1.,-1.0554808768484E-16));
#48703=DIRECTION('ref_axis',(-0.813826036051073,-6.02617711430328E-14,-0.581108581114922));
#48704=DIRECTION('center_axis',(-7.39721188273472E-14,1.,-1.0554808768484E-16));
#48705=DIRECTION('ref_axis',(-0.813826036051073,-6.02617711430328E-14,-0.581108581114922));
#48706=DIRECTION('',(-0.575461908797935,0.707106781186504,0.410905818312053));
#48707=DIRECTION('center_axis',(6.7216128184098E-14,-1.,-3.09884788437082E-15));
#48708=DIRECTION('ref_axis',(-0.813826036051075,-5.65030022559431E-14,0.581108581114919));
#48709=DIRECTION('center_axis',(-6.6878601422281E-14,1.,-8.42209836172541E-15));
#48710=DIRECTION('ref_axis',(-1.,-6.6878601422281E-14,-9.81357852128142E-17));
#48711=DIRECTION('',(6.6878601422281E-14,-1.,8.42209836172541E-15));
#48712=DIRECTION('center_axis',(7.17283375552464E-14,-1.,6.61584725119951E-15));
#48713=DIRECTION('ref_axis',(-1.,-7.17283375552463E-14,5.75531685801174E-15));
#48714=DIRECTION('center_axis',(7.17283375552464E-14,-1.,6.61584725119951E-15));
#48715=DIRECTION('ref_axis',(-1.,-7.17283375552463E-14,5.75531685801174E-15));
#48716=DIRECTION('center_axis',(-8.30355629492075E-14,1.,-2.21448706217753E-15));
#48717=DIRECTION('ref_axis',(-2.77555756156507E-16,2.21448706217751E-15,
1.));
#48718=DIRECTION('center_axis',(-5.82747545344175E-14,1.,-7.72560328633601E-15));
#48719=DIRECTION('ref_axis',(0.813826036051082,5.19149268485742E-14,0.581108581114909));
#48720=DIRECTION('',(0.575461908797932,-0.707106781186507,0.410905818312053));
#48721=DIRECTION('',(0.,0.,1.));
#48722=DIRECTION('',(1.,0.,0.));
#48723=DIRECTION('',(0.,0.,1.));
#48724=DIRECTION('',(1.,0.,0.));
#48725=DIRECTION('',(0.,0.,1.));
#48726=DIRECTION('',(1.,0.,0.));
#48727=DIRECTION('',(0.499999999999949,1.5731954382779E-16,0.866025403784468));
#48728=DIRECTION('',(0.866025403784468,1.50017985838519E-15,-0.499999999999949));
#48729=DIRECTION('',(0.866025403784435,1.04365219448719E-15,0.500000000000006));
#48730=DIRECTION('',(0.500000000000006,2.72071395407886E-15,-0.866025403784435));
#48731=DIRECTION('',(1.,2.48718524494355E-15,9.27036225562007E-15));
#48732=DIRECTION('',(9.27036225562006E-15,3.3852640147228E-15,-1.));
#48733=DIRECTION('',(-0.500000000000005,4.40087876549237E-16,0.866025403784436));
#48734=DIRECTION('',(0.866025403784436,-1.30647364612355E-15,0.500000000000005));
#48735=DIRECTION('',(-0.996957691137886,-2.61024771841798E-15,-0.0779446090567848));
#48736=DIRECTION('',(0.0779446090567848,-1.68273418511062E-15,-0.996957691137886));
#48737=DIRECTION('',(-0.824418382495331,-3.25922747070343E-15,-0.565980857100117));
#48738=DIRECTION('',(0.565980857100117,-1.65234655129868E-15,-0.824418382495331));
#48739=DIRECTION('',(-0.430976834037727,-3.8060666058185E-15,-0.902362991552079));
#48740=DIRECTION('',(0.902362991552079,-1.30154021231385E-15,-0.430976834037727));
#48741=DIRECTION('',(0.0779446090567757,-4.1699194300542E-15,-0.996957691137887));
#48742=DIRECTION('',(0.996957691137887,-7.75016296304832E-16,0.0779446090567757));
#48743=DIRECTION('',(-0.90236299155208,-1.85926161831425E-15,0.430976834037726));
#48744=DIRECTION('',(-0.430976834037726,-1.45594076520776E-15,-0.90236299155208));
#48745=DIRECTION('',(0.,0.,1.));
#48746=DIRECTION('',(1.,0.,0.));
#48747=DIRECTION('',(-2.28053578501289E-31,0.,1.));
#48748=DIRECTION('',(1.,0.,-2.28053578501289E-31));
#48749=DIRECTION('',(-1.,-6.19683138282077E-16,1.10325655394828E-14));
#48750=DIRECTION('',(-1.10325655394828E-14,1.67330091313544E-15,-1.));
#48751=DIRECTION('',(-1.,2.93441552625757E-17,1.10325655394828E-14));
#48752=DIRECTION('',(-1.10325655394828E-14,6.19683138282068E-16,-1.));
#48753=DIRECTION('',(0.,0.,1.));
#48754=DIRECTION('',(1.,0.,0.));
#48755=DIRECTION('',(0.,-5.55111512312579E-17,1.));
#48756=DIRECTION('',(1.,-2.95822839457879E-31,0.));
#48757=DIRECTION('',(0.,-5.55111512312579E-17,1.));
#48758=DIRECTION('',(1.,-2.95822839457879E-31,0.));
#48759=DIRECTION('',(0.,-5.55111512312579E-17,1.));
#48760=DIRECTION('',(1.,-2.95822839457879E-31,0.));
#48761=DIRECTION('',(0.,-5.55111512312579E-17,1.));
#48762=DIRECTION('',(1.,-2.95822839457879E-31,0.));
#48763=DIRECTION('',(0.,-5.55111512312579E-17,1.));
#48764=DIRECTION('',(1.,-2.95822839457879E-31,0.));
#48765=DIRECTION('',(0.,-5.55111512312579E-17,1.));
#48766=DIRECTION('',(1.,-2.95822839457879E-31,0.));
#48767=DIRECTION('',(0.,-5.55111512312579E-17,1.));
#48768=DIRECTION('',(1.,-2.95822839457879E-31,0.));
#48769=DIRECTION('',(-1.09215432370203E-14,9.03884366155634E-30,-1.));
#48770=DIRECTION('',(1.,-1.65021938141356E-15,-1.09215432370203E-14));
#48771=DIRECTION('',(-1.09215432370203E-14,-5.53032878375509E-16,-1.));
#48772=DIRECTION('',(1.,-1.65021938141356E-15,-1.09215432370203E-14));
#48773=DIRECTION('',(-1.09215432370203E-14,-5.53032878375509E-16,-1.));
#48774=DIRECTION('',(1.,-1.65021938141356E-15,-1.09215432370203E-14));
#48775=DIRECTION('',(-1.09215432370203E-14,-5.53032878375509E-16,-1.));
#48776=DIRECTION('',(1.,-1.65021938141356E-15,-1.09215432370203E-14));
#48777=DIRECTION('',(-1.09215432370203E-14,-5.53032878375509E-16,-1.));
#48778=DIRECTION('',(1.,-1.65021938141356E-15,-1.09215432370203E-14));
#48779=DIRECTION('',(-1.09215432370203E-14,-5.53032878375509E-16,-1.));
#48780=DIRECTION('',(1.,-1.65021938141356E-15,-1.09215432370203E-14));
#48781=DIRECTION('',(-1.09215432370203E-14,-5.53032878375509E-16,-1.));
#48782=DIRECTION('',(1.,-1.65021938141356E-15,-1.09215432370203E-14));
#48783=DIRECTION('',(-1.09215432370203E-14,-5.53032878375509E-16,-1.));
#48784=DIRECTION('',(1.,-1.65021938141356E-15,-1.09215432370203E-14));
#48785=DIRECTION('',(0.,0.,1.));
#48786=DIRECTION('',(1.,0.,0.));
#48787=DIRECTION('',(0.,0.,1.));
#48788=DIRECTION('',(1.,-3.39516177580892E-30,0.));
#48789=DIRECTION('',(0.,0.,1.));
#48790=DIRECTION('',(1.,-3.39516177580892E-30,0.));
#48791=DIRECTION('',(1.38942507272227E-15,-5.91645678915759E-31,1.));
#48792=DIRECTION('',(1.,1.5352188818224E-30,-1.38942507272227E-15));
#48793=DIRECTION('',(1.38942507272227E-15,-5.91645678915759E-31,1.));
#48794=DIRECTION('',(1.,-1.8174399653669E-30,-1.38942507272227E-15));
#48795=DIRECTION('',(1.38942507272227E-15,-5.91645678915759E-31,1.));
#48796=DIRECTION('',(1.,-1.8174399653669E-30,-1.38942507272227E-15));
#48797=DIRECTION('',(7.52318358734877E-15,-2.24055836443304E-15,1.));
#48798=DIRECTION('',(-1.,-8.42415004659287E-30,7.52318358734877E-15));
#48799=DIRECTION('',(7.52318358734877E-15,-2.24055836443304E-15,1.));
#48800=DIRECTION('',(-1.,-4.95679401805003E-17,7.52318358734877E-15));
#48801=DIRECTION('',(7.52318358734877E-15,-2.24055836443304E-15,1.));
#48802=DIRECTION('',(-1.,-4.95679401805003E-17,7.52318358734877E-15));
#48803=DIRECTION('',(8.91260866007103E-15,-2.24055836443304E-15,1.));
#48804=DIRECTION('',(-1.,-1.00018718570349E-29,8.91260866007103E-15));
#48805=DIRECTION('',(8.91260866007103E-15,-2.24055836443304E-15,1.));
#48806=DIRECTION('',(-1.,-4.95679401805019E-17,8.91260866007103E-15));
#48807=DIRECTION('',(8.91260866007103E-15,-2.24055836443304E-15,1.));
#48808=DIRECTION('',(-1.,-4.95679401805019E-17,8.91260866007103E-15));
#48809=DIRECTION('',(0.,0.,1.));
#48810=DIRECTION('',(1.,0.,0.));
#48811=DIRECTION('',(0.,0.,1.));
#48812=DIRECTION('',(1.,0.,0.));
#48813=DIRECTION('',(3.34404360992195E-15,0.,1.));
#48814=DIRECTION('',(1.,2.59872095719319E-30,-3.34404360992195E-15));
#48815=DIRECTION('',(3.34404360992195E-15,0.,1.));
#48816=DIRECTION('',(1.,2.59872095719319E-30,-3.34404360992195E-15));
#48817=DIRECTION('',(0.,0.,1.));
#48818=DIRECTION('',(1.,0.,0.));
#48819=DIRECTION('',(0.,0.,1.));
#48820=DIRECTION('',(1.,0.,0.));
#48821=DIRECTION('',(0.,0.,1.));
#48822=DIRECTION('',(1.,0.,0.));
#48823=DIRECTION('',(0.,0.,1.));
#48824=DIRECTION('',(1.,0.,0.));
#48825=DIRECTION('',(0.,0.,1.));
#48826=DIRECTION('',(1.,0.,0.));
#48827=DIRECTION('',(0.,0.,1.));
#48828=DIRECTION('',(1.,0.,0.));
#48829=DIRECTION('',(0.,0.,1.));
#48830=DIRECTION('',(1.,0.,0.));
#48831=DIRECTION('',(0.,0.,1.));
#48832=DIRECTION('',(1.,0.,0.));
#48833=DIRECTION('',(0.,0.,1.));
#48834=DIRECTION('',(1.,0.,0.));
#48835=DIRECTION('',(0.,0.,1.));
#48836=DIRECTION('',(1.,0.,0.));
#48837=CARTESIAN_POINT('',(0.,0.,0.));
#48838=CARTESIAN_POINT('',(0.,0.,0.));
#48839=CARTESIAN_POINT('Origin',(382.3447776627,-195.47200726879,429.516345148026));
#48840=CARTESIAN_POINT('',(382.968334535155,-195.47200726879,421.540683618923));
#48841=CARTESIAN_POINT('',(382.584752280159,-195.47200726879,426.446927731621));
#48842=CARTESIAN_POINT('',(382.937109532866,-195.47200726879,421.940069882636));
#48843=CARTESIAN_POINT('',(382.968334535155,-210.47200726879,421.540683618923));
#48844=CARTESIAN_POINT('',(382.968334535155,-195.47200726879,421.540683618923));
#48845=CARTESIAN_POINT('',(382.584752280159,-210.47200726879,426.446927731621));
#48846=CARTESIAN_POINT('',(382.937109532866,-210.47200726879,421.940069882636));
#48847=CARTESIAN_POINT('',(382.584752280159,-210.47200726879,426.446927731621));
#48848=CARTESIAN_POINT('Origin',(371.0048422415,-195.47200726879,420.605348310242));
#48849=CARTESIAN_POINT('',(370.621259986505,-195.47200726879,425.51159242294));
#48850=CARTESIAN_POINT('',(371.0048422415,-195.47200726879,420.605348310242));
#48851=CARTESIAN_POINT('',(371.285395675438,-195.47200726879,417.016903809402));
#48852=CARTESIAN_POINT('',(370.621259986505,-210.47200726879,425.51159242294));
#48853=CARTESIAN_POINT('',(370.621259986505,-210.47200726879,425.51159242294));
#48854=CARTESIAN_POINT('',(371.0048422415,-210.47200726879,420.605348310242));
#48855=CARTESIAN_POINT('',(371.285395675438,-210.47200726879,417.016903809402));
#48856=CARTESIAN_POINT('',(371.0048422415,-195.47200726879,420.605348310242));
#48857=CARTESIAN_POINT('Origin',(382.968334535155,-195.47200726879,421.540683618923));
#48858=CARTESIAN_POINT('',(353.029152922466,-195.47200726879,419.199964622495));
#48859=CARTESIAN_POINT('',(353.029152922466,-210.47200726879,419.199964622495));
#48860=CARTESIAN_POINT('Origin',(323.651078177653,-210.47200726879,409.682356624389));
#48861=CARTESIAN_POINT('',(420.687969084835,-210.47200726879,385.433330852756));
#48862=CARTESIAN_POINT('',(433.14196495934,-210.47200726879,430.251161579503));
#48863=CARTESIAN_POINT('',(420.081814582884,-210.47200726879,383.251980374045));
#48864=CARTESIAN_POINT('',(431.749931923224,-210.47200726879,448.056088160926));
#48865=CARTESIAN_POINT('',(433.608541542394,-210.47200726879,424.283370880314));
#48866=CARTESIAN_POINT('',(438.073398571173,-210.47200726879,453.263273266005));
#48867=CARTESIAN_POINT('Origin',(436.734720378913,-210.47200726879,448.44581120621));
#48868=CARTESIAN_POINT('',(449.951557303507,-210.47200726879,449.962565992797));
#48869=CARTESIAN_POINT('',(390.584364046299,-210.47200726879,466.459544269457));
#48870=CARTESIAN_POINT('',(403.916141292317,-210.47200726879,514.24988954184));
#48871=CARTESIAN_POINT('Origin',(375.115917770964,-210.47200726879,445.000000551892));
#48872=CARTESIAN_POINT('',(358.875763403191,-210.47200726879,502.626450984414));
#48873=CARTESIAN_POINT('',(354.564704687327,-210.47200726879,501.513908673498));
#48874=CARTESIAN_POINT('',(344.15226118922,-210.47200726879,492.518451721519));
#48875=CARTESIAN_POINT('',(325.221168140732,-210.47200726879,479.521851333988));
#48876=CARTESIAN_POINT('',(336.480973282039,-210.47200726879,495.391141926086));
#48877=CARTESIAN_POINT('Origin',(341.322356903719,-210.47200726879,496.640543633995));
#48878=CARTESIAN_POINT('',(333.400390264926,-210.47200726879,507.328282775076));
#48879=CARTESIAN_POINT('',(346.449185288851,-210.47200726879,456.764703334135));
#48880=CARTESIAN_POINT('',(300.743642935741,-210.47200726879,435.316781261079));
#48881=CARTESIAN_POINT('Origin',(375.115917770964,-210.47200726879,445.000000551892));
#48882=CARTESIAN_POINT('',(333.330024950362,-210.47200726879,402.122389091758));
#48883=CARTESIAN_POINT('',(312.102604347699,-210.47200726879,423.745879662505));
#48884=CARTESIAN_POINT('',(349.445560200449,-210.47200726879,394.42546177323));
#48885=CARTESIAN_POINT('',(327.919413934783,-210.47200726879,404.706546495746));
#48886=CARTESIAN_POINT('',(350.793381459681,-210.47200726879,386.345586463583));
#48887=CARTESIAN_POINT('Origin',(347.290676030261,-210.47200726879,389.91364681547));
#48888=CARTESIAN_POINT('',(341.995805744459,-210.47200726879,377.709152887802));
#48889=CARTESIAN_POINT('',(349.71557428276,-210.47200726879,385.287521106456));
#48890=CARTESIAN_POINT('Origin',(375.115917770964,-210.47200726879,445.000000551892));
#48891=CARTESIAN_POINT('Origin',(375.115917770964,-210.47200726879,445.000000551892));
#48892=CARTESIAN_POINT('Origin',(375.115917770964,-210.47200726879,445.000000551892));
#48893=CARTESIAN_POINT('Origin',(375.115917770964,-195.47200726879,445.000000551892));
#48894=CARTESIAN_POINT('Origin',(438.073398571173,-210.47200726879,453.263273266005));
#48895=CARTESIAN_POINT('',(449.951557303508,-195.47200726879,449.962565992797));
#48896=CARTESIAN_POINT('',(449.951557303507,-210.47200726879,449.962565992797));
#48897=CARTESIAN_POINT('',(438.073398571173,-195.47200726879,453.263273266005));
#48898=CARTESIAN_POINT('',(438.073398571173,-210.47200726879,453.263273266005));
#48899=CARTESIAN_POINT('',(390.584364046299,-195.47200726879,466.459544269457));
#48900=CARTESIAN_POINT('Origin',(436.734720378913,-210.47200726879,448.44581120621));
#48901=CARTESIAN_POINT('',(431.749931923224,-195.47200726879,448.056088160926));
#48902=CARTESIAN_POINT('',(431.749931923224,-210.47200726879,448.056088160926));
#48903=CARTESIAN_POINT('Origin',(436.734720378913,-195.47200726879,448.44581120621));
#48904=CARTESIAN_POINT('Origin',(433.14196495934,-210.47200726879,430.251161579503));
#48905=CARTESIAN_POINT('',(433.14196495934,-195.47200726879,430.251161579503));
#48906=CARTESIAN_POINT('',(433.14196495934,-210.47200726879,430.251161579503));
#48907=CARTESIAN_POINT('',(433.608541542394,-195.47200726879,424.283370880314));
#48908=CARTESIAN_POINT('Origin',(420.176185455833,-210.47200726879,383.591590074578));
#48909=CARTESIAN_POINT('',(420.687969084835,-195.47200726879,385.433330852756));
#48910=CARTESIAN_POINT('',(420.687969084835,-210.47200726879,385.433330852756));
#48911=CARTESIAN_POINT('',(420.081814582884,-195.47200726879,383.251980374046));
#48912=CARTESIAN_POINT('Origin',(336.480973282039,-210.47200726879,495.391141926086));
#48913=CARTESIAN_POINT('',(333.400390264926,-195.47200726879,507.328282775076));
#48914=CARTESIAN_POINT('',(333.400390264926,-210.47200726879,507.328282775076));
#48915=CARTESIAN_POINT('',(336.480973282039,-195.47200726879,495.391141926086));
#48916=CARTESIAN_POINT('',(336.480973282039,-210.47200726879,495.391141926086));
#48917=CARTESIAN_POINT('',(346.449185288851,-195.47200726879,456.764703334135));
#48918=CARTESIAN_POINT('Origin',(341.322356903719,-210.47200726879,496.640543633995));
#48919=CARTESIAN_POINT('',(344.15226118922,-195.47200726879,492.518451721519));
#48920=CARTESIAN_POINT('',(344.15226118922,-210.47200726879,492.518451721519));
#48921=CARTESIAN_POINT('Origin',(341.322356903719,-195.47200726879,496.640543633995));
#48922=CARTESIAN_POINT('Origin',(358.875763403191,-210.47200726879,502.626450984414));
#48923=CARTESIAN_POINT('',(358.875763403191,-195.47200726879,502.626450984414));
#48924=CARTESIAN_POINT('',(358.875763403191,-210.47200726879,502.626450984414));
#48925=CARTESIAN_POINT('',(325.221168140732,-195.47200726879,479.521851333988));
#48926=CARTESIAN_POINT('Origin',(405.767027407906,-210.47200726879,514.727542306972));
#48927=CARTESIAN_POINT('',(403.916141292317,-195.47200726879,514.24988954184));
#48928=CARTESIAN_POINT('',(403.916141292317,-210.47200726879,514.24988954184));
#48929=CARTESIAN_POINT('',(354.564704687327,-195.47200726879,501.513908673498));
#48930=CARTESIAN_POINT('Origin',(375.115917770964,-210.47200726879,445.000000551892));
#48931=CARTESIAN_POINT('',(300.743642935741,-195.47200726879,435.316781261079));
#48932=CARTESIAN_POINT('Origin',(375.115917770964,-195.47200726879,445.000000551892));
#48933=CARTESIAN_POINT('',(300.743642935741,-210.47200726879,435.316781261079));
#48934=CARTESIAN_POINT('Origin',(375.115917770964,-210.47200726879,445.000000551892));
#48935=CARTESIAN_POINT('Origin',(375.115917770964,-195.47200726879,445.000000551892));
#48936=CARTESIAN_POINT('Origin',(347.290676030261,-210.47200726879,389.91364681547));
#48937=CARTESIAN_POINT('',(349.445560200449,-195.47200726879,394.42546177323));
#48938=CARTESIAN_POINT('',(349.445560200449,-210.47200726879,394.42546177323));
#48939=CARTESIAN_POINT('',(350.793381459681,-195.47200726879,386.345586463583));
#48940=CARTESIAN_POINT('Origin',(347.290676030261,-195.47200726879,389.91364681547));
#48941=CARTESIAN_POINT('',(350.793381459681,-210.47200726879,386.345586463583));
#48942=CARTESIAN_POINT('Origin',(333.330024950362,-210.47200726879,402.122389091758));
#48943=CARTESIAN_POINT('',(333.330024950362,-195.47200726879,402.122389091758));
#48944=CARTESIAN_POINT('',(333.330024950362,-210.47200726879,402.122389091758));
#48945=CARTESIAN_POINT('',(327.919413934783,-195.47200726879,404.706546495746));
#48946=CARTESIAN_POINT('Origin',(299.404540449154,-210.47200726879,436.680869274125));
#48947=CARTESIAN_POINT('',(312.102604347699,-195.47200726879,423.745879662505));
#48948=CARTESIAN_POINT('Origin',(350.793381459681,-210.47200726879,386.345586463583));
#48949=CARTESIAN_POINT('',(341.995805744459,-195.47200726879,377.709152887802));
#48950=CARTESIAN_POINT('',(341.995805744459,-210.47200726879,377.709152887802));
#48951=CARTESIAN_POINT('',(349.71557428276,-195.47200726879,385.287521106456));
#48952=CARTESIAN_POINT('Origin',(375.115917770964,-210.47200726879,445.000000551892));
#48953=CARTESIAN_POINT('Origin',(375.115917770964,-195.47200726879,445.000000551892));
#48954=CARTESIAN_POINT('Origin',(323.651078177653,-195.47200726879,409.682356624389));
#48955=CARTESIAN_POINT('',(0.,0.,0.));
#48956=CARTESIAN_POINT('Origin',(263.115917770968,-85.47200726879,445.000000551893));
#48957=CARTESIAN_POINT('',(209.115917770968,-85.4720072687899,402.500000551893));
#48958=CARTESIAN_POINT('',(220.615917770968,-85.4720072687899,391.000000551893));
#48959=CARTESIAN_POINT('Origin',(220.615917770968,-85.4720072687899,402.500000551893));
#48960=CARTESIAN_POINT('',(305.615917770968,-85.47200726879,391.000000551893));
#48961=CARTESIAN_POINT('',(220.615917770968,-85.4720072687899,391.000000551893));
#48962=CARTESIAN_POINT('',(317.115917770968,-85.47200726879,402.500000551893));
#48963=CARTESIAN_POINT('Origin',(305.615917770968,-85.47200726879,402.500000551893));
#48964=CARTESIAN_POINT('',(317.115917770968,-85.4720072687901,487.500000551893));
#48965=CARTESIAN_POINT('',(317.115917770968,-85.47200726879,402.500000551893));
#48966=CARTESIAN_POINT('',(305.615917770968,-85.4720072687901,499.000000551893));
#48967=CARTESIAN_POINT('Origin',(305.615917770968,-85.4720072687901,487.500000551893));
#48968=CARTESIAN_POINT('',(220.615917770968,-85.47200726879,499.000000551893));
#48969=CARTESIAN_POINT('',(305.615917770968,-85.4720072687901,499.000000551893));
#48970=CARTESIAN_POINT('',(209.115917770968,-85.47200726879,487.500000551893));
#48971=CARTESIAN_POINT('Origin',(220.615917770968,-85.47200726879,487.500000551893));
#48972=CARTESIAN_POINT('',(209.115917770968,-85.47200726879,487.500000551893));
#48973=CARTESIAN_POINT('',(215.865917770968,-85.4720072687899,403.500000551893));
#48974=CARTESIAN_POINT('Origin',(221.615917770968,-85.4720072687899,403.500000551893));
#48975=CARTESIAN_POINT('',(298.865917770968,-85.47200726879,403.500000551893));
#48976=CARTESIAN_POINT('Origin',(304.615917770968,-85.47200726879,403.500000551893));
#48977=CARTESIAN_POINT('',(298.865917770968,-85.4720072687901,486.500000551893));
#48978=CARTESIAN_POINT('Origin',(304.615917770968,-85.4720072687901,486.500000551893));
#48979=CARTESIAN_POINT('',(215.865917770968,-85.47200726879,486.500000551893));
#48980=CARTESIAN_POINT('Origin',(221.615917770968,-85.47200726879,486.500000551893));
#48981=CARTESIAN_POINT('',(304.615917770968,-85.47200726879,415.000000551893));
#48982=CARTESIAN_POINT('',(293.115917770968,-85.47200726879,403.500000551893));
#48983=CARTESIAN_POINT('Origin',(304.615917770968,-85.47200726879,403.500000551893));
#48984=CARTESIAN_POINT('',(233.115917770968,-85.4720072687899,403.500000551893));
#48985=CARTESIAN_POINT('',(233.115917770968,-85.4720072687899,403.500000551893));
#48986=CARTESIAN_POINT('',(221.615917770968,-85.47200726879,415.000000551893));
#48987=CARTESIAN_POINT('Origin',(221.615917770968,-85.4720072687899,403.500000551893));
#48988=CARTESIAN_POINT('',(221.615917770968,-85.47200726879,475.000000551893));
#48989=CARTESIAN_POINT('',(221.615917770968,-85.47200726879,475.000000551893));
#48990=CARTESIAN_POINT('',(233.115917770968,-85.47200726879,486.500000551893));
#48991=CARTESIAN_POINT('Origin',(221.615917770968,-85.47200726879,486.500000551893));
#48992=CARTESIAN_POINT('',(293.115917770968,-85.4720072687901,486.500000551893));
#48993=CARTESIAN_POINT('',(293.115917770968,-85.4720072687901,486.500000551893));
#48994=CARTESIAN_POINT('',(304.615917770968,-85.4720072687901,475.000000551893));
#48995=CARTESIAN_POINT('Origin',(304.615917770968,-85.4720072687901,486.500000551893));
#48996=CARTESIAN_POINT('',(304.615917770968,-85.47200726879,415.000000551893));
#48997=CARTESIAN_POINT('Origin',(220.615917770968,-69.4720072687899,402.500000551893));
#48998=CARTESIAN_POINT('',(209.115917770967,-72.0120072687899,402.500000536626));
#48999=CARTESIAN_POINT('',(220.615917771658,-72.0120072687899,391.000000551893));
#49000=CARTESIAN_POINT('Origin',(220.615917770968,-72.0120072687899,402.500000551893));
#49001=CARTESIAN_POINT('',(220.615917770968,-85.4720072687899,391.000000551893));
#49002=CARTESIAN_POINT('',(209.115917770968,-85.4720072687899,402.500000551893));
#49003=CARTESIAN_POINT('Origin',(220.615917770968,-72.0120072687899,402.500000551893));
#49004=CARTESIAN_POINT('',(211.655917428536,-69.47200726879,402.500000528338));
#49005=CARTESIAN_POINT('Origin',(211.655917770968,-72.0120072687899,402.500000526873));
#49006=CARTESIAN_POINT('',(220.615917770968,-69.47200726879,393.540000209774));
#49007=CARTESIAN_POINT('Origin',(220.615917770968,-69.47200726879,402.500000551893));
#49008=CARTESIAN_POINT('Origin',(220.615917770968,-72.0120072687899,393.540000551893));
#49009=CARTESIAN_POINT('Origin',(220.367523674428,-72.0120072687899,393.540000551893));
#49010=CARTESIAN_POINT('',(227.022312716318,-69.4720072687899,393.540000551893));
#49011=CARTESIAN_POINT('',(220.615917770968,-69.4720072687899,393.540000551893));
#49012=CARTESIAN_POINT('',(227.022399311985,-72.0120048639452,391.000000934311));
#49013=CARTESIAN_POINT('Origin',(227.022312716318,-72.0120072687899,393.540000551893));
#49014=CARTESIAN_POINT('',(220.615917771658,-72.0120072687899,391.000000551893));
#49015=CARTESIAN_POINT('Origin',(263.115917770968,-69.47200726879,445.000000551893));
#49016=CARTESIAN_POINT('',(290.999730487759,-69.4720073199884,486.249685136186));
#49017=CARTESIAN_POINT('',(304.365591386209,-69.4720072899969,472.883807402065));
#49018=CARTESIAN_POINT('Origin',(263.115917770968,-69.4720072685233,445.000000551893));
#49019=CARTESIAN_POINT('',(299.209522825618,-69.4720072687901,496.460000551893));
#49020=CARTESIAN_POINT('',(290.999736208098,-69.4720072840695,486.249688664203));
#49021=CARTESIAN_POINT('',(305.615917770968,-69.4720072687901,496.460000894012));
#49022=CARTESIAN_POINT('',(305.615917770968,-69.4720072687901,496.460000551893));
#49023=CARTESIAN_POINT('',(314.5759181134,-69.4720072687901,487.500000575449));
#49024=CARTESIAN_POINT('Origin',(305.615917770968,-69.4720072687902,487.500000551893));
#49025=CARTESIAN_POINT('',(314.575917770968,-69.4720072687901,481.093605606543));
#49026=CARTESIAN_POINT('',(314.575917770968,-69.4720072687901,481.093605606543));
#49027=CARTESIAN_POINT('',(314.575917770968,-69.4720072687901,481.093605606543));
#49028=CARTESIAN_POINT('',(298.865917770968,-69.4720072687901,486.500000551893));
#49029=CARTESIAN_POINT('Origin',(304.615917770968,-69.4720072687901,486.500000551893));
#49030=CARTESIAN_POINT('Origin',(263.115917770968,-69.47200726879,445.000000551893));
#49031=CARTESIAN_POINT('',(304.365590681733,-69.4720072757894,417.116194305707));
#49032=CARTESIAN_POINT('',(290.999729934783,-69.4720072776403,403.750316697743));
#49033=CARTESIAN_POINT('Origin',(263.115917770968,-69.4720072684969,445.000000551893));
#49034=CARTESIAN_POINT('',(314.575917770968,-69.47200726879,408.906395497243));
#49035=CARTESIAN_POINT('',(304.365605883278,-69.4720072829853,417.116182114733));
#49036=CARTESIAN_POINT('',(314.575918113087,-69.47200726879,402.500000551893));
#49037=CARTESIAN_POINT('',(314.575917770968,-69.47200726879,402.500000551893));
#49038=CARTESIAN_POINT('',(305.615917794523,-69.47200726879,393.540000209461));
#49039=CARTESIAN_POINT('Origin',(305.615917770968,-69.4720072687901,402.500000551893));
#49040=CARTESIAN_POINT('',(299.209522825618,-69.47200726879,393.540000551893));
#49041=CARTESIAN_POINT('',(299.209522825618,-69.47200726879,393.540000551893));
#49042=CARTESIAN_POINT('',(299.209522825618,-69.47200726879,393.540000551893));
#49043=CARTESIAN_POINT('',(298.865917770968,-69.47200726879,403.500000551893));
#49044=CARTESIAN_POINT('Origin',(304.615917770968,-69.47200726879,403.500000551893));
#49045=CARTESIAN_POINT('Origin',(263.115917770968,-69.47200726879,445.000000551893));
#49046=CARTESIAN_POINT('',(235.232105054176,-69.4720073199883,403.750315967598));
#49047=CARTESIAN_POINT('',(221.866244155727,-69.4720072899968,417.116193701721));
#49048=CARTESIAN_POINT('Origin',(263.115917770968,-69.4720072685233,445.000000551893));
#49049=CARTESIAN_POINT('',(235.232099333838,-69.4720072840694,403.750312439583));
#49050=CARTESIAN_POINT('',(211.655917770968,-69.4720072687899,408.906395497243));
#49051=CARTESIAN_POINT('',(211.655917770968,-69.4720072687899,408.906395497243));
#49052=CARTESIAN_POINT('',(211.655917770968,-69.4720072687899,408.906395497243));
#49053=CARTESIAN_POINT('',(215.865917770968,-69.4720072687899,403.500000551893));
#49054=CARTESIAN_POINT('Origin',(221.615917770968,-69.4720072687899,403.500000551893));
#49055=CARTESIAN_POINT('Origin',(263.115917770968,-69.47200726879,445.000000551893));
#49056=CARTESIAN_POINT('',(221.866244860203,-69.4720072757895,472.883806798079));
#49057=CARTESIAN_POINT('',(235.232105607153,-69.4720072776404,486.249684406043));
#49058=CARTESIAN_POINT('Origin',(263.115917770968,-69.4720072684969,445.000000551893));
#49059=CARTESIAN_POINT('',(211.655917770968,-69.47200726879,481.093605606543));
#49060=CARTESIAN_POINT('',(221.866229658658,-69.4720072829853,472.883818989053));
#49061=CARTESIAN_POINT('',(211.655917428849,-69.4720072687901,487.500000551893));
#49062=CARTESIAN_POINT('',(211.655917770968,-69.47200726879,487.500000551893));
#49063=CARTESIAN_POINT('',(220.615917747413,-69.4720072687901,496.460000894325));
#49064=CARTESIAN_POINT('Origin',(220.615917770968,-69.4720072687901,487.500000551893));
#49065=CARTESIAN_POINT('',(227.022312716318,-69.47200726879,496.460000551893));
#49066=CARTESIAN_POINT('',(227.022312716318,-69.47200726879,496.460000551893));
#49067=CARTESIAN_POINT('',(227.022312716318,-69.47200726879,496.460000551893));
#49068=CARTESIAN_POINT('',(215.865917770968,-69.47200726879,486.500000551893));
#49069=CARTESIAN_POINT('Origin',(221.615917770968,-69.47200726879,486.500000551893));
#49070=CARTESIAN_POINT('Origin',(221.615917770968,-67.8720072687899,403.500000551893));
#49071=CARTESIAN_POINT('',(215.865917770968,-67.8720072687899,403.500000551893));
#49072=CARTESIAN_POINT('Origin',(304.615917770968,-67.87200726879,403.500000551893));
#49073=CARTESIAN_POINT('',(298.865917770968,-67.87200726879,403.500000551893));
#49074=CARTESIAN_POINT('Origin',(304.615917770968,-67.8720072687901,486.500000551893));
#49075=CARTESIAN_POINT('',(298.865917770968,-67.8720072687901,486.500000551893));
#49076=CARTESIAN_POINT('Origin',(221.615917770968,-67.87200726879,486.500000551893));
#49077=CARTESIAN_POINT('',(215.865917770968,-67.87200726879,486.500000551893));
#49078=CARTESIAN_POINT('Origin',(263.115917770968,-66.93200726879,445.000000551893));
#49079=CARTESIAN_POINT('',(302.261283577094,-66.93200726879,471.46134667694));
#49080=CARTESIAN_POINT('Origin',(304.365605883808,-66.9320073823691,472.883818948733));
#49081=CARTESIAN_POINT('',(289.577263857934,-66.932007268792,484.145366370259));
#49082=CARTESIAN_POINT('Origin',(263.115917770968,-66.93200726879,445.000000551893));
#49083=CARTESIAN_POINT('Origin',(290.999736208028,-66.93200726879,486.249688664283));
#49084=CARTESIAN_POINT('Ctrl Pts',(288.998285659208,-70.8410255423381,487.371976483543));
#49085=CARTESIAN_POINT('Ctrl Pts',(289.064861327528,-70.712722248464,487.348817061843));
#49086=CARTESIAN_POINT('Ctrl Pts',(289.246966153228,-70.4229586079247,487.284039301003));
#49087=CARTESIAN_POINT('Ctrl Pts',(289.613432565908,-70.0324228883725,487.143425190533));
#49088=CARTESIAN_POINT('Ctrl Pts',(290.085363845378,-69.7114497472353,486.941854741653));
#49089=CARTESIAN_POINT('Ctrl Pts',(290.593740217718,-69.5126381445131,486.698890965093));
#49090=CARTESIAN_POINT('Ctrl Pts',(290.971346420728,-69.4612407849915,486.497163873883));
#49091=CARTESIAN_POINT('Ctrl Pts',(291.171959587518,-69.464214633553,486.382871735513));
#49092=CARTESIAN_POINT('Ctrl Pts',(291.203406899448,-69.4654396674751,486.364779958613));
#49093=CARTESIAN_POINT('Ctrl Pts',(288.092412841418,-70.7821785594621,485.955461353113));
#49094=CARTESIAN_POINT('Ctrl Pts',(288.166834942358,-70.6531438863331,485.927338245653));
#49095=CARTESIAN_POINT('Ctrl Pts',(288.367773215418,-70.3684786785252,485.850444521383));
#49096=CARTESIAN_POINT('Ctrl Pts',(288.755212370428,-70.0112367740759,485.696202514793));
#49097=CARTESIAN_POINT('Ctrl Pts',(289.226188565798,-69.7468008290303,485.495309940943));
#49098=CARTESIAN_POINT('Ctrl Pts',(289.706503561258,-69.6062166524364,485.271875115773));
#49099=CARTESIAN_POINT('Ctrl Pts',(290.047780774728,-69.5867023581793,485.096173932863));
#49100=CARTESIAN_POINT('Ctrl Pts',(290.226195016768,-69.6011587121203,484.998161076463));
#49101=CARTESIAN_POINT('Ctrl Pts',(290.254102448988,-69.6040471487246,484.982674968233));
#49102=CARTESIAN_POINT('Ctrl Pts',(286.563889095188,-70.1428862842578,485.663027413833));
#49103=CARTESIAN_POINT('Ctrl Pts',(286.670561310298,-69.9482081499977,485.609927354613));
#49104=CARTESIAN_POINT('Ctrl Pts',(286.958062081058,-69.5204913988233,485.465578959453));
#49105=CARTESIAN_POINT('Ctrl Pts',(287.509285705738,-68.9908005466805,485.181938243533));
#49106=CARTESIAN_POINT('Ctrl Pts',(288.174844305588,-68.6071038509314,484.824524259113));
#49107=CARTESIAN_POINT('Ctrl Pts',(288.850431096308,-68.4105256300781,484.441925233693));
#49108=CARTESIAN_POINT('Ctrl Pts',(289.330116142288,-68.389499075236,484.152675406223));
#49109=CARTESIAN_POINT('Ctrl Pts',(289.581590656338,-68.4143084253991,483.994803323553));
#49110=CARTESIAN_POINT('Ctrl Pts',(289.620947839548,-68.4190995018021,483.969940141563));
#49111=CARTESIAN_POINT('Ctrl Pts',(285.486322930458,-69.372176498392,486.700075181433));
#49112=CARTESIAN_POINT('Ctrl Pts',(285.626997021668,-69.0930496471823,486.619528281213));
#49113=CARTESIAN_POINT('Ctrl Pts',(286.007989346758,-68.4746082940248,486.399765496033));
#49114=CARTESIAN_POINT('Ctrl Pts',(286.750769803908,-67.687850874675,485.961842661743));
#49115=CARTESIAN_POINT('Ctrl Pts',(287.669776998228,-67.092862159682,485.400645899203));
#49116=CARTESIAN_POINT('Ctrl Pts',(288.626813241638,-66.7653976675591,484.791983689493));
#49117=CARTESIAN_POINT('Ctrl Pts',(289.322427686498,-66.710525711832,484.329365258813));
#49118=CARTESIAN_POINT('Ctrl Pts',(289.690905404228,-66.7372867844731,484.077539521653));
#49119=CARTESIAN_POINT('Ctrl Pts',(289.748659863038,-66.742883356668,484.037902817103));
#49120=CARTESIAN_POINT('',(285.988731321319,-69.4720430411235,486.344876715169));
#49121=CARTESIAN_POINT('Ctrl Pts',(285.988756574376,-69.4718748783635,486.34485393706));
#49122=CARTESIAN_POINT('Ctrl Pts',(286.118744452923,-69.2047921984534,486.272949747314));
#49123=CARTESIAN_POINT('Ctrl Pts',(286.412224215766,-68.7100477492417,486.109000546669));
#49124=CARTESIAN_POINT('Ctrl Pts',(286.951205734338,-68.071986203272,485.799398096773));
#49125=CARTESIAN_POINT('Ctrl Pts',(287.559472514128,-67.566352173163,485.438326232773));
#49126=CARTESIAN_POINT('Ctrl Pts',(288.213563806918,-67.2011737721991,485.035967098023));
#49127=CARTESIAN_POINT('Ctrl Pts',(288.891014788688,-66.981639700943,484.603378736393));
#49128=CARTESIAN_POINT('Ctrl Pts',(289.347255309368,-66.932003603433,484.300842719953));
#49129=CARTESIAN_POINT('Ctrl Pts',(289.577263878948,-66.9320072687941,484.145366401723));
#49130=CARTESIAN_POINT('',(288.93249809502,-70.7420402776062,487.189112872311));
#49131=CARTESIAN_POINT('Origin',(287.218164767968,-69.4721762071729,488.567491527033));
#49132=CARTESIAN_POINT('Ctrl Pts',(288.93252952171,-70.7420200455039,487.189113576105));
#49133=CARTESIAN_POINT('Ctrl Pts',(288.988623498153,-70.6445951393942,487.169106682144));
#49134=CARTESIAN_POINT('Ctrl Pts',(289.050594887069,-70.5513567221658,487.146538078092));
#49135=CARTESIAN_POINT('Ctrl Pts',(289.141870461995,-70.4311536188864,487.112441714298));
#49136=CARTESIAN_POINT('Ctrl Pts',(289.166664996978,-70.4000028232925,487.103104730079));
#49137=CARTESIAN_POINT('Ctrl Pts',(289.288288528221,-70.2540727483778,487.056904492515));
#49138=CARTESIAN_POINT('Ctrl Pts',(289.393550533437,-70.1478860178951,487.015764059843));
#49139=CARTESIAN_POINT('Ctrl Pts',(289.510668415097,-70.0479200253442,486.968035327824));
#49140=CARTESIAN_POINT('Ctrl Pts',(289.516201545576,-70.0432370796359,486.96577616909));
#49141=CARTESIAN_POINT('Ctrl Pts',(289.628422450322,-69.9490612742506,486.919869119029));
#49142=CARTESIAN_POINT('Ctrl Pts',(289.740699614602,-69.8694544987993,486.872336831436));
#49143=CARTESIAN_POINT('Ctrl Pts',(289.900685400632,-69.7740400952016,486.801798814279));
#49144=CARTESIAN_POINT('Ctrl Pts',(289.945476928754,-69.7491804686929,486.781766067426));
#49145=CARTESIAN_POINT('Ctrl Pts',(290.069653334246,-69.6852131557637,486.725375784309));
#49146=CARTESIAN_POINT('Ctrl Pts',(290.14983936454,-69.6493657107357,486.688021219364));
#49147=CARTESIAN_POINT('Ctrl Pts',(290.316444820684,-69.5855318937613,486.608314250907));
#49148=CARTESIAN_POINT('Ctrl Pts',(290.402937085815,-69.5581670824828,486.565796223865));
#49149=CARTESIAN_POINT('Ctrl Pts',(290.531326493797,-69.525878339649,486.500878319984));
#49150=CARTESIAN_POINT('Ctrl Pts',(290.572982658775,-69.5166925224002,486.479536360681));
#49151=CARTESIAN_POINT('Ctrl Pts',(290.743416506245,-69.4843334129536,486.391078676298));
#49152=CARTESIAN_POINT('Ctrl Pts',(290.872510995065,-69.4720048208224,486.321377974098));
#49153=CARTESIAN_POINT('Ctrl Pts',(290.999733582907,-69.4720073298542,486.249690143456));
#49154=CARTESIAN_POINT('Origin',(263.115917770968,-85.47200726879,445.000000551893));
#49155=CARTESIAN_POINT('',(263.115917770968,-56.01200726879,492.250000551893));
#49156=CARTESIAN_POINT('',(262.857585971945,-56.01200726879,492.24929435277));
#49157=CARTESIAN_POINT('Origin',(263.115917770968,-56.01200726879,445.000000551893));
#49158=CARTESIAN_POINT('',(263.115917770968,-69.4720072687901,492.250000551893));
#49159=CARTESIAN_POINT('',(263.115917770968,-85.4720072687901,492.250000551893));
#49160=CARTESIAN_POINT('Origin',(263.115917770968,-69.47200726879,445.000000551893));
#49161=CARTESIAN_POINT('',(304.46086780848,-69.4721941921344,467.872700496303));
#49162=CARTESIAN_POINT('Ctrl Pts',(302.261283619528,-66.93200726879,471.461346659823));
#49163=CARTESIAN_POINT('Ctrl Pts',(302.418142881798,-66.932003845303,471.229292331673));
#49164=CARTESIAN_POINT('Ctrl Pts',(302.722783928448,-66.982389652618,470.769804097933));
#49165=CARTESIAN_POINT('Ctrl Pts',(303.158021100128,-67.205344908648,470.087868144283));
#49166=CARTESIAN_POINT('Ctrl Pts',(303.558526243438,-67.571638226744,469.436410965183));
#49167=CARTESIAN_POINT('Ctrl Pts',(303.916770751998,-68.074931862037,468.832754965133));
#49168=CARTESIAN_POINT('Ctrl Pts',(304.224868997438,-68.7101394690151,468.296382954193));
#49169=CARTESIAN_POINT('Ctrl Pts',(304.388818617838,-69.2046237434901,468.002914444963));
#49170=CARTESIAN_POINT('Ctrl Pts',(304.460794941428,-69.4719904999791,467.872796581653));
#49171=CARTESIAN_POINT('',(304.460780736566,-69.4720434315167,422.127162382352));
#49172=CARTESIAN_POINT('Origin',(263.115917770968,-69.47200726879,445.000000551893));
#49173=CARTESIAN_POINT('',(302.261283588757,-66.93200726879,418.53865446472));
#49174=CARTESIAN_POINT('Ctrl Pts',(304.460757971866,-69.4718531713743,422.127137633859));
#49175=CARTESIAN_POINT('Ctrl Pts',(304.388790543676,-69.2045390954083,421.997036357919));
#49176=CARTESIAN_POINT('Ctrl Pts',(304.224851420204,-68.7101031547398,421.703587571966));
#49177=CARTESIAN_POINT('Ctrl Pts',(303.916770755058,-68.074931865877,421.167246137583));
#49178=CARTESIAN_POINT('Ctrl Pts',(303.558526234868,-67.571638234798,420.563590126083));
#49179=CARTESIAN_POINT('Ctrl Pts',(303.158021102038,-67.20534489923,419.912132962153));
#49180=CARTESIAN_POINT('Ctrl Pts',(302.722783926568,-66.982389656305,419.230197003253));
#49181=CARTESIAN_POINT('Ctrl Pts',(302.418142881528,-66.932003845745,418.770708771203));
#49182=CARTESIAN_POINT('Ctrl Pts',(302.261283619518,-66.93200726879,418.538654443953));
#49183=CARTESIAN_POINT('',(289.577263929339,-66.9320072687885,405.854634796628));
#49184=CARTESIAN_POINT('Origin',(263.115917770968,-66.93200726879,445.000000551893));
#49185=CARTESIAN_POINT('',(285.988607027166,-69.4721792344465,403.655044784447));
#49186=CARTESIAN_POINT('Ctrl Pts',(289.577263854638,-66.932007268787,405.854634739443));
#49187=CARTESIAN_POINT('Ctrl Pts',(289.347343615378,-66.932005368643,405.699217182813));
#49188=CARTESIAN_POINT('Ctrl Pts',(288.891074071928,-66.981556806277,405.396653518833));
#49189=CARTESIAN_POINT('Ctrl Pts',(288.212152496378,-67.201691318908,404.963139413083));
#49190=CARTESIAN_POINT('Ctrl Pts',(287.557492638358,-67.567693344638,404.560478072123));
#49191=CARTESIAN_POINT('Ctrl Pts',(286.949480792468,-68.073737286196,404.199599095673));
#49192=CARTESIAN_POINT('Ctrl Pts',(286.411264535488,-68.7115153777147,403.890461337593));
#49193=CARTESIAN_POINT('Ctrl Pts',(286.118404220698,-69.2054638755325,403.726863292833));
#49194=CARTESIAN_POINT('Ctrl Pts',(285.988695062078,-69.47199135406,403.655113065203));
#49195=CARTESIAN_POINT('',(240.243104220617,-69.4720430411234,403.655124388617));
#49196=CARTESIAN_POINT('Origin',(263.115917770968,-69.47200726879,445.000000551893));
#49197=CARTESIAN_POINT('',(236.654571684002,-66.9320072687919,405.854634733527));
#49198=CARTESIAN_POINT('Ctrl Pts',(240.243078967561,-69.4718748783634,403.655147166726));
#49199=CARTESIAN_POINT('Ctrl Pts',(240.113091089014,-69.2047921984533,403.727051356473));
#49200=CARTESIAN_POINT('Ctrl Pts',(239.81961132617,-68.7100477492417,403.891000557117));
#49201=CARTESIAN_POINT('Ctrl Pts',(239.280629807598,-68.0719862032719,404.200603007013));
#49202=CARTESIAN_POINT('Ctrl Pts',(238.672363027808,-67.5663521731629,404.561674871013));
#49203=CARTESIAN_POINT('Ctrl Pts',(238.018271735018,-67.2011737721989,404.964034005763));
#49204=CARTESIAN_POINT('Ctrl Pts',(237.340820753248,-66.9816397009429,405.396622367393));
#49205=CARTESIAN_POINT('Ctrl Pts',(236.884580232568,-66.9320036034329,405.699158383833));
#49206=CARTESIAN_POINT('Ctrl Pts',(236.654571662988,-66.9320072687939,405.854634702063));
#49207=CARTESIAN_POINT('',(223.970551964843,-66.93200726879,418.538654426845));
#49208=CARTESIAN_POINT('Origin',(263.115917770968,-66.93200726879,445.000000551893));
#49209=CARTESIAN_POINT('',(221.770967733456,-69.4721941921343,422.127300607483));
#49210=CARTESIAN_POINT('Ctrl Pts',(223.970551922408,-66.9320072687899,418.538654443963));
#49211=CARTESIAN_POINT('Ctrl Pts',(223.813692660138,-66.9320038453029,418.770708772113));
#49212=CARTESIAN_POINT('Ctrl Pts',(223.509051613488,-66.9823896526179,419.230197005853));
#49213=CARTESIAN_POINT('Ctrl Pts',(223.073814441808,-67.2053449086479,419.912132959503));
#49214=CARTESIAN_POINT('Ctrl Pts',(222.673309298498,-67.5716382267429,420.563590138603));
#49215=CARTESIAN_POINT('Ctrl Pts',(222.315064789938,-68.0749318620369,421.167246138653));
#49216=CARTESIAN_POINT('Ctrl Pts',(222.006966544498,-68.7101394690148,421.703618149593));
#49217=CARTESIAN_POINT('Ctrl Pts',(221.843016924098,-69.20462374349,421.997086658823));
#49218=CARTESIAN_POINT('Ctrl Pts',(221.771040600508,-69.471990499979,422.127204522133));
#49219=CARTESIAN_POINT('',(221.771098592854,-69.4723526686334,467.87293717337));
#49220=CARTESIAN_POINT('Origin',(263.115917770968,-69.47200726879,445.000000551893));
#49221=CARTESIAN_POINT('',(223.970551953179,-66.93200726879,471.461346639066));
#49222=CARTESIAN_POINT('Ctrl Pts',(221.771077570127,-69.4718531714348,467.872863470021));
#49223=CARTESIAN_POINT('Ctrl Pts',(221.84304499834,-69.2045390954037,468.002964746004));
#49224=CARTESIAN_POINT('Ctrl Pts',(222.006984121657,-68.7101031548514,468.296413531676));
#49225=CARTESIAN_POINT('Ctrl Pts',(222.315064786898,-68.074931865861,468.832754966233));
#49226=CARTESIAN_POINT('Ctrl Pts',(222.673309307068,-67.571638234802,469.436410977693));
#49227=CARTESIAN_POINT('Ctrl Pts',(223.073814439898,-67.205344899229,470.087868141633));
#49228=CARTESIAN_POINT('Ctrl Pts',(223.509051615368,-66.982389656305,470.769804100533));
#49229=CARTESIAN_POINT('Ctrl Pts',(223.813692660408,-66.932003845745,471.229292332583));
#49230=CARTESIAN_POINT('Ctrl Pts',(223.970551922418,-66.93200726879,471.461346659833));
#49231=CARTESIAN_POINT('',(236.654571612597,-66.9320072687885,484.145366307158));
#49232=CARTESIAN_POINT('Origin',(263.115917770968,-66.93200726879,445.000000551893));
#49233=CARTESIAN_POINT('',(240.24303782791,-69.4723069190014,486.344850841488));
#49234=CARTESIAN_POINT('Ctrl Pts',(236.654571687298,-66.932007268787,484.145366364343));
#49235=CARTESIAN_POINT('Ctrl Pts',(236.884491926558,-66.932005368643,484.300783920973));
#49236=CARTESIAN_POINT('Ctrl Pts',(237.340761470018,-66.981556806277,484.603347584953));
#49237=CARTESIAN_POINT('Ctrl Pts',(238.019683045558,-67.201691318908,485.036861690703));
#49238=CARTESIAN_POINT('Ctrl Pts',(238.674342903578,-67.567693344638,485.439523031663));
#49239=CARTESIAN_POINT('Ctrl Pts',(239.282354749468,-68.073737286197,485.800402008113));
#49240=CARTESIAN_POINT('Ctrl Pts',(239.820546721509,-68.7114866004303,486.10952581754));
#49241=CARTESIAN_POINT('Ctrl Pts',(240.113391678348,-69.2053970132659,486.27311566556));
#49242=CARTESIAN_POINT('Ctrl Pts',(240.243087805294,-69.4718831208831,486.344858900952));
#49243=CARTESIAN_POINT('Origin',(263.115917770968,-69.47200726879,445.000000551893));
#49244=CARTESIAN_POINT('Origin',(263.115917770968,-56.01200726879,445.000000551893));
#49245=CARTESIAN_POINT('Origin',(263.115917770968,-69.47200726879,445.000000551893));
#49246=CARTESIAN_POINT('',(287.218198108558,-72.0120072687901,488.567467571773));
#49247=CARTESIAN_POINT('',(239.013637433378,-72.01200726879,488.567467571773));
#49248=CARTESIAN_POINT('Origin',(263.115917770968,-72.01200726879,445.000000551893));
#49249=CARTESIAN_POINT('Origin',(287.218198108558,-69.4720072687901,488.567467571773));
#49250=CARTESIAN_POINT('Origin',(239.013637433378,-69.47200726879,488.567467571773));
#49251=CARTESIAN_POINT('Origin',(263.115917770968,-72.01200726879,445.000000551893));
#49252=CARTESIAN_POINT('',(232.66750323717,-72.0120085167185,496.460000513384));
#49253=CARTESIAN_POINT('',(232.667503020318,-72.012008100742,496.460000551893));
#49254=CARTESIAN_POINT('',(293.564332521699,-72.0120076847427,496.460000551919));
#49255=CARTESIAN_POINT('',(293.564332521618,-72.0120081006951,496.460000551893));
#49256=CARTESIAN_POINT('',(287.218030147038,-72.0120072687901,488.567258682123));
#49257=CARTESIAN_POINT('Origin',(263.115917770968,-72.01200726879,445.000000551893));
#49258=CARTESIAN_POINT('',(306.683384791277,-72.0120072687908,469.102280888707));
#49259=CARTESIAN_POINT('',(306.683384791312,-72.0120072687919,420.897720215143));
#49260=CARTESIAN_POINT('Origin',(263.115917770968,-72.01200726879,445.000000551893));
#49261=CARTESIAN_POINT('',(314.575917732466,-72.0120093486708,475.448415085728));
#49262=CARTESIAN_POINT('',(314.575917770968,-72.0120081007421,475.448415302543));
#49263=CARTESIAN_POINT('',(314.575917770971,-72.012008516648,414.551585801181));
#49264=CARTESIAN_POINT('',(314.575917770968,-72.012008100695,414.551585801243));
#49265=CARTESIAN_POINT('',(306.683313170078,-72.01200726879,420.897777802283));
#49266=CARTESIAN_POINT('Origin',(263.115917770968,-72.01200726879,445.000000551893));
#49267=CARTESIAN_POINT('',(239.013637433378,-72.0120072687899,401.432533532013));
#49268=CARTESIAN_POINT('',(287.218198108558,-72.01200726879,401.432533532013));
#49269=CARTESIAN_POINT('Origin',(263.115917770968,-72.01200726879,445.000000551893));
#49270=CARTESIAN_POINT('',(293.564332304803,-72.0120093486707,393.540000590395));
#49271=CARTESIAN_POINT('',(293.564332521618,-72.012008100742,393.540000551893));
#49272=CARTESIAN_POINT('',(232.667503020229,-72.0120085166479,393.540000551878));
#49273=CARTESIAN_POINT('',(232.667503020318,-72.0120081006949,393.540000551893));
#49274=CARTESIAN_POINT('',(239.013805394898,-72.0120072687899,401.432742421663));
#49275=CARTESIAN_POINT('Origin',(263.115917770968,-72.01200726879,445.000000551893));
#49276=CARTESIAN_POINT('',(219.548450750635,-72.0120072687917,420.897720215124));
#49277=CARTESIAN_POINT('',(219.548450750735,-72.0120072687907,469.102280888843));
#49278=CARTESIAN_POINT('Origin',(263.115917770968,-72.01200726879,445.000000551893));
#49279=CARTESIAN_POINT('',(211.655917809477,-72.0120085167184,414.551586018095));
#49280=CARTESIAN_POINT('',(211.655917770968,-72.0120081007419,414.551585801243));
#49281=CARTESIAN_POINT('',(211.655917770966,-72.012008516648,475.448415302606));
#49282=CARTESIAN_POINT('',(211.655917770968,-72.012008100695,475.448415302543));
#49283=CARTESIAN_POINT('',(219.548478072158,-72.01200726879,469.102258921483));
#49284=CARTESIAN_POINT('Origin',(208.622849682388,-69.4720072687899,390.820344809323));
#49285=CARTESIAN_POINT('Origin',(287.218198108558,-69.4720072687901,488.567467571773));
#49286=CARTESIAN_POINT('',(297.495237745731,-70.7420027751341,497.838375097668));
#49287=CARTESIAN_POINT('Ctrl Pts',(297.495223246486,-70.7420072386772,497.838360765429));
#49288=CARTESIAN_POINT('Ctrl Pts',(297.430584327513,-70.8046621666009,497.815698843203));
#49289=CARTESIAN_POINT('Ctrl Pts',(297.360281447534,-70.8666202157765,497.791051170732));
#49290=CARTESIAN_POINT('Ctrl Pts',(297.28423434323,-70.927488967184,497.764391959688));
#49291=CARTESIAN_POINT('Ctrl Pts',(297.249478309544,-70.955307993216,497.752207821376));
#49292=CARTESIAN_POINT('Ctrl Pts',(297.213522928337,-70.9828991882139,497.739603111736));
#49293=CARTESIAN_POINT('Ctrl Pts',(297.176363170917,-71.0102237238982,497.726573251284));
#49294=CARTESIAN_POINT('Ctrl Pts',(297.099408625323,-71.0668104018838,497.699589571629));
#49295=CARTESIAN_POINT('Ctrl Pts',(297.017285377873,-71.1222548073893,497.670785396027));
#49296=CARTESIAN_POINT('Ctrl Pts',(296.930099031586,-71.17617908362,497.640217390304));
#49297=CARTESIAN_POINT('Ctrl Pts',(296.883067947229,-71.2052675509352,497.623728037131));
#49298=CARTESIAN_POINT('Ctrl Pts',(296.834564258945,-71.233913619238,497.606724878083));
#49299=CARTESIAN_POINT('Ctrl Pts',(296.784609466707,-71.2620580049096,497.589212848827));
#49300=CARTESIAN_POINT('Ctrl Pts',(296.710034719059,-71.304073202354,497.56307010848));
#49301=CARTESIAN_POINT('Ctrl Pts',(296.632228985522,-71.3449729686995,497.535790957057));
#49302=CARTESIAN_POINT('Ctrl Pts',(296.550979327238,-71.3847000761761,497.507298519727));
#49303=CARTESIAN_POINT('Ctrl Pts',(296.476907750018,-71.4209174532253,497.481323274828));
#49304=CARTESIAN_POINT('Ctrl Pts',(296.399973458015,-71.4561599907446,497.454339993113));
#49305=CARTESIAN_POINT('Ctrl Pts',(296.320005933237,-71.4903483914338,497.426297806313));
#49306=CARTESIAN_POINT('Ctrl Pts',(296.236163687569,-71.5261933459647,497.396896872354));
#49307=CARTESIAN_POINT('Ctrl Pts',(296.148991000274,-71.5608777497719,497.366328831849));
#49308=CARTESIAN_POINT('Ctrl Pts',(296.058184783034,-71.5942905948271,497.334485472522));
#49309=CARTESIAN_POINT('Ctrl Pts',(295.974225761459,-71.6251839616489,497.305043245171));
#49310=CARTESIAN_POINT('Ctrl Pts',(295.887160058519,-71.6549900460394,497.274511147639));
#49311=CARTESIAN_POINT('Ctrl Pts',(295.796743844254,-71.6835702845246,497.24280707608));
#49312=CARTESIAN_POINT('Ctrl Pts',(295.789370038573,-71.685901117845,497.240221481617));
#49313=CARTESIAN_POINT('Ctrl Pts',(295.781973948109,-71.6882237691193,497.237628092557));
#49314=CARTESIAN_POINT('Ctrl Pts',(295.774555440656,-71.6905381475854,497.235026864326));
#49315=CARTESIAN_POINT('Ctrl Pts',(295.684394659189,-71.7186659310274,497.203412854148));
#49316=CARTESIAN_POINT('Ctrl Pts',(295.590927640836,-71.7455720207983,497.170636985462));
#49317=CARTESIAN_POINT('Ctrl Pts',(295.493955551593,-71.7710584862261,497.136633017367));
#49318=CARTESIAN_POINT('Ctrl Pts',(295.400012919925,-71.7957487414619,497.103691350595));
#49319=CARTESIAN_POINT('Ctrl Pts',(295.302780415339,-71.8191066957974,497.069597425559));
#49320=CARTESIAN_POINT('Ctrl Pts',(295.20208695446,-71.8409047899498,497.034283224832));
#49321=CARTESIAN_POINT('Ctrl Pts',(295.179882407108,-71.8457116245701,497.026495868678));
#49322=CARTESIAN_POINT('Ctrl Pts',(295.157509613646,-71.8504424182202,497.018649132406));
#49323=CARTESIAN_POINT('Ctrl Pts',(295.13496683554,-71.8550944056927,497.010742209453));
#49324=CARTESIAN_POINT('Ctrl Pts',(295.029517193622,-71.876855273447,496.973755543918));
#49325=CARTESIAN_POINT('Ctrl Pts',(294.920346256765,-71.8968900354862,496.935453348788));
#49326=CARTESIAN_POINT('Ctrl Pts',(294.807768064222,-71.9148342843373,496.895973288881));
#49327=CARTESIAN_POINT('Ctrl Pts',(294.69684542964,-71.9325146477646,496.857073816796));
#49328=CARTESIAN_POINT('Ctrl Pts',(294.582615070484,-71.9481650394229,496.817030824154));
#49329=CARTESIAN_POINT('Ctrl Pts',(294.465415417878,-71.9614508713659,496.775945401434));
#49330=CARTESIAN_POINT('Ctrl Pts',(294.44178868109,-71.9641292142394,496.767662830225));
#49331=CARTESIAN_POINT('Ctrl Pts',(294.418041395273,-71.9667115210617,496.759337795346));
#49332=CARTESIAN_POINT('Ctrl Pts',(294.394176519811,-71.9691951485018,496.750970974903));
#49333=CARTESIAN_POINT('Ctrl Pts',(294.286409353994,-71.9804105219317,496.713188731813));
#49334=CARTESIAN_POINT('Ctrl Pts',(294.176244821695,-71.9896168634752,496.674554011708));
#49335=CARTESIAN_POINT('Ctrl Pts',(294.063676027197,-71.9965893765212,496.635082677501));
#49336=CARTESIAN_POINT('Ctrl Pts',(293.954872495805,-72.0033286691063,496.596931602244));
#49337=CARTESIAN_POINT('Ctrl Pts',(293.843822487108,-72.0079808733766,496.557999236117));
#49338=CARTESIAN_POINT('Ctrl Pts',(293.730541954548,-72.0103037875458,496.518282068601));
#49339=CARTESIAN_POINT('Ctrl Pts',(293.675660579299,-72.0114291770661,496.499040167764));
#49340=CARTESIAN_POINT('Ctrl Pts',(293.620256039227,-72.0120072687892,496.479613764687));
#49341=CARTESIAN_POINT('Ctrl Pts',(293.564332521698,-72.0120072687901,496.460000551921));
#49342=CARTESIAN_POINT('',(288.932517128318,-70.742010863496,487.189123540753));
#49343=CARTESIAN_POINT('Origin',(287.218198108558,-69.4720072687901,488.567467571773));
#49344=CARTESIAN_POINT('Origin',(214.070843635538,-72.0120072687899,390.575096505143));
#49345=CARTESIAN_POINT('Origin',(299.209522825618,-72.0120072687901,496.460000551893));
#49346=CARTESIAN_POINT('Origin',(299.209522825618,-72.0120072687901,496.460000551893));
#49347=CARTESIAN_POINT('',(299.209436229951,-72.0120048639454,499.000000169476));
#49348=CARTESIAN_POINT('Origin',(299.209530492038,-72.0119940551321,496.460000551893));
#49349=CARTESIAN_POINT('Origin',(299.209522825618,-72.0120072687901,496.460000551893));
#49350=CARTESIAN_POINT('Origin',(305.864311867508,-72.0120072687901,496.460000551893));
#49351=CARTESIAN_POINT('',(305.615917770278,-72.0120072687901,499.000000551893));
#49352=CARTESIAN_POINT('',(305.615917770278,-72.0120072687901,499.000000551893));
#49353=CARTESIAN_POINT('Origin',(305.615917770968,-72.0120072687901,496.460000551893));
#49354=CARTESIAN_POINT('Origin',(305.615917770968,-72.0120072687901,487.500000551893));
#49355=CARTESIAN_POINT('',(317.115917770969,-72.0120072687902,487.50000056716));
#49356=CARTESIAN_POINT('Origin',(305.615917770968,-72.0120072687901,487.500000551893));
#49357=CARTESIAN_POINT('Origin',(314.575917770968,-72.0120072687901,487.500000576913));
#49358=CARTESIAN_POINT('Origin',(305.615917770968,-69.4720072687901,487.500000551893));
#49359=CARTESIAN_POINT('',(305.615917770968,-85.4720072687901,499.000000551893));
#49360=CARTESIAN_POINT('',(317.115917770968,-85.4720072687901,487.500000551893));
#49361=CARTESIAN_POINT('Origin',(317.115917770968,-69.4720072687901,487.500000551893));
#49362=CARTESIAN_POINT('',(317.115917770968,-72.01200726879,402.500000552583));
#49363=CARTESIAN_POINT('',(317.115917388551,-72.0120048639453,408.90648209291));
#49364=CARTESIAN_POINT('',(317.115917770968,-72.01200726879,402.500000552583));
#49365=CARTESIAN_POINT('',(317.115921985178,-74.552007268779,414.551585800843));
#49366=CARTESIAN_POINT('Ctrl Pts',(317.115917292418,-72.012007955791,408.906503863893));
#49367=CARTESIAN_POINT('Ctrl Pts',(317.115920597578,-72.19552121824,409.042444578523));
#49368=CARTESIAN_POINT('Ctrl Pts',(317.115916447358,-72.553339671846,409.346292243203));
#49369=CARTESIAN_POINT('Ctrl Pts',(317.115918163698,-73.060368305257,409.910077792133));
#49370=CARTESIAN_POINT('Ctrl Pts',(317.115917523658,-73.517848719505,410.575025306713));
#49371=CARTESIAN_POINT('Ctrl Pts',(317.115918367468,-73.920471429642,411.354781495243));
#49372=CARTESIAN_POINT('Ctrl Pts',(317.115915632288,-74.254566710336,412.270129474193));
#49373=CARTESIAN_POINT('Ctrl Pts',(317.115925729188,-74.490207324085,413.339593273333));
#49374=CARTESIAN_POINT('Ctrl Pts',(317.115900627578,-74.551992485447,414.132916486413));
#49375=CARTESIAN_POINT('Ctrl Pts',(317.115921985178,-74.552007268779,414.551585800843));
#49376=CARTESIAN_POINT('',(317.115921689795,-74.5520072687783,475.448415303017));
#49377=CARTESIAN_POINT('',(317.115921985178,-74.552007268779,414.551585800843));
#49378=CARTESIAN_POINT('',(317.115917387258,-72.0120079573944,481.093518686536));
#49379=CARTESIAN_POINT('Ctrl Pts',(317.115921985308,-74.5520072687791,475.448415303033));
#49380=CARTESIAN_POINT('Ctrl Pts',(317.115900627238,-74.5519924846921,475.867084617403));
#49381=CARTESIAN_POINT('Ctrl Pts',(317.115925729348,-74.4902073241181,476.660407830253));
#49382=CARTESIAN_POINT('Ctrl Pts',(317.115915632248,-74.254566710358,477.729871629363));
#49383=CARTESIAN_POINT('Ctrl Pts',(317.115918367468,-73.9204714300721,478.645219608463));
#49384=CARTESIAN_POINT('Ctrl Pts',(317.115917523708,-73.5178487189331,479.424975796243));
#49385=CARTESIAN_POINT('Ctrl Pts',(317.115918163528,-73.0603683068281,480.089923312253));
#49386=CARTESIAN_POINT('Ctrl Pts',(317.115916447978,-72.5533396705431,480.653708859803));
#49387=CARTESIAN_POINT('Ctrl Pts',(317.115920596228,-72.1955212187221,480.957556521343));
#49388=CARTESIAN_POINT('Ctrl Pts',(317.115917292588,-72.0120079573931,481.093497241393));
#49389=CARTESIAN_POINT('',(317.115917292588,-72.0120079573931,481.093497241393));
#49390=CARTESIAN_POINT('',(317.115917770968,-85.47200726879,402.500000551893));
#49391=CARTESIAN_POINT('Origin',(314.575917770968,-72.01200726879,402.251606455353));
#49392=CARTESIAN_POINT('Origin',(314.575917770968,-72.01200726879,408.906395497243));
#49393=CARTESIAN_POINT('Origin',(314.575917770968,-72.01200726879,402.500000551893));
#49394=CARTESIAN_POINT('Origin',(305.615917770968,-72.01200726879,402.500000551893));
#49395=CARTESIAN_POINT('',(305.615917786235,-72.0120072687901,391.000000551892));
#49396=CARTESIAN_POINT('Origin',(305.615917770968,-72.01200726879,402.500000551893));
#49397=CARTESIAN_POINT('Origin',(305.615917795988,-72.01200726879,393.540000551893));
#49398=CARTESIAN_POINT('Origin',(305.615917770968,-69.47200726879,402.500000551893));
#49399=CARTESIAN_POINT('',(305.615917770968,-85.47200726879,391.000000551893));
#49400=CARTESIAN_POINT('Origin',(305.615917770968,-69.47200726879,391.000000551893));
#49401=CARTESIAN_POINT('',(293.564332522092,-74.5520072687782,390.999996633066));
#49402=CARTESIAN_POINT('',(299.209435905611,-72.0120079573942,391.000000935603));
#49403=CARTESIAN_POINT('Ctrl Pts',(293.564332522108,-74.5520072687789,390.999996337553));
#49404=CARTESIAN_POINT('Ctrl Pts',(293.983001836478,-74.551992484692,391.000017695623));
#49405=CARTESIAN_POINT('Ctrl Pts',(294.776325049328,-74.4902073241179,390.999992593513));
#49406=CARTESIAN_POINT('Ctrl Pts',(295.845788848438,-74.2545667103579,391.000002690613));
#49407=CARTESIAN_POINT('Ctrl Pts',(296.761136827538,-73.920471430072,390.999999955393));
#49408=CARTESIAN_POINT('Ctrl Pts',(297.540893015318,-73.517848718933,391.000000799153));
#49409=CARTESIAN_POINT('Ctrl Pts',(298.205840531328,-73.060368306828,391.000000159333));
#49410=CARTESIAN_POINT('Ctrl Pts',(298.769626078878,-72.553339670543,391.000001874883));
#49411=CARTESIAN_POINT('Ctrl Pts',(299.073473740418,-72.195521218722,390.999997726633));
#49412=CARTESIAN_POINT('Ctrl Pts',(299.209414460468,-72.012007957393,391.000001030273));
#49413=CARTESIAN_POINT('',(299.209414460468,-72.012007957393,391.000001030273));
#49414=CARTESIAN_POINT('',(232.667503019918,-74.5520072687789,390.999996337683));
#49415=CARTESIAN_POINT('Ctrl Pts',(227.022421082968,-72.0120079557909,391.000001030443));
#49416=CARTESIAN_POINT('Ctrl Pts',(227.158361797598,-72.1955212182399,390.999997725283));
#49417=CARTESIAN_POINT('Ctrl Pts',(227.462209462278,-72.5533396718459,391.000001875503));
#49418=CARTESIAN_POINT('Ctrl Pts',(228.025995011208,-73.0603683052569,391.000000159163));
#49419=CARTESIAN_POINT('Ctrl Pts',(228.690942525788,-73.5178487195049,391.000000799203));
#49420=CARTESIAN_POINT('Ctrl Pts',(229.470698714318,-73.9204714296419,390.999999955393));
#49421=CARTESIAN_POINT('Ctrl Pts',(230.386046693268,-74.2545667103359,391.000002690573));
#49422=CARTESIAN_POINT('Ctrl Pts',(231.455510492408,-74.4902073240849,390.999992593673));
#49423=CARTESIAN_POINT('Ctrl Pts',(232.248833705488,-74.5519924854469,391.000017695283));
#49424=CARTESIAN_POINT('Ctrl Pts',(232.667503019918,-74.5520072687789,390.999996337683));
#49425=CARTESIAN_POINT('',(232.667503019918,-74.5520072687789,390.999996337683));
#49426=CARTESIAN_POINT('Ctrl Pts',(293.403620000158,-74.713507444107,391.005206331223));
#49427=CARTESIAN_POINT('Ctrl Pts',(293.523253662578,-74.7444877320719,391.007066101423));
#49428=CARTESIAN_POINT('Ctrl Pts',(294.096491996468,-74.8792972330759,391.018187674123));
#49429=CARTESIAN_POINT('Ctrl Pts',(295.116742986068,-75.0078404229239,391.055676766553));
#49430=CARTESIAN_POINT('Ctrl Pts',(296.436962017788,-74.9488215722139,391.135288071793));
#49431=CARTESIAN_POINT('Ctrl Pts',(297.629286318478,-74.6941844595169,391.229364066743));
#49432=CARTESIAN_POINT('Ctrl Pts',(298.687681546088,-74.2773859025649,391.328484148293));
#49433=CARTESIAN_POINT('Ctrl Pts',(299.613647008578,-73.717781829922,391.426026814723));
#49434=CARTESIAN_POINT('Ctrl Pts',(300.228909735688,-73.1791351904629,391.496377994003));
#49435=CARTESIAN_POINT('Ctrl Pts',(300.530920362218,-72.841170440473,391.532173125083));
#49436=CARTESIAN_POINT('Ctrl Pts',(300.593570177078,-72.767200936835,391.539646373643));
#49437=CARTESIAN_POINT('Ctrl Pts',(293.435266749438,-73.0348243119389,390.897237502753));
#49438=CARTESIAN_POINT('Ctrl Pts',(293.531207702328,-73.0665839015929,390.880070293753));
#49439=CARTESIAN_POINT('Ctrl Pts',(293.992363219048,-73.2090046443279,390.801058739933));
#49440=CARTESIAN_POINT('Ctrl Pts',(294.824652130898,-73.3818065881169,390.686408027683));
#49441=CARTESIAN_POINT('Ctrl Pts',(295.922404003618,-73.4353515830609,390.584022189883));
#49442=CARTESIAN_POINT('Ctrl Pts',(296.929923102608,-73.326904152345,390.525172261023));
#49443=CARTESIAN_POINT('Ctrl Pts',(297.836986340198,-73.078553798327,390.497473304713));
#49444=CARTESIAN_POINT('Ctrl Pts',(298.640699611108,-72.7034694849989,390.491103395363));
#49445=CARTESIAN_POINT('Ctrl Pts',(299.180855751788,-72.31828963445,390.496606056823));
#49446=CARTESIAN_POINT('Ctrl Pts',(299.447631606278,-72.069395060257,390.501676649803));
#49447=CARTESIAN_POINT('Ctrl Pts',(299.503042114118,-72.014632724146,390.502823399773));
#49448=CARTESIAN_POINT('Ctrl Pts',(293.457348103978,-71.8635323633289,392.104816764133));
#49449=CARTESIAN_POINT('Ctrl Pts',(293.537031632768,-71.8812991757079,392.074367240203));
#49450=CARTESIAN_POINT('Ctrl Pts',(293.918365156668,-71.960042879052,391.931270597373));
#49451=CARTESIAN_POINT('Ctrl Pts',(294.593238217918,-72.047682887232,391.699013943113));
#49452=CARTESIAN_POINT('Ctrl Pts',(295.459642360368,-72.0525390584189,391.438419217373));
#49453=CARTESIAN_POINT('Ctrl Pts',(296.236766415788,-71.958291489615,391.232931397543));
#49454=CARTESIAN_POINT('Ctrl Pts',(296.922378360948,-71.779984113589,391.072990588673));
#49455=CARTESIAN_POINT('Ctrl Pts',(297.518836711668,-71.526452518351,390.950035877043));
#49456=CARTESIAN_POINT('Ctrl Pts',(297.913123545478,-71.274222914498,390.878004465333));
#49457=CARTESIAN_POINT('Ctrl Pts',(298.106123060458,-71.1135155794619,390.845098548043));
#49458=CARTESIAN_POINT('Ctrl Pts',(298.146136149308,-71.0782444347639,390.838373797913));
#49459=CARTESIAN_POINT('Ctrl Pts',(293.454354624918,-72.0223202985269,393.779768035813));
#49460=CARTESIAN_POINT('Ctrl Pts',(293.536634858248,-72.021150461685,393.751110055733));
#49461=CARTESIAN_POINT('Ctrl Pts',(293.926472357468,-72.009654141941,393.614988263533));
#49462=CARTESIAN_POINT('Ctrl Pts',(294.585041091708,-71.942527322552,393.382263256273));
#49463=CARTESIAN_POINT('Ctrl Pts',(295.373710291988,-71.7716399178189,393.098370205453));
#49464=CARTESIAN_POINT('Ctrl Pts',(296.036673675948,-71.5496287323249,392.855527631373));
#49465=CARTESIAN_POINT('Ctrl Pts',(296.586257353848,-71.293762522114,392.650805810713));
#49466=CARTESIAN_POINT('Ctrl Pts',(297.036029175858,-71.0134407520789,392.480480571413));
#49467=CARTESIAN_POINT('Ctrl Pts',(297.316139250318,-70.780263637391,392.372687692493));
#49468=CARTESIAN_POINT('Ctrl Pts',(297.448639673388,-70.644919903199,392.321227125813));
#49469=CARTESIAN_POINT('Ctrl Pts',(297.475912026518,-70.6157338063319,392.310614635863));
#49470=CARTESIAN_POINT('',(297.495234411945,-70.7420091884828,392.161623914219));
#49471=CARTESIAN_POINT('Ctrl Pts',(293.564332521712,-72.0120105965991,393.540000551893));
#49472=CARTESIAN_POINT('Ctrl Pts',(293.610180177156,-72.0120088645519,393.523921124626));
#49473=CARTESIAN_POINT('Ctrl Pts',(293.655679608989,-72.0116188869948,393.507964757136));
#49474=CARTESIAN_POINT('Ctrl Pts',(293.700828127475,-72.0108586572667,393.492132222862));
#49475=CARTESIAN_POINT('Ctrl Pts',(293.821427560535,-72.0088279533303,393.449840809511));
#49476=CARTESIAN_POINT('Ctrl Pts',(293.939519908192,-72.0041577141726,393.408434113532));
#49477=CARTESIAN_POINT('Ctrl Pts',(294.05507958132,-71.9971271823479,393.367917803027));
#49478=CARTESIAN_POINT('Ctrl Pts',(294.170639254449,-71.9900966505231,393.327401492523));
#49479=CARTESIAN_POINT('Ctrl Pts',(294.283666851026,-71.9807057284239,393.28777534827));
#49480=CARTESIAN_POINT('Ctrl Pts',(294.394177386595,-71.9692011295368,393.24903082564));
#49481=CARTESIAN_POINT('Ctrl Pts',(294.469689910043,-71.9613399668995,393.222556456852));
#49482=CARTESIAN_POINT('Ctrl Pts',(294.544023221346,-71.9524908559285,393.196494275085));
#49483=CARTESIAN_POINT('Ctrl Pts',(294.61708943307,-71.9427410029954,393.170874910482));
#49484=CARTESIAN_POINT('Ctrl Pts',(294.720519831422,-71.9289393955364,393.134608885136));
#49485=CARTESIAN_POINT('Ctrl Pts',(294.821408954925,-71.9133317336542,393.099230965762));
#49486=CARTESIAN_POINT('Ctrl Pts',(294.919510626567,-71.8961610227596,393.06482701592));
#49487=CARTESIAN_POINT('Ctrl Pts',(294.992918738488,-71.8833124194074,393.039083020347));
#49488=CARTESIAN_POINT('Ctrl Pts',(295.064767002146,-71.8695891220288,393.013884055383));
#49489=CARTESIAN_POINT('Ctrl Pts',(295.13496867765,-71.8551008150858,392.989260375731));
#49490=CARTESIAN_POINT('Ctrl Pts',(295.23044268125,-71.8353967744157,392.955772267892));
#49491=CARTESIAN_POINT('Ctrl Pts',(295.322858820816,-71.8142817745928,392.923362377343));
#49492=CARTESIAN_POINT('Ctrl Pts',(295.412369258352,-71.7919537135011,392.891974213068));
#49493=CARTESIAN_POINT('Ctrl Pts',(295.508894470344,-71.767875841807,392.858126213951));
#49494=CARTESIAN_POINT('Ctrl Pts',(295.602039818024,-71.7423873942477,392.825466660148));
#49495=CARTESIAN_POINT('Ctrl Pts',(295.691974537143,-71.7156824432709,392.793932532312));
#49496=CARTESIAN_POINT('Ctrl Pts',(295.719807600318,-71.707417775355,392.784173327181));
#49497=CARTESIAN_POINT('Ctrl Pts',(295.747333405952,-71.6990363146507,392.774521827672));
#49498=CARTESIAN_POINT('Ctrl Pts',(295.774557578644,-71.6905430693269,392.764975958906));
#49499=CARTESIAN_POINT('Ctrl Pts',(295.865554257107,-71.6621544338826,392.7330689342));
#49500=CARTESIAN_POINT('Ctrl Pts',(295.953168415807,-71.6325246163829,392.702345484388));
#49501=CARTESIAN_POINT('Ctrl Pts',(296.037660773368,-71.601797552647,392.67271616762));
#49502=CARTESIAN_POINT('Ctrl Pts',(296.052067301209,-71.5965583770343,392.667664165413));
#49503=CARTESIAN_POINT('Ctrl Pts',(296.066383106193,-71.591287185193,392.662643959429));
#49504=CARTESIAN_POINT('Ctrl Pts',(296.080609518588,-71.5859845479236,392.657655092465));
#49505=CARTESIAN_POINT('Ctrl Pts',(296.163364197678,-71.5551392417853,392.628634980214));
#49506=CARTESIAN_POINT('Ctrl Pts',(296.243092687893,-71.5232336033096,392.600675798085));
#49507=CARTESIAN_POINT('Ctrl Pts',(296.320007651119,-71.4903512772879,392.5737046794));
#49508=CARTESIAN_POINT('Ctrl Pts',(296.405578887035,-71.4537682619746,392.54369813889));
#49509=CARTESIAN_POINT('Ctrl Pts',(296.487669371849,-71.4159779683996,392.51490829633));
#49510=CARTESIAN_POINT('Ctrl Pts',(296.566499322963,-71.3770761149287,392.487264268723));
#49511=CARTESIAN_POINT('Ctrl Pts',(296.590594755396,-71.365185241364,392.47881450071));
#49512=CARTESIAN_POINT('Ctrl Pts',(296.614385651394,-71.3531901564309,392.470471746746));
#49513=CARTESIAN_POINT('Ctrl Pts',(296.637878473138,-71.341092656553,392.462233905615));
#49514=CARTESIAN_POINT('Ctrl Pts',(296.688139289384,-71.3152111245251,392.444609772429));
#49515=CARTESIAN_POINT('Ctrl Pts',(296.73703559184,-71.2888614634883,392.427465915853));
#49516=CARTESIAN_POINT('Ctrl Pts',(296.784610174726,-71.2620589084764,392.410788823981));
#49517=CARTESIAN_POINT('Ctrl Pts',(296.856519361253,-71.2215467313672,392.385581327932));
#49518=CARTESIAN_POINT('Ctrl Pts',(296.92542409753,-71.1799959836175,392.361421243769));
#49519=CARTESIAN_POINT('Ctrl Pts',(296.991253732561,-71.1375810950574,392.338337811185));
#49520=CARTESIAN_POINT('Ctrl Pts',(297.02886740447,-71.113346117884,392.325148422251));
#49521=CARTESIAN_POINT('Ctrl Pts',(297.065478074462,-71.088829010672,392.312310191884));
#49522=CARTESIAN_POINT('Ctrl Pts',(297.101079686947,-71.0640622089105,392.299825987935));
#49523=CARTESIAN_POINT('Ctrl Pts',(297.126698112609,-71.0462403624964,392.290842528241));
#49524=CARTESIAN_POINT('Ctrl Pts',(297.151794116107,-71.0282892411028,392.282042358285));
#49525=CARTESIAN_POINT('Ctrl Pts',(297.176362709175,-71.0102232726032,392.273427484222));
#49526=CARTESIAN_POINT('Ctrl Pts',(297.238139349407,-70.9647971941419,392.251765764558));
#49527=CARTESIAN_POINT('Ctrl Pts',(297.296594249163,-70.9186326263586,392.231273559932));
#49528=CARTESIAN_POINT('Ctrl Pts',(297.351737586078,-70.8719111276471,392.211942525523));
#49529=CARTESIAN_POINT('Ctrl Pts',(297.39400288267,-70.8361008537176,392.19712601371));
#49530=CARTESIAN_POINT('Ctrl Pts',(297.434323915126,-70.7999629729411,392.182991257644));
#49531=CARTESIAN_POINT('Ctrl Pts',(297.47272325268,-70.7635713397337,392.169528477904));
#49532=CARTESIAN_POINT('Ctrl Pts',(297.4802977877,-70.7563928382873,392.16687285145));
#49533=CARTESIAN_POINT('Ctrl Pts',(297.487797592225,-70.7492044430814,392.164243357357));
#49534=CARTESIAN_POINT('Ctrl Pts',(297.495222765696,-70.7420068815995,392.161639947474));
#49535=CARTESIAN_POINT('Ctrl Pts',(299.209414460475,-72.012007957416,391.000001627217));
#49536=CARTESIAN_POINT('Ctrl Pts',(299.163364790386,-71.9753249175646,391.000003616177));
#49537=CARTESIAN_POINT('Ctrl Pts',(299.116494777333,-71.9392458075241,391.002052727671));
#49538=CARTESIAN_POINT('Ctrl Pts',(299.069205430033,-71.9036114492888,391.006195158111));
#49539=CARTESIAN_POINT('Ctrl Pts',(299.022239451589,-71.8682207620344,391.010309262236));
#49540=CARTESIAN_POINT('Ctrl Pts',(298.974860013137,-71.8332687556906,391.016488185206));
#49541=CARTESIAN_POINT('Ctrl Pts',(298.927438390979,-71.7986331412756,391.024745193473));
#49542=CARTESIAN_POINT('Ctrl Pts',(298.88006471894,-71.7640325484769,391.03299385271));
#49543=CARTESIAN_POINT('Ctrl Pts',(298.832649141448,-71.7297478280264,391.043316415269));
#49544=CARTESIAN_POINT('Ctrl Pts',(298.785537542146,-71.6956899506139,391.055693654232));
#49545=CARTESIAN_POINT('Ctrl Pts',(298.759718399476,-71.6770247978908,391.062476903016));
#49546=CARTESIAN_POINT('Ctrl Pts',(298.733990114611,-71.6584283466725,391.069876702762));
#49547=CARTESIAN_POINT('Ctrl Pts',(298.708406203038,-71.6398898461304,391.077885749038));
#49548=CARTESIAN_POINT('Ctrl Pts',(298.641042885633,-71.5910773378212,391.098973842814));
#49549=CARTESIAN_POINT('Ctrl Pts',(298.574726333039,-71.5425836661342,391.124291348115));
#49550=CARTESIAN_POINT('Ctrl Pts',(298.509739437054,-71.4947553753244,391.153715969436));
#49551=CARTESIAN_POINT('Ctrl Pts',(298.446007898098,-71.4478509874047,391.182572193011));
#49552=CARTESIAN_POINT('Ctrl Pts',(298.383555320484,-71.4015866110902,391.215378436927));
#49553=CARTESIAN_POINT('Ctrl Pts',(298.322651474073,-71.3562721759616,391.25197246669));
#49554=CARTESIAN_POINT('Ctrl Pts',(298.292576717278,-71.3338955824275,391.270042861421));
#49555=CARTESIAN_POINT('Ctrl Pts',(298.262879642304,-71.3117503575619,391.289036158411));
#49556=CARTESIAN_POINT('Ctrl Pts',(298.233592745105,-71.2898721306231,391.308928412373));
#49557=CARTESIAN_POINT('Ctrl Pts',(298.179041925794,-71.2491209647858,391.345980434111));
#49558=CARTESIAN_POINT('Ctrl Pts',(298.125921199044,-71.2092859907837,391.386153790494));
#49559=CARTESIAN_POINT('Ctrl Pts',(298.074355627012,-71.1706830835568,391.429272972365));
#49560=CARTESIAN_POINT('Ctrl Pts',(298.022037552681,-71.131516839683,391.473021397396));
#49561=CARTESIAN_POINT('Ctrl Pts',(297.97132087597,-71.0936188702448,391.519802373784));
#49562=CARTESIAN_POINT('Ctrl Pts',(297.92234701012,-71.0572796433853,391.569397266211));
#49563=CARTESIAN_POINT('Ctrl Pts',(297.88768363514,-71.0315589814523,391.60450019965));
#49564=CARTESIAN_POINT('Ctrl Pts',(297.853893622557,-71.0066183661927,391.641012067787));
#49565=CARTESIAN_POINT('Ctrl Pts',(297.821027833467,-70.9825493079028,391.678844594721));
#49566=CARTESIAN_POINT('Ctrl Pts',(297.783852322583,-70.9553240513914,391.721638136449));
#49567=CARTESIAN_POINT('Ctrl Pts',(297.74783219056,-70.9292507855693,391.766122622644));
#49568=CARTESIAN_POINT('Ctrl Pts',(297.713249741123,-70.9041908400237,391.812136771624));
#49569=CARTESIAN_POINT('Ctrl Pts',(297.677888662821,-70.8785666661705,391.859186935841));
#49570=CARTESIAN_POINT('Ctrl Pts',(297.644030742679,-70.854002558325,391.907836549861));
#49571=CARTESIAN_POINT('Ctrl Pts',(297.611937753492,-70.8303782654378,391.957887372366));
#49572=CARTESIAN_POINT('Ctrl Pts',(297.578945979081,-70.8060923587238,392.009339901004));
#49573=CARTESIAN_POINT('Ctrl Pts',(297.547819508731,-70.7828005038815,392.062273279665));
#49574=CARTESIAN_POINT('Ctrl Pts',(297.518799775462,-70.760390068132,392.116443580042));
#49575=CARTESIAN_POINT('Ctrl Pts',(297.510781411271,-70.7541979011033,392.131411229564));
#49576=CARTESIAN_POINT('Ctrl Pts',(297.502923633929,-70.7480730855497,392.146473147346));
#49577=CARTESIAN_POINT('Ctrl Pts',(297.495230955743,-70.7420133331691,392.161623817083));
#49578=CARTESIAN_POINT('Origin',(293.564332522078,-74.552013924409,393.540000551893));
#49579=CARTESIAN_POINT('Origin',(297.262553908368,-69.47200726879,388.940612583843));
#49580=CARTESIAN_POINT('',(288.932479187181,-70.7420814892878,402.810893549063));
#49581=CARTESIAN_POINT('Origin',(287.218198108558,-69.47200726879,401.432533532013));
#49582=CARTESIAN_POINT('',(297.495223127598,-70.7420071496969,392.161640238453));
#49583=CARTESIAN_POINT('Origin',(287.218198108558,-69.47200726879,401.432533532013));
#49584=CARTESIAN_POINT('Origin',(287.218198108558,-69.47200726879,401.432533532013));
#49585=CARTESIAN_POINT('Origin',(287.218166972068,-69.4721721185271,401.432510673503));
#49586=CARTESIAN_POINT('Ctrl Pts',(291.203645131898,-69.4654484632099,403.635357625233));
#49587=CARTESIAN_POINT('Ctrl Pts',(291.173051143578,-69.4642529784631,403.617755948263));
#49588=CARTESIAN_POINT('Ctrl Pts',(290.972859048508,-69.461131317104,403.503668639343));
#49589=CARTESIAN_POINT('Ctrl Pts',(290.594946600108,-69.5121743079279,403.301685955943));
#49590=CARTESIAN_POINT('Ctrl Pts',(290.084964756368,-69.7115095210406,403.057939922303));
#49591=CARTESIAN_POINT('Ctrl Pts',(289.611953752488,-70.0335847626073,402.855968300073));
#49592=CARTESIAN_POINT('Ctrl Pts',(289.246049537548,-70.4242464530172,402.715633112443));
#49593=CARTESIAN_POINT('Ctrl Pts',(289.064520043938,-70.713413234504,402.651065852173));
#49594=CARTESIAN_POINT('Ctrl Pts',(288.998413612038,-70.840779768824,402.628068939403));
#49595=CARTESIAN_POINT('Ctrl Pts',(290.254313491288,-69.6040686220959,405.017443465873));
#49596=CARTESIAN_POINT('Ctrl Pts',(290.227163648548,-69.6012555491032,405.002376957633));
#49597=CARTESIAN_POINT('Ctrl Pts',(290.049137019188,-69.5867035136386,404.904544662123));
#49598=CARTESIAN_POINT('Ctrl Pts',(289.707639443108,-69.605895880883,404.728653457343));
#49599=CARTESIAN_POINT('Ctrl Pts',(289.225829971688,-69.7468138148854,404.504512583233));
#49600=CARTESIAN_POINT('Ctrl Pts',(288.753707550808,-70.0122251216757,404.303173476413));
#49601=CARTESIAN_POINT('Ctrl Pts',(288.366767689408,-70.3697189200571,404.149170983363));
#49602=CARTESIAN_POINT('Ctrl Pts',(288.166452102968,-70.653842506004,404.072518279053));
#49603=CARTESIAN_POINT('Ctrl Pts',(288.092556015588,-70.781931585494,404.044593288783));
#49604=CARTESIAN_POINT('Ctrl Pts',(289.621245193278,-68.419135189814,406.030249678763));
#49605=CARTESIAN_POINT('Ctrl Pts',(289.582956330878,-68.41446975451,406.006060540213));
#49606=CARTESIAN_POINT('Ctrl Pts',(289.332024190148,-68.389529900869,405.848495325453));
#49607=CARTESIAN_POINT('Ctrl Pts',(288.852027174878,-68.410079767087,405.558979345753));
#49608=CARTESIAN_POINT('Ctrl Pts',(288.174342656098,-68.6071111008892,405.175179965833));
#49609=CARTESIAN_POINT('Ctrl Pts',(287.507154848008,-68.9922445608695,404.816936851443));
#49610=CARTESIAN_POINT('Ctrl Pts',(286.956624676828,-69.522348198985,404.533699690253));
#49611=CARTESIAN_POINT('Ctrl Pts',(286.670012222648,-69.9492631288261,404.389800539313));
#49612=CARTESIAN_POINT('Ctrl Pts',(286.564094264238,-70.1425137073577,404.337074995393));
#49613=CARTESIAN_POINT('Ctrl Pts',(289.749096409928,-66.742924819268,405.962398778943));
#49614=CARTESIAN_POINT('Ctrl Pts',(289.692909216458,-66.737473314687,405.923836788043));
#49615=CARTESIAN_POINT('Ctrl Pts',(289.325208151628,-66.710484421782,405.672506085923));
#49616=CARTESIAN_POINT('Ctrl Pts',(288.629076985118,-66.764646425836,405.209457145263));
#49617=CARTESIAN_POINT('Ctrl Pts',(287.669049228958,-67.092908761381,404.598876954383));
#49618=CARTESIAN_POINT('Ctrl Pts',(286.747852601878,-67.690059702462,404.036399957943));
#49619=CARTESIAN_POINT('Ctrl Pts',(286.006080448558,-68.4773127599906,403.599132951133));
#49620=CARTESIAN_POINT('Ctrl Pts',(285.626273772118,-69.0945594144157,403.380059086583));
#49621=CARTESIAN_POINT('Ctrl Pts',(285.486593332898,-69.3716421412076,403.300079990813));
#49622=CARTESIAN_POINT('Ctrl Pts',(290.999733508293,-69.4720072796082,403.750310918259));
#49623=CARTESIAN_POINT('Ctrl Pts',(290.872577534336,-69.472005849716,403.678659148785));
#49624=CARTESIAN_POINT('Ctrl Pts',(290.743479119672,-69.4843168520742,403.608952691824));
#49625=CARTESIAN_POINT('Ctrl Pts',(290.573417073416,-69.5166114182824,403.52069155269));
#49626=CARTESIAN_POINT('Ctrl Pts',(290.532260427764,-69.5256727717997,403.499602683094));
#49627=CARTESIAN_POINT('Ctrl Pts',(290.403656894431,-69.5579244915856,403.434557401163));
#49628=CARTESIAN_POINT('Ctrl Pts',(290.316431600513,-69.5855055086998,403.391675607924));
#49629=CARTESIAN_POINT('Ctrl Pts',(290.149149606719,-69.6496600928294,403.311655708688));
#49630=CARTESIAN_POINT('Ctrl Pts',(290.069003164979,-69.6855216028275,403.274325295143));
#49631=CARTESIAN_POINT('Ctrl Pts',(289.944724104076,-69.7495837444736,403.217895622591));
#49632=CARTESIAN_POINT('Ctrl Pts',(289.899775287176,-69.7745536342543,403.197796416373));
#49633=CARTESIAN_POINT('Ctrl Pts',(289.739386970048,-69.8703147051977,403.127097475838));
#49634=CARTESIAN_POINT('Ctrl Pts',(289.62693747088,-69.950164289824,403.079509070807));
#49635=CARTESIAN_POINT('Ctrl Pts',(289.514831043793,-70.0443954690097,403.033665288188));
#49636=CARTESIAN_POINT('Ctrl Pts',(289.509507836765,-70.0489065579999,403.031492461485));
#49637=CARTESIAN_POINT('Ctrl Pts',(289.392695719642,-70.1487082562832,402.983898553237));
#49638=CARTESIAN_POINT('Ctrl Pts',(289.287584575188,-70.2548440769942,402.942824966919));
#49639=CARTESIAN_POINT('Ctrl Pts',(289.16570429737,-70.4011757050269,402.896533092463));
#49640=CARTESIAN_POINT('Ctrl Pts',(289.140508058321,-70.4328767762964,402.887047510866));
#49641=CARTESIAN_POINT('Ctrl Pts',(289.049504035329,-70.5529932331026,402.853066472181));
#49642=CARTESIAN_POINT('Ctrl Pts',(288.988121244777,-70.6454659295424,402.830716147373));
#49643=CARTESIAN_POINT('Ctrl Pts',(288.932529004827,-70.7420200540542,402.810888197655));
#49644=CARTESIAN_POINT('Origin',(290.999736346768,-66.932007290493,403.750312537073));
#49645=CARTESIAN_POINT('Origin',(301.593507745258,-72.01200726879,390.575096505143));
#49646=CARTESIAN_POINT('Origin',(299.209522825618,-72.01200726879,393.540000551893));
#49647=CARTESIAN_POINT('Origin',(299.209522825618,-72.01200726879,393.540000551893));
#49648=CARTESIAN_POINT('Origin',(299.209522825618,-72.01200726879,393.540000551893));
#49649=CARTESIAN_POINT('Origin',(220.367523674428,-72.0120072687899,393.540000551893));
#49650=CARTESIAN_POINT('Origin',(263.115917770968,-66.93200726879,445.000000551893));
#49651=CARTESIAN_POINT('Origin',(304.365605883138,-66.93200726879,417.116182114513));
#49652=CARTESIAN_POINT('Ctrl Pts',(305.487892930988,-70.84102555105,419.117632653513));
#49653=CARTESIAN_POINT('Ctrl Pts',(305.464850568738,-70.713370333766,419.051393351193));
#49654=CARTESIAN_POINT('Ctrl Pts',(305.400366416118,-70.4246254735271,418.870097571243));
#49655=CARTESIAN_POINT('Ctrl Pts',(305.260591345888,-70.03536275261,418.505648539213));
#49656=CARTESIAN_POINT('Ctrl Pts',(305.059765698908,-69.713847880508,418.035004394313));
#49657=CARTESIAN_POINT('Ctrl Pts',(304.816679242508,-69.5133172296705,417.525769821493));
#49658=CARTESIAN_POINT('Ctrl Pts',(304.613886321128,-69.461221631883,417.145987521843));
#49659=CARTESIAN_POINT('Ctrl Pts',(304.498796499068,-69.4642140921142,416.943973415093));
#49660=CARTESIAN_POINT('Ctrl Pts',(304.480695707958,-69.4654397984238,416.912510521983));
#49661=CARTESIAN_POINT('Ctrl Pts',(304.071378819998,-70.782178593213,420.023505505583));
#49662=CARTESIAN_POINT('Ctrl Pts',(304.043397780898,-70.653795640172,419.949459441043));
#49663=CARTESIAN_POINT('Ctrl Pts',(303.966843753868,-70.3700937613876,419.749402599143));
#49664=CARTESIAN_POINT('Ctrl Pts',(303.813452007048,-70.0138432466799,419.363994547833));
#49665=CARTESIAN_POINT('Ctrl Pts',(303.613137828218,-69.7486471121801,418.894056400303));
#49666=CARTESIAN_POINT('Ctrl Pts',(303.389433232488,-69.6065541583208,418.412681539603));
#49667=CARTESIAN_POINT('Ctrl Pts',(303.212782003088,-69.5866015108646,418.069396475333));
#49668=CARTESIAN_POINT('Ctrl Pts',(303.114084903818,-69.6011568594992,417.889736153403));
#49669=CARTESIAN_POINT('Ctrl Pts',(303.098591120058,-69.604046788924,417.861814842233));
#49670=CARTESIAN_POINT('Ctrl Pts',(303.778945393968,-70.1428866111332,421.552028656883));
#49671=CARTESIAN_POINT('Ctrl Pts',(303.726113566768,-69.9491917586301,421.445895462313));
#49672=CARTESIAN_POINT('Ctrl Pts',(303.582399730018,-69.5229124456986,421.159653521583));
#49673=CARTESIAN_POINT('Ctrl Pts',(303.300284792268,-68.9946418506595,420.611300963493));
#49674=CARTESIAN_POINT('Ctrl Pts',(302.943787010338,-68.6097419549074,419.947170649373));
#49675=CARTESIAN_POINT('Ctrl Pts',(302.560567407998,-68.410944976237,419.270074416423));
#49676=CARTESIAN_POINT('Ctrl Pts',(302.269706171108,-68.389326074635,418.787576198633));
#49677=CARTESIAN_POINT('Ctrl Pts',(302.110731762418,-68.414305770954,418.534345416843));
#49678=CARTESIAN_POINT('Ctrl Pts',(302.085856285908,-68.419099312278,418.494968636633));
#49679=CARTESIAN_POINT('Ctrl Pts',(304.815992739688,-69.3721770309352,422.629594373163));
#49680=CARTESIAN_POINT('Ctrl Pts',(304.735852768918,-69.0944600428793,422.489631115633));
#49681=CARTESIAN_POINT('Ctrl Pts',(304.517061054368,-68.4781267582278,422.110314934323));
#49682=CARTESIAN_POINT('Ctrl Pts',(304.081529312988,-67.693627670349,421.371481733023));
#49683=CARTESIAN_POINT('Ctrl Pts',(303.521853468128,-67.097079327632,420.454658245163));
#49684=CARTESIAN_POINT('Ctrl Pts',(302.912262522438,-66.766264510463,419.495730799533));
#49685=CARTESIAN_POINT('Ctrl Pts',(302.447058675868,-66.710340497794,418.796089905903));
#49686=CARTESIAN_POINT('Ctrl Pts',(302.193474645818,-66.737284122907,418.425039014543));
#49687=CARTESIAN_POINT('Ctrl Pts',(302.153818312178,-66.742883601451,418.367255833933));
#49688=CARTESIAN_POINT('',(305.30504375147,-70.7420553610057,419.183412677393));
#49689=CARTESIAN_POINT('Origin',(306.683409048718,-69.4721778291691,420.897753867533));
#49690=CARTESIAN_POINT('Ctrl Pts',(305.305042220708,-70.742010897001,419.183399964073));
#49691=CARTESIAN_POINT('Ctrl Pts',(305.277815995278,-70.609423932929,419.107063253613));
#49692=CARTESIAN_POINT('Ctrl Pts',(305.213936898318,-70.3602758137963,418.932833631543));
#49693=CARTESIAN_POINT('Ctrl Pts',(305.091118039558,-70.0432002664174,418.618591900583));
#49694=CARTESIAN_POINT('Ctrl Pts',(304.942919608568,-69.791339768846,418.267516581863));
#49695=CARTESIAN_POINT('Ctrl Pts',(304.771191547518,-69.6083606197754,417.892354850793));
#49696=CARTESIAN_POINT('Ctrl Pts',(304.578280667416,-69.4970261598067,417.504572957698));
#49697=CARTESIAN_POINT('Ctrl Pts',(304.437924443537,-69.4720061889132,417.244522589505));
#49698=CARTESIAN_POINT('Ctrl Pts',(304.365607433868,-69.4720072829599,417.116184866493));
#49699=CARTESIAN_POINT('Origin',(208.730420887858,-72.01200726879,494.013388642063));
#49700=CARTESIAN_POINT('',(315.954292413807,-70.7420026857022,410.620680697854));
#49701=CARTESIAN_POINT('',(305.305042220708,-70.742010897001,419.183399964073));
#49702=CARTESIAN_POINT('Origin',(314.575917770968,-72.01200726879,408.906395497243));
#49703=CARTESIAN_POINT('Origin',(314.575917770968,-72.01200726879,408.906395497243));
#49704=CARTESIAN_POINT('Origin',(314.575917770968,-72.011994055132,408.906387830823));
#49705=CARTESIAN_POINT('Ctrl Pts',(316.576327554178,-72.767751257,407.522814320583));
#49706=CARTESIAN_POINT('Ctrl Pts',(316.583782922478,-72.841526713075,407.585316356403));
#49707=CARTESIAN_POINT('Ctrl Pts',(316.619560336498,-73.179288192142,407.887183345043));
#49708=CARTESIAN_POINT('Ctrl Pts',(316.689891498608,-73.717781820139,408.502271310003));
#49709=CARTESIAN_POINT('Ctrl Pts',(316.787434179168,-74.277385903423,409.428236779663));
#49710=CARTESIAN_POINT('Ctrl Pts',(316.886554255398,-74.694184456929,410.486632004843));
#49711=CARTESIAN_POINT('Ctrl Pts',(316.980630255158,-74.948821569849,411.678956305813));
#49712=CARTESIAN_POINT('Ctrl Pts',(317.060241543218,-75.007840422917,412.999175337793));
#49713=CARTESIAN_POINT('Ctrl Pts',(317.097721793168,-74.879327723335,414.019184250283));
#49714=CARTESIAN_POINT('Ctrl Pts',(317.108843213778,-74.744596630044,414.592201564763));
#49715=CARTESIAN_POINT('Ctrl Pts',(317.110701299278,-74.713685427546,414.711610886703));
#49716=CARTESIAN_POINT('Ctrl Pts',(317.613103449168,-72.015040141213,408.613288514213));
#49717=CARTESIAN_POINT('Ctrl Pts',(317.614247001878,-72.069657434211,408.668567963553));
#49718=CARTESIAN_POINT('Ctrl Pts',(317.619313854468,-72.318399048559,408.935215997553));
#49719=CARTESIAN_POINT('Ctrl Pts',(317.624814914728,-72.703469476734,409.475218706333));
#49720=CARTESIAN_POINT('Ctrl Pts',(317.618445020368,-73.078553800105,410.278931984853));
#49721=CARTESIAN_POINT('Ctrl Pts',(317.590746058588,-73.326904151249,411.185995219963));
#49722=CARTESIAN_POINT('Ctrl Pts',(317.531896134968,-73.435351582353,412.193514319393));
#49723=CARTESIAN_POINT('Ctrl Pts',(317.429510279318,-73.381806590394,413.291266192613));
#49724=CARTESIAN_POINT('Ctrl Pts',(317.314886825698,-73.209045637398,414.123357625123));
#49725=CARTESIAN_POINT('Ctrl Pts',(317.235911832778,-73.066698954042,414.584338071243));
#49726=CARTESIAN_POINT('Ctrl Pts',(317.218779455948,-73.035006784976,414.680100276573));
#49727=CARTESIAN_POINT('Ctrl Pts',(317.277494481808,-71.078506845443,409.970079907573));
#49728=CARTESIAN_POINT('Ctrl Pts',(317.270785073228,-71.113684992587,410.009998731183));
#49729=CARTESIAN_POINT('Ctrl Pts',(317.237893413858,-71.274294562834,410.202906766823));
#49730=CARTESIAN_POINT('Ctrl Pts',(317.165882438868,-71.526452514999,410.597081606803));
#49731=CARTESIAN_POINT('Ctrl Pts',(317.042927735698,-71.779984116282,411.193539961963));
#49732=CARTESIAN_POINT('Ctrl Pts',(316.882986923958,-71.958291490743,411.879151906023));
#49733=CARTESIAN_POINT('Ctrl Pts',(316.677499107228,-72.052539059859,412.656275961963));
#49734=CARTESIAN_POINT('Ctrl Pts',(316.416904371818,-72.047682890276,413.522680104983));
#49735=CARTESIAN_POINT('Ctrl Pts',(316.184702855868,-71.960063670979,414.197393038243));
#49736=CARTESIAN_POINT('Ctrl Pts',(316.041666670348,-71.881362788512,414.578578626823));
#49737=CARTESIAN_POINT('Ctrl Pts',(316.011276520298,-71.863634441064,414.658112344523));
#49738=CARTESIAN_POINT('Ctrl Pts',(315.805224721488,-70.615950955131,410.640209231163));
#49739=CARTESIAN_POINT('Ctrl Pts',(315.794636946478,-70.645062585471,410.667418342263));
#49740=CARTESIAN_POINT('Ctrl Pts',(315.743200015988,-70.780329866031,410.799858625583));
#49741=CARTESIAN_POINT('Ctrl Pts',(315.635437754638,-71.013440751854,411.079889146753));
#49742=CARTESIAN_POINT('Ctrl Pts',(315.465112514288,-71.293762523166,411.529660968353));
#49743=CARTESIAN_POINT('Ctrl Pts',(315.260390694088,-71.549628732834,412.079244646643));
#49744=CARTESIAN_POINT('Ctrl Pts',(315.017548119678,-71.771639918357,412.742208030733));
#49745=CARTESIAN_POINT('Ctrl Pts',(314.733655070238,-71.942527322346,413.530877231093));
#49746=CARTESIAN_POINT('Ctrl Pts',(314.500985277318,-72.009638215756,414.189289707313));
#49747=CARTESIAN_POINT('Ctrl Pts',(314.364918237878,-72.021141169012,414.578968533643));
#49748=CARTESIAN_POINT('Ctrl Pts',(314.336314960658,-72.022313562161,414.661090911573));
#49749=CARTESIAN_POINT('Ctrl Pts',(315.954278372765,-70.7420068809478,410.620695559264));
#49750=CARTESIAN_POINT('Ctrl Pts',(315.951674963195,-70.7492044424186,410.628120732305));
#49751=CARTESIAN_POINT('Ctrl Pts',(315.949045469402,-70.7563928376237,410.635620536423));
#49752=CARTESIAN_POINT('Ctrl Pts',(315.946389843238,-70.7635713390688,410.643195071058));
#49753=CARTESIAN_POINT('Ctrl Pts',(315.928825029924,-70.8110513042364,410.693294474588));
#49754=CARTESIAN_POINT('Ctrl Pts',(315.910115871374,-70.8580999963981,410.746666500798));
#49755=CARTESIAN_POINT('Ctrl Pts',(315.890242304815,-70.9045511124985,410.803356320062));
#49756=CARTESIAN_POINT('Ctrl Pts',(315.875009939518,-70.9401542019987,410.846807002811));
#49757=CARTESIAN_POINT('Ctrl Pts',(315.85909374957,-70.975405861412,410.892206097532));
#49758=CARTESIAN_POINT('Ctrl Pts',(315.842490840838,-71.0102232739626,410.939555612702));
#49759=CARTESIAN_POINT('Ctrl Pts',(315.833875966783,-71.0282892423347,410.964124205851));
#49760=CARTESIAN_POINT('Ctrl Pts',(315.825075796751,-71.0462403635193,410.98922020942));
#49761=CARTESIAN_POINT('Ctrl Pts',(315.816092336927,-71.0640622097132,411.014838635134));
#49762=CARTESIAN_POINT('Ctrl Pts',(315.794243070786,-71.1074078992631,411.077146900826));
#49763=CARTESIAN_POINT('Ctrl Pts',(315.771308437755,-71.1499888075381,411.142548617801));
#49764=CARTESIAN_POINT('Ctrl Pts',(315.747307516489,-71.1916308944392,411.211001129355));
#49765=CARTESIAN_POINT('Ctrl Pts',(315.733593917851,-71.2154242671948,411.250113389202));
#49766=CARTESIAN_POINT('Ctrl Pts',(315.719532516711,-71.2389111258158,411.290220793764));
#49767=CARTESIAN_POINT('Ctrl Pts',(315.705129498392,-71.2620589077046,411.331308147898));
#49768=CARTESIAN_POINT('Ctrl Pts',(315.688452406246,-71.2888614627661,411.378882730932));
#49769=CARTESIAN_POINT('Ctrl Pts',(315.671308549575,-71.3152111239888,411.427779033538));
#49770=CARTESIAN_POINT('Ctrl Pts',(315.653684416389,-71.3410926562256,411.478039849955));
#49771=CARTESIAN_POINT('Ctrl Pts',(315.626733718716,-71.3806705091198,411.554898328823));
#49772=CARTESIAN_POINT('Ctrl Pts',(315.598659847284,-71.4191559802297,411.634947740602));
#49773=CARTESIAN_POINT('Ctrl Pts',(315.569390399603,-71.4564687983853,411.718411883613));
#49774=CARTESIAN_POINT('Ctrl Pts',(315.560443806303,-71.4678739541145,411.743923801391));
#49775=CARTESIAN_POINT('Ctrl Pts',(315.551385540596,-71.4791691936542,411.769754688635));
#49776=CARTESIAN_POINT('Ctrl Pts',(315.54221364373,-71.4903512773119,411.795910671373));
#49777=CARTESIAN_POINT('Ctrl Pts',(315.515242525184,-71.5232336034354,411.8728256347));
#49778=CARTESIAN_POINT('Ctrl Pts',(315.487283343028,-71.5551392419007,411.952554125022));
#49779=CARTESIAN_POINT('Ctrl Pts',(315.458263230685,-71.5859845480198,412.035308804217));
#49780=CARTESIAN_POINT('Ctrl Pts',(315.429004195628,-71.6170838036807,412.118744803052));
#49781=CARTESIAN_POINT('Ctrl Pts',(315.398666821627,-71.6471054203413,412.205256651372));
#49782=CARTESIAN_POINT('Ctrl Pts',(315.367160717853,-71.6759139021885,412.295107683839));
#49783=CARTESIAN_POINT('Ctrl Pts',(315.361788708047,-71.6808259486952,412.310427909753));
#49784=CARTESIAN_POINT('Ctrl Pts',(315.356382733281,-71.6857026097516,412.325845178458));
#49785=CARTESIAN_POINT('Ctrl Pts',(315.350942364032,-71.6905430691911,412.341360743912));
#49786=CARTESIAN_POINT('Ctrl Pts',(315.320097573025,-71.7179866034364,412.429328003468));
#49787=CARTESIAN_POINT('Ctrl Pts',(315.288149145133,-71.7442659054153,412.520446812886));
#49788=CARTESIAN_POINT('Ctrl Pts',(315.255030549156,-71.769198804243,412.614896704636));
#49789=CARTESIAN_POINT('Ctrl Pts',(315.244780981062,-71.7769150566009,412.644127128461));
#49790=CARTESIAN_POINT('Ctrl Pts',(315.234419413948,-71.7845020756706,412.673676369388));
#49791=CARTESIAN_POINT('Ctrl Pts',(315.223944109765,-71.7919537134942,412.703549064507));
#49792=CARTESIAN_POINT('Ctrl Pts',(315.192555945547,-71.814281774581,412.793059501975));
#49793=CARTESIAN_POINT('Ctrl Pts',(315.160146055062,-71.8353967743902,412.88547564147));
#49794=CARTESIAN_POINT('Ctrl Pts',(315.126657947258,-71.855100815038,412.980949644988));
#49795=CARTESIAN_POINT('Ctrl Pts',(315.093751173053,-71.874462805279,413.074766276684));
#49796=CARTESIAN_POINT('Ctrl Pts',(315.059816408482,-71.8924577821927,413.171525236941));
#49797=CARTESIAN_POINT('Ctrl Pts',(315.024927819642,-71.9088265655513,413.271013891659));
#49798=CARTESIAN_POINT('Ctrl Pts',(314.998821176152,-71.9210750973982,413.345459861713));
#49799=CARTESIAN_POINT('Ctrl Pts',(314.972180772578,-71.9324134528439,413.421433367158));
#49800=CARTESIAN_POINT('Ctrl Pts',(314.945043412244,-71.9427410029756,413.498828889789));
#49801=CARTESIAN_POINT('Ctrl Pts',(314.919424047628,-71.9524908559149,413.571895101447));
#49802=CARTESIAN_POINT('Ctrl Pts',(314.89336186585,-71.9613399669071,413.64622841268));
#49803=CARTESIAN_POINT('Ctrl Pts',(314.86688749706,-71.9692011295698,413.721740936061));
#49804=CARTESIAN_POINT('Ctrl Pts',(314.828142974388,-71.980705728506,413.832251471643));
#49805=CARTESIAN_POINT('Ctrl Pts',(314.788516830115,-71.99009665066,413.945279068244));
#49806=CARTESIAN_POINT('Ctrl Pts',(314.748000519617,-71.9971271824969,414.060838741406));
#49807=CARTESIAN_POINT('Ctrl Pts',(314.70748420912,-72.0041577143339,414.176398414569));
#49808=CARTESIAN_POINT('Ctrl Pts',(314.666077513173,-72.0088279534613,414.294490762271));
#49809=CARTESIAN_POINT('Ctrl Pts',(314.623786099889,-72.0108586572646,414.415090195384));
#49810=CARTESIAN_POINT('Ctrl Pts',(314.607953565646,-72.0116188869426,414.460238713869));
#49811=CARTESIAN_POINT('Ctrl Pts',(314.591997198208,-72.012008864435,414.505738145661));
#49812=CARTESIAN_POINT('Ctrl Pts',(314.575917770983,-72.0120105964115,414.551585801107));
#49813=CARTESIAN_POINT('Origin',(314.575917770968,-74.55200726879,414.551585801123));
#49814=CARTESIAN_POINT('Origin',(314.575917770968,-74.55200726879,402.251606455353));
#49815=CARTESIAN_POINT('Origin',(314.575917770968,-74.5520139244091,475.448415303003));
#49816=CARTESIAN_POINT('Ctrl Pts',(317.110711991638,-74.7135074441071,475.287702781083));
#49817=CARTESIAN_POINT('Ctrl Pts',(317.108852221438,-74.7444877320721,475.407336443503));
#49818=CARTESIAN_POINT('Ctrl Pts',(317.097730648738,-74.879297233076,475.980574777393));
#49819=CARTESIAN_POINT('Ctrl Pts',(317.060241556308,-75.0078404229241,477.000825766993));
#49820=CARTESIAN_POINT('Ctrl Pts',(316.980630251068,-74.9488215722141,478.321044798713));
#49821=CARTESIAN_POINT('Ctrl Pts',(316.886554256118,-74.6941844595181,479.513369099403));
#49822=CARTESIAN_POINT('Ctrl Pts',(316.787434174568,-74.2773859025651,480.571764327013));
#49823=CARTESIAN_POINT('Ctrl Pts',(316.689891508138,-73.7177818299221,481.497729789503));
#49824=CARTESIAN_POINT('Ctrl Pts',(316.619540328858,-73.1791351904631,482.112992516613));
#49825=CARTESIAN_POINT('Ctrl Pts',(316.583745197778,-72.8411704404731,482.415003143143));
#49826=CARTESIAN_POINT('Ctrl Pts',(316.576271949218,-72.7672009368351,482.477652958003));
#49827=CARTESIAN_POINT('Ctrl Pts',(317.218680820108,-73.034824311939,475.319349530363));
#49828=CARTESIAN_POINT('Ctrl Pts',(317.235848029108,-73.066583901593,475.415290483253));
#49829=CARTESIAN_POINT('Ctrl Pts',(317.314859582928,-73.209004644328,475.876445999973));
#49830=CARTESIAN_POINT('Ctrl Pts',(317.429510295178,-73.3818065881171,476.708734911823));
#49831=CARTESIAN_POINT('Ctrl Pts',(317.531896132978,-73.435351583061,477.806486784543));
#49832=CARTESIAN_POINT('Ctrl Pts',(317.590746061838,-73.3269041523451,478.814005883533));
#49833=CARTESIAN_POINT('Ctrl Pts',(317.618445018148,-73.0785537983271,479.721069121113));
#49834=CARTESIAN_POINT('Ctrl Pts',(317.624814927498,-72.7034694849991,480.524782392033));
#49835=CARTESIAN_POINT('Ctrl Pts',(317.619312266038,-72.3182896344501,481.064938532713));
#49836=CARTESIAN_POINT('Ctrl Pts',(317.614241673058,-72.0693950602571,481.331714387203));
#49837=CARTESIAN_POINT('Ctrl Pts',(317.613094923088,-72.0146327241461,481.387124895043));
#49838=CARTESIAN_POINT('Ctrl Pts',(316.011101558728,-71.8635323633291,475.341430884903));
#49839=CARTESIAN_POINT('Ctrl Pts',(316.041551082658,-71.8812991757081,475.421114413693));
#49840=CARTESIAN_POINT('Ctrl Pts',(316.184647725488,-71.9600428790521,475.802447937593));
#49841=CARTESIAN_POINT('Ctrl Pts',(316.416904379748,-72.0476828872321,476.477320998843));
#49842=CARTESIAN_POINT('Ctrl Pts',(316.677499105488,-72.0525390584191,477.343725141293));
#49843=CARTESIAN_POINT('Ctrl Pts',(316.882986925318,-71.9582914896151,478.120849196703));
#49844=CARTESIAN_POINT('Ctrl Pts',(317.042927734188,-71.7799841135891,478.806461141873));
#49845=CARTESIAN_POINT('Ctrl Pts',(317.165882445818,-71.5264525183511,479.402919492593));
#49846=CARTESIAN_POINT('Ctrl Pts',(317.237913857528,-71.2742229144981,479.797206326403));
#49847=CARTESIAN_POINT('Ctrl Pts',(317.270819774818,-71.1135155794621,479.990205841383));
#49848=CARTESIAN_POINT('Ctrl Pts',(317.277544524948,-71.0782444347641,480.030218930233));
#49849=CARTESIAN_POINT('Ctrl Pts',(314.336150287048,-72.0223202985271,475.338437405843));
#49850=CARTESIAN_POINT('Ctrl Pts',(314.364808267128,-72.0211504616851,475.420717639173));
#49851=CARTESIAN_POINT('Ctrl Pts',(314.500930059328,-72.009654141941,475.810555138393));
#49852=CARTESIAN_POINT('Ctrl Pts',(314.733655066588,-71.9425273225521,476.469123872633));
#49853=CARTESIAN_POINT('Ctrl Pts',(315.017548117408,-71.7716399178201,477.257793072913));
#49854=CARTESIAN_POINT('Ctrl Pts',(315.260390691488,-71.549628732325,477.920756456873));
#49855=CARTESIAN_POINT('Ctrl Pts',(315.465112512148,-71.2937625221141,478.470340134773));
#49856=CARTESIAN_POINT('Ctrl Pts',(315.635437751448,-71.0134407520801,478.920111956783));
#49857=CARTESIAN_POINT('Ctrl Pts',(315.743230630368,-70.7802636373911,479.200222031243));
#49858=CARTESIAN_POINT('Ctrl Pts',(315.794691197048,-70.6449199031991,479.332722454313));
#49859=CARTESIAN_POINT('Ctrl Pts',(315.805303686998,-70.6157338063321,479.359994807443));
#49860=CARTESIAN_POINT('',(315.954294408643,-70.7420091884829,479.37931719287));
#49861=CARTESIAN_POINT('Ctrl Pts',(314.575917770969,-72.0120105965992,475.448415302637));
#49862=CARTESIAN_POINT('Ctrl Pts',(314.591997198235,-72.012008864552,475.494262958081));
#49863=CARTESIAN_POINT('Ctrl Pts',(314.607953565725,-72.0116188869949,475.539762389914));
#49864=CARTESIAN_POINT('Ctrl Pts',(314.6237861,-72.0108586572668,475.5849109084));
#49865=CARTESIAN_POINT('Ctrl Pts',(314.66607751335,-72.0088279533304,475.70551034146));
#49866=CARTESIAN_POINT('Ctrl Pts',(314.70748420933,-72.0041577141727,475.823602689117));
#49867=CARTESIAN_POINT('Ctrl Pts',(314.748000519834,-71.997127182348,475.939162362245));
#49868=CARTESIAN_POINT('Ctrl Pts',(314.788516830339,-71.9900966505232,476.054722035374));
#49869=CARTESIAN_POINT('Ctrl Pts',(314.828142974591,-71.9807057284241,476.167749631951));
#49870=CARTESIAN_POINT('Ctrl Pts',(314.866887497221,-71.969201129537,476.27826016752));
#49871=CARTESIAN_POINT('Ctrl Pts',(314.89336186601,-71.9613399668997,476.353772690968));
#49872=CARTESIAN_POINT('Ctrl Pts',(314.919424047776,-71.9524908559287,476.428106002271));
#49873=CARTESIAN_POINT('Ctrl Pts',(314.945043412379,-71.9427410029957,476.501172213995));
#49874=CARTESIAN_POINT('Ctrl Pts',(314.981309437727,-71.9289393955363,476.604602612351));
#49875=CARTESIAN_POINT('Ctrl Pts',(315.016687357102,-71.9133317336536,476.705491735856));
#49876=CARTESIAN_POINT('Ctrl Pts',(315.051091306944,-71.8961610227584,476.803593407501));
#49877=CARTESIAN_POINT('Ctrl Pts',(315.076835302516,-71.8833124194068,476.877001519419));
#49878=CARTESIAN_POINT('Ctrl Pts',(315.102034267479,-71.8695891220288,476.948849783074));
#49879=CARTESIAN_POINT('Ctrl Pts',(315.12665794713,-71.8551008150864,477.019051458575));
#49880=CARTESIAN_POINT('Ctrl Pts',(315.160146054969,-71.8353967744164,477.114525462175));
#49881=CARTESIAN_POINT('Ctrl Pts',(315.192555945518,-71.8142817745934,477.206941601741));
#49882=CARTESIAN_POINT('Ctrl Pts',(315.223944109793,-71.7919537135017,477.296452039276));
#49883=CARTESIAN_POINT('Ctrl Pts',(315.25779210891,-71.7678758418075,477.39297725127));
#49884=CARTESIAN_POINT('Ctrl Pts',(315.290451662713,-71.742387394248,477.486122598949));
#49885=CARTESIAN_POINT('Ctrl Pts',(315.32198579055,-71.715682443271,477.576057318069));
#49886=CARTESIAN_POINT('Ctrl Pts',(315.33174499568,-71.7074177753551,477.603890381244));
#49887=CARTESIAN_POINT('Ctrl Pts',(315.34139649519,-71.6990363146508,477.631416186877));
#49888=CARTESIAN_POINT('Ctrl Pts',(315.350942363955,-71.690543069327,477.658640359569));
#49889=CARTESIAN_POINT('Ctrl Pts',(315.382849388659,-71.6621544338846,477.749637038026));
#49890=CARTESIAN_POINT('Ctrl Pts',(315.413572838469,-71.6325246163871,477.83725119672));
#49891=CARTESIAN_POINT('Ctrl Pts',(315.443202155235,-71.6017975526535,477.921743554275));
#49892=CARTESIAN_POINT('Ctrl Pts',(315.448254157444,-71.5965583770387,477.936150082122));
#49893=CARTESIAN_POINT('Ctrl Pts',(315.453274363431,-71.5912871851952,477.950465887112));
#49894=CARTESIAN_POINT('Ctrl Pts',(315.458263230396,-71.5859845479237,477.964692299512));
#49895=CARTESIAN_POINT('Ctrl Pts',(315.487283342647,-71.5551392417853,478.047446978603));
#49896=CARTESIAN_POINT('Ctrl Pts',(315.515242524777,-71.5232336033097,478.127175468818));
#49897=CARTESIAN_POINT('Ctrl Pts',(315.542213643461,-71.4903512772878,478.204090432044));
#49898=CARTESIAN_POINT('Ctrl Pts',(315.572220183972,-71.4537682619738,478.289661667962));
#49899=CARTESIAN_POINT('Ctrl Pts',(315.601010026533,-71.4159779683979,478.371752152777));
#49900=CARTESIAN_POINT('Ctrl Pts',(315.62865405414,-71.3770761149262,478.450582103894));
#49901=CARTESIAN_POINT('Ctrl Pts',(315.637103822152,-71.3651852413623,478.474677536325));
#49902=CARTESIAN_POINT('Ctrl Pts',(315.645446576115,-71.3531901564301,478.498468432321));
#49903=CARTESIAN_POINT('Ctrl Pts',(315.653684417246,-71.341092656553,478.521961254064));
#49904=CARTESIAN_POINT('Ctrl Pts',(315.671308550432,-71.3152111245253,478.572222070309));
#49905=CARTESIAN_POINT('Ctrl Pts',(315.688452407008,-71.2888614634885,478.621118372765));
#49906=CARTESIAN_POINT('Ctrl Pts',(315.70512949888,-71.2620589084766,478.668692955651));
#49907=CARTESIAN_POINT('Ctrl Pts',(315.730336994929,-71.2215467313676,478.740602142178));
#49908=CARTESIAN_POINT('Ctrl Pts',(315.754497079091,-71.1799959836181,478.809506878454));
#49909=CARTESIAN_POINT('Ctrl Pts',(315.777580511676,-71.1375810950581,478.875336513486));
#49910=CARTESIAN_POINT('Ctrl Pts',(315.790769900609,-71.1133461178848,478.912950185394));
#49911=CARTESIAN_POINT('Ctrl Pts',(315.803608130977,-71.0888290106729,478.949560855386));
#49912=CARTESIAN_POINT('Ctrl Pts',(315.816092334926,-71.0640622089115,478.985162467871));
#49913=CARTESIAN_POINT('Ctrl Pts',(315.82507579462,-71.0462403624972,479.010780893534));
#49914=CARTESIAN_POINT('Ctrl Pts',(315.833875964576,-71.0282892411033,479.035876897032));
#49915=CARTESIAN_POINT('Ctrl Pts',(315.842490838639,-71.0102232726035,479.060445490101));
#49916=CARTESIAN_POINT('Ctrl Pts',(315.864152558303,-70.9647971941416,479.122222130333));
#49917=CARTESIAN_POINT('Ctrl Pts',(315.88464476293,-70.9186326263578,479.18067703009));
#49918=CARTESIAN_POINT('Ctrl Pts',(315.903975797339,-70.8719111276457,479.235820367005));
#49919=CARTESIAN_POINT('Ctrl Pts',(315.918792309151,-70.8361008537166,479.278085663597));
#49920=CARTESIAN_POINT('Ctrl Pts',(315.932927065217,-70.7999629729406,479.318406696052));
#49921=CARTESIAN_POINT('Ctrl Pts',(315.946389844957,-70.7635713397338,479.356806033605));
#49922=CARTESIAN_POINT('Ctrl Pts',(315.949045471411,-70.7563928382873,479.364380568625));
#49923=CARTESIAN_POINT('Ctrl Pts',(315.951674965504,-70.7492044430815,479.37188037315));
#49924=CARTESIAN_POINT('Ctrl Pts',(315.954278375387,-70.7420068815996,479.379305546621));
#49925=CARTESIAN_POINT('Ctrl Pts',(317.115916695644,-72.0120079574161,481.0934972414));
#49926=CARTESIAN_POINT('Ctrl Pts',(317.115914706685,-71.975324917565,481.047447571311));
#49927=CARTESIAN_POINT('Ctrl Pts',(317.11386559519,-71.9392458075248,481.000577558259));
#49928=CARTESIAN_POINT('Ctrl Pts',(317.10972316475,-71.9036114492898,480.953288210959));
#49929=CARTESIAN_POINT('Ctrl Pts',(317.105609060625,-71.8682207620356,480.906322232516));
#49930=CARTESIAN_POINT('Ctrl Pts',(317.099430137655,-71.833268755692,480.858942794064));
#49931=CARTESIAN_POINT('Ctrl Pts',(317.091173129388,-71.7986331412772,480.811521171906));
#49932=CARTESIAN_POINT('Ctrl Pts',(317.082924470151,-71.7640325484783,480.764147499867));
#49933=CARTESIAN_POINT('Ctrl Pts',(317.072601907592,-71.7297478280276,480.716731922374));
#49934=CARTESIAN_POINT('Ctrl Pts',(317.060224668629,-71.6956899506149,480.669620323073));
#49935=CARTESIAN_POINT('Ctrl Pts',(317.053441419845,-71.6770247978915,480.643801180401));
#49936=CARTESIAN_POINT('Ctrl Pts',(317.046041620099,-71.6584283466728,480.618072895536));
#49937=CARTESIAN_POINT('Ctrl Pts',(317.038032573823,-71.6398898461305,480.592488983963));
#49938=CARTESIAN_POINT('Ctrl Pts',(317.016944480046,-71.5910773378187,480.525125666554));
#49939=CARTESIAN_POINT('Ctrl Pts',(316.991626974743,-71.5425836661291,480.458809113957));
#49940=CARTESIAN_POINT('Ctrl Pts',(316.96220235342,-71.4947553753167,480.393822217968));
#49941=CARTESIAN_POINT('Ctrl Pts',(316.933346129845,-71.4478509873964,480.330090679011));
#49942=CARTESIAN_POINT('Ctrl Pts',(316.900539885927,-71.4015866110813,480.267638101397));
#49943=CARTESIAN_POINT('Ctrl Pts',(316.863945856163,-71.3562721759521,480.206734254986));
#49944=CARTESIAN_POINT('Ctrl Pts',(316.845875461435,-71.3338955824212,480.176659498195));
#49945=CARTESIAN_POINT('Ctrl Pts',(316.826882164448,-71.3117503575587,480.146962423224));
#49946=CARTESIAN_POINT('Ctrl Pts',(316.806989910488,-71.289872130623,480.11767552603));
#49947=CARTESIAN_POINT('Ctrl Pts',(316.769937888749,-71.2491209647852,480.063124706718));
#49948=CARTESIAN_POINT('Ctrl Pts',(316.729764532366,-71.2092859907826,480.010003979968));
#49949=CARTESIAN_POINT('Ctrl Pts',(316.686645350494,-71.1706830835551,479.958438407935));
#49950=CARTESIAN_POINT('Ctrl Pts',(316.642896925465,-71.1315168396827,479.906120333606));
#49951=CARTESIAN_POINT('Ctrl Pts',(316.596115949078,-71.0936188702458,479.855403656897));
#49952=CARTESIAN_POINT('Ctrl Pts',(316.546521056654,-71.0572796433875,479.806429791048));
#49953=CARTESIAN_POINT('Ctrl Pts',(316.511418123213,-71.0315589814536,479.771766416068));
#49954=CARTESIAN_POINT('Ctrl Pts',(316.474906255075,-71.0066183661931,479.737976403483));
#49955=CARTESIAN_POINT('Ctrl Pts',(316.437073728139,-70.9825493079024,479.705110614392));
#49956=CARTESIAN_POINT('Ctrl Pts',(316.394280186412,-70.9553240513913,479.667935103509));
#49957=CARTESIAN_POINT('Ctrl Pts',(316.349795700217,-70.9292507855694,479.631914971486));
#49958=CARTESIAN_POINT('Ctrl Pts',(316.303781551238,-70.904190840024,479.597332522048));
#49959=CARTESIAN_POINT('Ctrl Pts',(316.256731387022,-70.8785666661709,479.561971443747));
#49960=CARTESIAN_POINT('Ctrl Pts',(316.208081773002,-70.8540025583256,479.528113523605));
#49961=CARTESIAN_POINT('Ctrl Pts',(316.158030950496,-70.8303782654384,479.496020534418));
#49962=CARTESIAN_POINT('Ctrl Pts',(316.106578421861,-70.8060923587252,479.463028760008));
#49963=CARTESIAN_POINT('Ctrl Pts',(316.053645043201,-70.7828005038837,479.431902289659));
#49964=CARTESIAN_POINT('Ctrl Pts',(315.999474742825,-70.7603900681349,479.402882556391));
#49965=CARTESIAN_POINT('Ctrl Pts',(315.984507093301,-70.7541979011052,479.394864192198));
#49966=CARTESIAN_POINT('Ctrl Pts',(315.969445175518,-70.7480730855507,479.387006414855));
#49967=CARTESIAN_POINT('Ctrl Pts',(315.954294505778,-70.7420133331691,479.379313736668));
#49968=CARTESIAN_POINT('Origin',(319.112977972408,-69.4720072687901,479.096520917133));
#49969=CARTESIAN_POINT('',(305.305026691757,-70.7420844489581,470.816561545459));
#49970=CARTESIAN_POINT('Origin',(306.683384790848,-69.47200726879,469.102280889483));
#49971=CARTESIAN_POINT('',(315.954278084408,-70.7420071496971,479.379305908523));
#49972=CARTESIAN_POINT('Origin',(306.683384790848,-69.47200726879,469.102280889483));
#49973=CARTESIAN_POINT('Origin',(306.683384790848,-69.47200726879,469.102280889483));
#49974=CARTESIAN_POINT('Origin',(306.683409153898,-69.4721780198136,469.102247046603));
#49975=CARTESIAN_POINT('Ctrl Pts',(304.480558603038,-69.4654490974856,473.087728863913));
#49976=CARTESIAN_POINT('Ctrl Pts',(304.498705664228,-69.4642164587728,473.056187095803));
#49977=CARTESIAN_POINT('Ctrl Pts',(304.613843052118,-69.4612105224026,472.854094590153));
#49978=CARTESIAN_POINT('Ctrl Pts',(304.816679229658,-69.513317227736,472.474231273923));
#49979=CARTESIAN_POINT('Ctrl Pts',(305.059765686868,-69.7138478877062,471.964996701443));
#49980=CARTESIAN_POINT('Ctrl Pts',(305.260591333288,-70.0353627268994,471.494352561143));
#49981=CARTESIAN_POINT('Ctrl Pts',(305.400342602498,-70.4245592719201,471.129965573733));
#49982=CARTESIAN_POINT('Ctrl Pts',(305.464816219258,-70.7132164602071,470.948704299693));
#49983=CARTESIAN_POINT('Ctrl Pts',(305.487849475208,-70.840784784687,470.882493350613));
#49984=CARTESIAN_POINT('Ctrl Pts',(303.098473769598,-69.6040686792588,472.138397726133));
#49985=CARTESIAN_POINT('Ctrl Pts',(303.114007019468,-69.6011683474859,472.110406731753));
#49986=CARTESIAN_POINT('Ctrl Pts',(303.212744305738,-69.5865972268538,471.930677833983));
#49987=CARTESIAN_POINT('Ctrl Pts',(303.389433235448,-69.6065541544155,471.587319568593));
#49988=CARTESIAN_POINT('Ctrl Pts',(303.613137828168,-69.7486471104222,471.105944697023));
#49989=CARTESIAN_POINT('Ctrl Pts',(303.813452001428,-70.0138432058711,470.636006546653));
#49990=CARTESIAN_POINT('Ctrl Pts',(303.966817657268,-70.3700332044193,470.250664139543));
#49991=CARTESIAN_POINT('Ctrl Pts',(304.043356984828,-70.653644403435,470.050648159123));
#49992=CARTESIAN_POINT('Ctrl Pts',(304.071326011608,-70.78193644975,469.976635184693));
#49993=CARTESIAN_POINT('Ctrl Pts',(302.085667889648,-68.419135632178,471.505330697043));
#49994=CARTESIAN_POINT('Ctrl Pts',(302.110606322998,-68.414325499387,471.465855536483));
#49995=CARTESIAN_POINT('Ctrl Pts',(302.269644108638,-68.389321427153,471.212527796443));
#49996=CARTESIAN_POINT('Ctrl Pts',(302.560567421638,-68.410944983966,470.729926704453));
#49997=CARTESIAN_POINT('Ctrl Pts',(302.943787016688,-68.6097419631934,470.052830454643));
#49998=CARTESIAN_POINT('Ctrl Pts',(303.300284786528,-68.9946417969067,469.388700136083));
#49999=CARTESIAN_POINT('Ctrl Pts',(303.582351736368,-69.5228226663637,468.840440988033));
#50000=CARTESIAN_POINT('Ctrl Pts',(303.726036985068,-69.9489645106605,468.554258016843));
#50001=CARTESIAN_POINT('Ctrl Pts',(303.778845690928,-70.1425212887321,468.448172524813));
#50002=CARTESIAN_POINT('Ctrl Pts',(302.153517964228,-66.742926046005,471.633182901113));
#50003=CARTESIAN_POINT('Ctrl Pts',(302.193274540738,-66.737305414815,471.575254910373));
#50004=CARTESIAN_POINT('Ctrl Pts',(302.446959418678,-66.710328544982,471.204060407683));
#50005=CARTESIAN_POINT('Ctrl Pts',(302.912262528458,-66.766264527055,470.504270319133));
#50006=CARTESIAN_POINT('Ctrl Pts',(303.521853466188,-67.097079350092,469.545342858733));
#50007=CARTESIAN_POINT('Ctrl Pts',(304.081529296598,-67.693627607904,468.628519370473));
#50008=CARTESIAN_POINT('Ctrl Pts',(304.516986927068,-68.4779934089828,467.889812007953));
#50009=CARTESIAN_POINT('Ctrl Pts',(304.735736195578,-69.0941315197382,467.510571937363));
#50010=CARTESIAN_POINT('Ctrl Pts',(304.815841535928,-69.3716532420849,467.370670606613));
#50011=CARTESIAN_POINT('Ctrl Pts',(304.36560734514,-69.4720072829635,472.883816394761));
#50012=CARTESIAN_POINT('Ctrl Pts',(304.437924386038,-69.4720061785358,472.755478620527));
#50013=CARTESIAN_POINT('Ctrl Pts',(304.578280640235,-69.4970261445459,472.495428198348));
#50014=CARTESIAN_POINT('Ctrl Pts',(304.771191553278,-69.6083606205034,472.107646255653));
#50015=CARTESIAN_POINT('Ctrl Pts',(304.942919591518,-69.7913397669247,471.732484512733));
#50016=CARTESIAN_POINT('Ctrl Pts',(305.091118069088,-70.0432002703421,471.381409217703));
#50017=CARTESIAN_POINT('Ctrl Pts',(305.213936884918,-70.3602758159736,471.067167469123));
#50018=CARTESIAN_POINT('Ctrl Pts',(305.277815958598,-70.609423919947,470.892937814703));
#50019=CARTESIAN_POINT('Ctrl Pts',(305.305042216108,-70.742010890829,470.816601123963));
#50020=CARTESIAN_POINT('Origin',(317.464909153118,-72.0120072687901,483.416551570203));
#50021=CARTESIAN_POINT('Origin',(314.575917770968,-72.0120072687901,481.093605606543));
#50022=CARTESIAN_POINT('Origin',(314.575917770968,-72.0120072687901,481.093605606543));
#50023=CARTESIAN_POINT('Origin',(314.575917770968,-72.0120072687901,481.093605606543));
#50024=CARTESIAN_POINT('Origin',(314.575917770968,-72.01200726879,402.251606455353));
#50025=CARTESIAN_POINT('Origin',(263.115917770968,-69.47200726879,445.000000551893));
#50026=CARTESIAN_POINT('Origin',(306.683384790848,-69.47200726879,420.897720214303));
#50027=CARTESIAN_POINT('Origin',(306.683384790848,-69.47200726879,420.897720214303));
#50028=CARTESIAN_POINT('Origin',(306.683384790848,-69.47200726879,420.897720214303));
#50029=CARTESIAN_POINT('Origin',(208.951764595088,-69.47200726879,499.480603520313));
#50030=CARTESIAN_POINT('Origin',(263.115917770968,-69.47200726879,445.000000551893));
#50031=CARTESIAN_POINT('Origin',(239.013637433378,-69.4720072687899,401.432533532013));
#50032=CARTESIAN_POINT('Ctrl Pts',(235.028190410038,-69.46544846321,486.364643478553));
#50033=CARTESIAN_POINT('Ctrl Pts',(235.058784398358,-69.4642529784631,486.382245155523));
#50034=CARTESIAN_POINT('Ctrl Pts',(235.258976493428,-69.461131317104,486.496332464443));
#50035=CARTESIAN_POINT('Ctrl Pts',(235.636888941828,-69.5121743079281,486.698315147843));
#50036=CARTESIAN_POINT('Ctrl Pts',(236.146870785568,-69.711509521041,486.942061181483));
#50037=CARTESIAN_POINT('Ctrl Pts',(236.619881789448,-70.0335847626079,487.144032803713));
#50038=CARTESIAN_POINT('Ctrl Pts',(236.985786004388,-70.4242464530176,487.284367991343));
#50039=CARTESIAN_POINT('Ctrl Pts',(237.167315497998,-70.713413234505,487.348935251613));
#50040=CARTESIAN_POINT('Ctrl Pts',(237.233421929898,-70.840779768824,487.371932164383));
#50041=CARTESIAN_POINT('Ctrl Pts',(235.977522050648,-69.6040686220959,484.982557637913));
#50042=CARTESIAN_POINT('Ctrl Pts',(236.004671893388,-69.6012555491032,484.997624146153));
#50043=CARTESIAN_POINT('Ctrl Pts',(236.182698522748,-69.5867035136386,485.095456441663));
#50044=CARTESIAN_POINT('Ctrl Pts',(236.524196098828,-69.605895880883,485.271347646443));
#50045=CARTESIAN_POINT('Ctrl Pts',(237.006005570248,-69.7468138148857,485.495488520553));
#50046=CARTESIAN_POINT('Ctrl Pts',(237.478127991128,-70.0122251216762,485.696827627373));
#50047=CARTESIAN_POINT('Ctrl Pts',(237.865067852528,-70.3697189200575,485.850830120423));
#50048=CARTESIAN_POINT('Ctrl Pts',(238.065383438968,-70.653842506004,485.927482824733));
#50049=CARTESIAN_POINT('Ctrl Pts',(238.139279526348,-70.781931585494,485.955407815003));
#50050=CARTESIAN_POINT('Ctrl Pts',(236.610590348658,-68.419135189814,483.969751425023));
#50051=CARTESIAN_POINT('Ctrl Pts',(236.648879211058,-68.41446975451,483.993940563573));
#50052=CARTESIAN_POINT('Ctrl Pts',(236.899811351788,-68.389529900869,484.151505778333));
#50053=CARTESIAN_POINT('Ctrl Pts',(237.379808367058,-68.410079767087,484.441021758033));
#50054=CARTESIAN_POINT('Ctrl Pts',(238.057492885838,-68.6071111008896,484.824821137953));
#50055=CARTESIAN_POINT('Ctrl Pts',(238.724680693938,-68.9922445608702,485.183064252343));
#50056=CARTESIAN_POINT('Ctrl Pts',(239.275210865108,-69.5223481989856,485.466301413533));
#50057=CARTESIAN_POINT('Ctrl Pts',(239.561823319288,-69.9492631288263,485.610200564473));
#50058=CARTESIAN_POINT('Ctrl Pts',(239.667741277698,-70.1425137073577,485.662926108393));
#50059=CARTESIAN_POINT('Ctrl Pts',(236.482739132008,-66.742924819268,484.037602324843));
#50060=CARTESIAN_POINT('Ctrl Pts',(236.538926325478,-66.737473314687,484.076164315743));
#50061=CARTESIAN_POINT('Ctrl Pts',(236.906627390308,-66.710484421782,484.327495017863));
#50062=CARTESIAN_POINT('Ctrl Pts',(237.602758556818,-66.764646425836,484.790543958523));
#50063=CARTESIAN_POINT('Ctrl Pts',(238.562786312978,-67.092908761381,485.401124149403));
#50064=CARTESIAN_POINT('Ctrl Pts',(239.483982940058,-67.690059702463,485.963601145843));
#50065=CARTESIAN_POINT('Ctrl Pts',(240.225755093378,-68.4773127599914,486.400868152653));
#50066=CARTESIAN_POINT('Ctrl Pts',(240.605561769818,-69.094559414416,486.619942017203));
#50067=CARTESIAN_POINT('Ctrl Pts',(240.745242209038,-69.3716421412076,486.699921112973));
#50068=CARTESIAN_POINT('',(237.299356354755,-70.7420814892879,487.189107554724));
#50069=CARTESIAN_POINT('Ctrl Pts',(235.232102033643,-69.4720072796082,486.249690185527));
#50070=CARTESIAN_POINT('Ctrl Pts',(235.3592580076,-69.4720058497161,486.321341955001));
#50071=CARTESIAN_POINT('Ctrl Pts',(235.488356422264,-69.4843168520743,486.391048411963));
#50072=CARTESIAN_POINT('Ctrl Pts',(235.658418468521,-69.5166114182826,486.479309551096));
#50073=CARTESIAN_POINT('Ctrl Pts',(235.699575114172,-69.5256727717999,486.500398420692));
#50074=CARTESIAN_POINT('Ctrl Pts',(235.828178647505,-69.5579244915859,486.565443702623));
#50075=CARTESIAN_POINT('Ctrl Pts',(235.915403941424,-69.5855055087001,486.608325495863));
#50076=CARTESIAN_POINT('Ctrl Pts',(236.082685935217,-69.6496600928298,486.688345395098));
#50077=CARTESIAN_POINT('Ctrl Pts',(236.162832376958,-69.6855216028279,486.725675808643));
#50078=CARTESIAN_POINT('Ctrl Pts',(236.28711143786,-69.7495837444741,486.782105481196));
#50079=CARTESIAN_POINT('Ctrl Pts',(236.33206025476,-69.7745536342549,486.802204687413));
#50080=CARTESIAN_POINT('Ctrl Pts',(236.492448571889,-69.8703147051983,486.872903627949));
#50081=CARTESIAN_POINT('Ctrl Pts',(236.604898071057,-69.9501642898247,486.92049203298));
#50082=CARTESIAN_POINT('Ctrl Pts',(236.717004498143,-70.0443954690103,486.966335815599));
#50083=CARTESIAN_POINT('Ctrl Pts',(236.722327705171,-70.0489065580006,486.968508642302));
#50084=CARTESIAN_POINT('Ctrl Pts',(236.839139822294,-70.1487082562837,487.016102550549));
#50085=CARTESIAN_POINT('Ctrl Pts',(236.944250966748,-70.2548440769946,487.057176136868));
#50086=CARTESIAN_POINT('Ctrl Pts',(237.066131244566,-70.4011757050274,487.103468011324));
#50087=CARTESIAN_POINT('Ctrl Pts',(237.091327483615,-70.4328767762969,487.11295359292));
#50088=CARTESIAN_POINT('Ctrl Pts',(237.182331506607,-70.5529932331032,487.146934631606));
#50089=CARTESIAN_POINT('Ctrl Pts',(237.243714297159,-70.6454659295432,487.169284956413));
#50090=CARTESIAN_POINT('Ctrl Pts',(237.299306537109,-70.7420200540544,487.189112906131));
#50091=CARTESIAN_POINT('Origin',(239.013668569868,-69.4721721185271,488.567490430283));
#50092=CARTESIAN_POINT('Origin',(235.232099195168,-66.932007290493,486.249688566713));
#50093=CARTESIAN_POINT('Origin',(224.680024455158,-72.01200726879,499.373047478893));
#50094=CARTESIAN_POINT('',(228.736601009321,-70.7420092778759,497.838377092546));
#50095=CARTESIAN_POINT('Origin',(227.022312716318,-72.01200726879,496.460000551893));
#50096=CARTESIAN_POINT('',(228.736612414338,-70.742007149697,497.838360865333));
#50097=CARTESIAN_POINT('Origin',(229.003814201928,-69.47200726879,501.016441204783));
#50098=CARTESIAN_POINT('Origin',(239.013637433378,-69.47200726879,488.567467571773));
#50099=CARTESIAN_POINT('Ctrl Pts',(232.667503020318,-72.01200726879,496.460000551893));
#50100=CARTESIAN_POINT('Ctrl Pts',(232.552467855573,-72.0120072687895,496.50034510223));
#50101=CARTESIAN_POINT('Ctrl Pts',(232.439630484044,-72.0095636111055,496.539900696401));
#50102=CARTESIAN_POINT('Ctrl Pts',(232.32901983994,-72.0049345804185,496.578681378017));
#50103=CARTESIAN_POINT('Ctrl Pts',(232.214621370972,-72.0001470301093,496.618790091227));
#50104=CARTESIAN_POINT('Ctrl Pts',(232.102604351893,-71.9930221141204,496.658069591567));
#50105=CARTESIAN_POINT('Ctrl Pts',(231.992972675035,-71.9838027053761,496.6965128071));
#50106=CARTESIAN_POINT('Ctrl Pts',(231.94065912929,-71.9794034297751,496.714856966124));
#50107=CARTESIAN_POINT('Ctrl Pts',(231.888888351699,-71.9745266060022,496.733010412023));
#50108=CARTESIAN_POINT('Ctrl Pts',(231.83765902232,-71.9691951485491,496.750970975055));
#50109=CARTESIAN_POINT('Ctrl Pts',(231.719354046327,-71.9568831008675,496.792447683885));
#50110=CARTESIAN_POINT('Ctrl Pts',(231.603941821324,-71.9421444368137,496.83289995809));
#50111=CARTESIAN_POINT('Ctrl Pts',(231.491767776884,-71.9253093502902,496.872233052362));
#50112=CARTESIAN_POINT('Ctrl Pts',(231.377934231753,-71.9082252058153,496.912148039687));
#50113=CARTESIAN_POINT('Ctrl Pts',(231.267435458371,-71.8889826584263,496.950910545216));
#50114=CARTESIAN_POINT('Ctrl Pts',(231.160592692157,-71.8679429935163,496.988389592098));
#50115=CARTESIAN_POINT('Ctrl Pts',(231.139204181572,-71.8637311304995,496.995892402249));
#50116=CARTESIAN_POINT('Ctrl Pts',(231.117962057352,-71.8594472855261,497.003343675825));
#50117=CARTESIAN_POINT('Ctrl Pts',(231.096868706623,-71.8550944057315,497.010742209328));
#50118=CARTESIAN_POINT('Ctrl Pts',(230.994786588947,-71.834028469214,497.046547709236));
#50119=CARTESIAN_POINT('Ctrl Pts',(230.896191382266,-71.8113504463176,497.081119958007));
#50120=CARTESIAN_POINT('Ctrl Pts',(230.800915719752,-71.7872977520841,497.114529086895));
#50121=CARTESIAN_POINT('Ctrl Pts',(230.702607866525,-71.7624795700636,497.149001476302));
#50122=CARTESIAN_POINT('Ctrl Pts',(230.607833795941,-71.7361978239251,497.182235199856));
#50123=CARTESIAN_POINT('Ctrl Pts',(230.516397501224,-71.7086604136538,497.214297533498));
#50124=CARTESIAN_POINT('Ctrl Pts',(230.496534912513,-71.7026784974344,497.221262393002));
#50125=CARTESIAN_POINT('Ctrl Pts',(230.476829796947,-71.6966371365143,497.228171951769));
#50126=CARTESIAN_POINT('Ctrl Pts',(230.457280101594,-71.6905381477013,497.235026864256));
#50127=CARTESIAN_POINT('Ctrl Pts',(230.366315753107,-71.6621596725492,497.266922637414));
#50128=CARTESIAN_POINT('Ctrl Pts',(230.278721835742,-71.6325417447297,497.297639767496));
#50129=CARTESIAN_POINT('Ctrl Pts',(230.194254442441,-71.6018271779252,497.327260296549));
#50130=CARTESIAN_POINT('Ctrl Pts',(230.107506337049,-71.5702832841915,497.357680612315));
#50131=CARTESIAN_POINT('Ctrl Pts',(230.024055457235,-71.5375825442999,497.386943973369));
#50132=CARTESIAN_POINT('Ctrl Pts',(229.943641520358,-71.5038254269623,497.415142400406));
#50133=CARTESIAN_POINT('Ctrl Pts',(229.932984397381,-71.4993516533258,497.418879490223));
#50134=CARTESIAN_POINT('Ctrl Pts',(229.922380625256,-71.4948592522483,497.422597884436));
#50135=CARTESIAN_POINT('Ctrl Pts',(229.911829609023,-71.4903483914863,497.426297806007));
#50136=CARTESIAN_POINT('Ctrl Pts',(229.824112674067,-71.4528468967154,497.457057476225));
#50137=CARTESIAN_POINT('Ctrl Pts',(229.740045190858,-71.4140777953039,497.486542947253));
#50138=CARTESIAN_POINT('Ctrl Pts',(229.659402575902,-71.3741434343248,497.514821730231));
#50139=CARTESIAN_POINT('Ctrl Pts',(229.585884356645,-71.337737086292,497.540602215752));
#50140=CARTESIAN_POINT('Ctrl Pts',(229.515212470564,-71.3003613442696,497.565379706035));
#50141=CARTESIAN_POINT('Ctrl Pts',(229.447226075572,-71.2620580055471,497.5892128494));
#50142=CARTESIAN_POINT('Ctrl Pts',(229.354619849438,-71.209883925015,497.621676660199));
#50143=CARTESIAN_POINT('Ctrl Pts',(229.267002875685,-71.1559856710929,497.652393646307));
#50144=CARTESIAN_POINT('Ctrl Pts',(229.184502681344,-71.1007413457377,497.681324771646));
#50145=CARTESIAN_POINT('Ctrl Pts',(229.139999322598,-71.0709407125436,497.696931186396));
#50146=CARTESIAN_POINT('Ctrl Pts',(229.096984178731,-71.0407484336903,497.712017366799));
#50147=CARTESIAN_POINT('Ctrl Pts',(229.055472371791,-71.0102237227464,497.726573248913));
#50148=CARTESIAN_POINT('Ctrl Pts',(228.974165797026,-70.9504368843627,497.755082943012));
#50149=CARTESIAN_POINT('Ctrl Pts',(228.898627668183,-70.8893746621778,497.781559283438));
#50150=CARTESIAN_POINT('Ctrl Pts',(228.82879483944,-70.8274387196506,497.806041823638));
#50151=CARTESIAN_POINT('Ctrl Pts',(228.796879010488,-70.7991320194465,497.817231124993));
#50152=CARTESIAN_POINT('Ctrl Pts',(228.766154363183,-70.7706425598328,497.828003538254));
#50153=CARTESIAN_POINT('Ctrl Pts',(228.736612293562,-70.7420072391727,497.838360768221));
#50154=CARTESIAN_POINT('Origin',(239.013637433378,-69.47200726879,488.567467571773));
#50155=CARTESIAN_POINT('Ctrl Pts',(232.828215541778,-74.713507444107,498.994794772563));
#50156=CARTESIAN_POINT('Ctrl Pts',(232.708581879358,-74.744487732072,498.992935002363));
#50157=CARTESIAN_POINT('Ctrl Pts',(232.135343545468,-74.879297233076,498.981813429663));
#50158=CARTESIAN_POINT('Ctrl Pts',(231.115092555868,-75.007840422924,498.944324337233));
#50159=CARTESIAN_POINT('Ctrl Pts',(229.794873524148,-74.948821572214,498.864713031993));
#50160=CARTESIAN_POINT('Ctrl Pts',(228.602549223458,-74.694184459517,498.770637037043));
#50161=CARTESIAN_POINT('Ctrl Pts',(227.544153995848,-74.277385902565,498.671516955493));
#50162=CARTESIAN_POINT('Ctrl Pts',(226.618188533358,-73.717781829921,498.573974289063));
#50163=CARTESIAN_POINT('Ctrl Pts',(226.002925806248,-73.179135190463,498.503623109783));
#50164=CARTESIAN_POINT('Ctrl Pts',(225.700915179718,-72.841170440473,498.467827978703));
#50165=CARTESIAN_POINT('Ctrl Pts',(225.638265364858,-72.767200936835,498.460354730143));
#50166=CARTESIAN_POINT('Ctrl Pts',(232.796568792498,-73.034824311939,499.102763601033));
#50167=CARTESIAN_POINT('Ctrl Pts',(232.700627839608,-73.066583901593,499.119930810033));
#50168=CARTESIAN_POINT('Ctrl Pts',(232.239472322888,-73.209004644328,499.198942363853));
#50169=CARTESIAN_POINT('Ctrl Pts',(231.407183411038,-73.381806588117,499.313593076103));
#50170=CARTESIAN_POINT('Ctrl Pts',(230.309431538318,-73.435351583061,499.415978913903));
#50171=CARTESIAN_POINT('Ctrl Pts',(229.301912439328,-73.326904152345,499.474828842763));
#50172=CARTESIAN_POINT('Ctrl Pts',(228.394849201738,-73.078553798327,499.502527799073));
#50173=CARTESIAN_POINT('Ctrl Pts',(227.591135930828,-72.703469484999,499.508897708423));
#50174=CARTESIAN_POINT('Ctrl Pts',(227.050979790138,-72.31828963445,499.503395046963));
#50175=CARTESIAN_POINT('Ctrl Pts',(226.784203935658,-72.069395060257,499.498324453983));
#50176=CARTESIAN_POINT('Ctrl Pts',(226.728793427818,-72.014632724146,499.497177704013));
#50177=CARTESIAN_POINT('Ctrl Pts',(232.774487437958,-71.863532363329,497.895184339653));
#50178=CARTESIAN_POINT('Ctrl Pts',(232.694803909168,-71.881299175708,497.925633863583));
#50179=CARTESIAN_POINT('Ctrl Pts',(232.313470385268,-71.960042879053,498.068730506413));
#50180=CARTESIAN_POINT('Ctrl Pts',(231.638597324018,-72.047682887232,498.300987160673));
#50181=CARTESIAN_POINT('Ctrl Pts',(230.772193181568,-72.052539058419,498.561581886413));
#50182=CARTESIAN_POINT('Ctrl Pts',(229.995069126148,-71.958291489615,498.767069706243));
#50183=CARTESIAN_POINT('Ctrl Pts',(229.309457180988,-71.779984113588,498.927010515113));
#50184=CARTESIAN_POINT('Ctrl Pts',(228.712998830268,-71.526452518351,499.049965226743));
#50185=CARTESIAN_POINT('Ctrl Pts',(228.318711996458,-71.274222914498,499.121996638453));
#50186=CARTESIAN_POINT('Ctrl Pts',(228.125712481478,-71.113515579462,499.154902555743));
#50187=CARTESIAN_POINT('Ctrl Pts',(228.085699392628,-71.078244434764,499.161627305873));
#50188=CARTESIAN_POINT('Ctrl Pts',(232.777480917018,-72.022320298527,496.220233067973));
#50189=CARTESIAN_POINT('Ctrl Pts',(232.695200683688,-72.021150461685,496.248891048053));
#50190=CARTESIAN_POINT('Ctrl Pts',(232.305363184468,-72.009654141941,496.385012840253));
#50191=CARTESIAN_POINT('Ctrl Pts',(231.646794450228,-71.942527322552,496.617737847513));
#50192=CARTESIAN_POINT('Ctrl Pts',(230.858125249948,-71.771639917819,496.901630898333));
#50193=CARTESIAN_POINT('Ctrl Pts',(230.195161865978,-71.549628732325,497.144473472413));
#50194=CARTESIAN_POINT('Ctrl Pts',(229.645578188088,-71.293762522114,497.349195293073));
#50195=CARTESIAN_POINT('Ctrl Pts',(229.195806366078,-71.013440752079,497.519520532373));
#50196=CARTESIAN_POINT('Ctrl Pts',(228.915696291618,-70.780263637391,497.627313411293));
#50197=CARTESIAN_POINT('Ctrl Pts',(228.783195868548,-70.644919903199,497.678773977973));
#50198=CARTESIAN_POINT('Ctrl Pts',(228.755923515418,-70.615733806332,497.689386467923));
#50199=CARTESIAN_POINT('',(227.022399636625,-72.0120079573874,499.000000348522));
#50200=CARTESIAN_POINT('Ctrl Pts',(227.022421081461,-72.012007957416,498.999999476569));
#50201=CARTESIAN_POINT('Ctrl Pts',(227.06847075155,-71.9753249175649,498.99999748761));
#50202=CARTESIAN_POINT('Ctrl Pts',(227.115340764603,-71.9392458075247,498.997948376115));
#50203=CARTESIAN_POINT('Ctrl Pts',(227.162630111902,-71.9036114492896,498.993805945675));
#50204=CARTESIAN_POINT('Ctrl Pts',(227.209596090345,-71.8682207620356,498.98969184155));
#50205=CARTESIAN_POINT('Ctrl Pts',(227.256975528797,-71.8332687556922,498.98351291858));
#50206=CARTESIAN_POINT('Ctrl Pts',(227.304397150955,-71.7986331412776,498.975255910314));
#50207=CARTESIAN_POINT('Ctrl Pts',(227.351770822992,-71.7640325484796,498.967007251077));
#50208=CARTESIAN_POINT('Ctrl Pts',(227.399186400484,-71.7297478280298,498.956684688518));
#50209=CARTESIAN_POINT('Ctrl Pts',(227.446297999784,-71.6956899506178,498.944307449555));
#50210=CARTESIAN_POINT('Ctrl Pts',(227.472117142457,-71.6770247978935,498.937524200771));
#50211=CARTESIAN_POINT('Ctrl Pts',(227.497845427324,-71.6584283466738,498.930124401024));
#50212=CARTESIAN_POINT('Ctrl Pts',(227.523429338898,-71.6398898461305,498.922115354748));
#50213=CARTESIAN_POINT('Ctrl Pts',(227.590792656308,-71.591077337818,498.90102726097));
#50214=CARTESIAN_POINT('Ctrl Pts',(227.657109208906,-71.5425836661277,498.875709755667));
#50215=CARTESIAN_POINT('Ctrl Pts',(227.722096104895,-71.4947553753147,498.846285134344));
#50216=CARTESIAN_POINT('Ctrl Pts',(227.785827643853,-71.4478509873942,498.817428910768));
#50217=CARTESIAN_POINT('Ctrl Pts',(227.848280221467,-71.4015866110791,498.78462266685));
#50218=CARTESIAN_POINT('Ctrl Pts',(227.909184067879,-71.3562721759498,498.748028637086));
#50219=CARTESIAN_POINT('Ctrl Pts',(227.939258824668,-71.3338955824197,498.729958242358));
#50220=CARTESIAN_POINT('Ctrl Pts',(227.968955899638,-71.311750357558,498.710964945372));
#50221=CARTESIAN_POINT('Ctrl Pts',(227.998242796831,-71.2898721306231,498.691072691413));
#50222=CARTESIAN_POINT('Ctrl Pts',(228.052793616142,-71.2491209647857,498.654020669675));
#50223=CARTESIAN_POINT('Ctrl Pts',(228.105914342892,-71.2092859907835,498.613847313292));
#50224=CARTESIAN_POINT('Ctrl Pts',(228.157479914924,-71.1706830835565,498.570728131421));
#50225=CARTESIAN_POINT('Ctrl Pts',(228.209797989254,-71.1315168396836,498.526979706391));
#50226=CARTESIAN_POINT('Ctrl Pts',(228.260514665963,-71.0936188702463,498.480198730004));
#50227=CARTESIAN_POINT('Ctrl Pts',(228.309488531813,-71.0572796433875,498.430603837579));
#50228=CARTESIAN_POINT('Ctrl Pts',(228.344151906793,-71.0315589814536,498.395500904138));
#50229=CARTESIAN_POINT('Ctrl Pts',(228.377941919378,-71.0066183661931,498.358989036));
#50230=CARTESIAN_POINT('Ctrl Pts',(228.410807708469,-70.9825493079025,498.321156509064));
#50231=CARTESIAN_POINT('Ctrl Pts',(228.447983219353,-70.9553240513908,498.278362967336));
#50232=CARTESIAN_POINT('Ctrl Pts',(228.484003351377,-70.9292507855684,498.233878481141));
#50233=CARTESIAN_POINT('Ctrl Pts',(228.518585800815,-70.9041908400226,498.18786433216));
#50234=CARTESIAN_POINT('Ctrl Pts',(228.553946879116,-70.8785666661695,498.140814167944));
#50235=CARTESIAN_POINT('Ctrl Pts',(228.587804799258,-70.8540025583241,498.092164553924));
#50236=CARTESIAN_POINT('Ctrl Pts',(228.619897788445,-70.8303782654369,498.042113731418));
#50237=CARTESIAN_POINT('Ctrl Pts',(228.652889562856,-70.8060923587233,497.990661202781));
#50238=CARTESIAN_POINT('Ctrl Pts',(228.684016033206,-70.7828005038813,497.93772782412));
#50239=CARTESIAN_POINT('Ctrl Pts',(228.713035766474,-70.7603900681321,497.883557523744));
#50240=CARTESIAN_POINT('Ctrl Pts',(228.721054130665,-70.7541979011036,497.868589874222));
#50241=CARTESIAN_POINT('Ctrl Pts',(228.728911908006,-70.7480730855502,497.853527956442));
#50242=CARTESIAN_POINT('Ctrl Pts',(228.736604586192,-70.7420133331698,497.838377286705));
#50243=CARTESIAN_POINT('',(232.667503019844,-74.5520072687783,499.00000447072));
#50244=CARTESIAN_POINT('Ctrl Pts',(232.667503019828,-74.552007268779,499.000004766233));
#50245=CARTESIAN_POINT('Ctrl Pts',(232.248833705458,-74.551992484692,498.999983408163));
#50246=CARTESIAN_POINT('Ctrl Pts',(231.455510492608,-74.490207324118,499.000008510273));
#50247=CARTESIAN_POINT('Ctrl Pts',(230.386046693498,-74.254566710358,498.999998413173));
#50248=CARTESIAN_POINT('Ctrl Pts',(229.470698714398,-73.920471430072,499.000001148393));
#50249=CARTESIAN_POINT('Ctrl Pts',(228.690942526618,-73.517848718933,499.000000304633));
#50250=CARTESIAN_POINT('Ctrl Pts',(228.025995010608,-73.060368306828,499.000000944453));
#50251=CARTESIAN_POINT('Ctrl Pts',(227.462209463058,-72.553339670543,498.999999228903));
#50252=CARTESIAN_POINT('Ctrl Pts',(227.158361801518,-72.195521218722,499.000003377153));
#50253=CARTESIAN_POINT('Ctrl Pts',(227.022421081468,-72.012007957393,499.000000073513));
#50254=CARTESIAN_POINT('Origin',(232.667503019858,-74.552013924409,496.460000551893));
#50255=CARTESIAN_POINT('Origin',(305.864311867508,-74.5520072687901,496.460000551893));
#50256=CARTESIAN_POINT('',(293.56433252188,-74.5520072687791,499.000004766103));
#50257=CARTESIAN_POINT('',(293.564332522018,-74.5520072687791,499.000004766103));
#50258=CARTESIAN_POINT('Origin',(293.564332521738,-74.5520072687901,496.460000551893));
#50259=CARTESIAN_POINT('Origin',(220.615917770968,-69.47200726879,499.000000551893));
#50260=CARTESIAN_POINT('Ctrl Pts',(299.209414458968,-72.0120079557911,499.000000073343));
#50261=CARTESIAN_POINT('Ctrl Pts',(299.073473744338,-72.1955212182401,499.000003378503));
#50262=CARTESIAN_POINT('Ctrl Pts',(298.769626079658,-72.5533396718461,498.999999228283));
#50263=CARTESIAN_POINT('Ctrl Pts',(298.205840530728,-73.0603683052571,499.000000944623));
#50264=CARTESIAN_POINT('Ctrl Pts',(297.540893016148,-73.5178487195051,499.000000304583));
#50265=CARTESIAN_POINT('Ctrl Pts',(296.761136827618,-73.9204714296421,499.000001148393));
#50266=CARTESIAN_POINT('Ctrl Pts',(295.845788848668,-74.2545667103361,498.999998413213));
#50267=CARTESIAN_POINT('Ctrl Pts',(294.776325049528,-74.4902073240851,499.000008510113));
#50268=CARTESIAN_POINT('Ctrl Pts',(293.983001836448,-74.5519924854471,498.999983408503));
#50269=CARTESIAN_POINT('Ctrl Pts',(293.564332522018,-74.5520072687791,499.000004766103));
#50270=CARTESIAN_POINT('',(220.615917755701,-72.0120072687902,499.000000551894));
#50271=CARTESIAN_POINT('',(227.022421081468,-72.012007957393,499.000000073513));
#50272=CARTESIAN_POINT('',(220.615917770968,-85.47200726879,499.000000551893));
#50273=CARTESIAN_POINT('Origin',(220.615917770968,-69.47200726879,487.500000551893));
#50274=CARTESIAN_POINT('',(209.115917770968,-72.01200726879,487.500000551203));
#50275=CARTESIAN_POINT('Origin',(220.615917770968,-72.01200726879,487.500000551893));
#50276=CARTESIAN_POINT('',(209.115917770968,-85.47200726879,487.500000551893));
#50277=CARTESIAN_POINT('Origin',(220.615917770968,-72.01200726879,487.500000551893));
#50278=CARTESIAN_POINT('Origin',(220.615917745948,-72.01200726879,496.460000551893));
#50279=CARTESIAN_POINT('Origin',(211.655917770968,-72.01200726879,487.500000551893));
#50280=CARTESIAN_POINT('Origin',(211.655917770968,-72.01200726879,487.748394648433));
#50281=CARTESIAN_POINT('',(209.115918153386,-72.0120048639453,481.093519010876));
#50282=CARTESIAN_POINT('Origin',(211.655917770968,-72.01200726879,481.093605606543));
#50283=CARTESIAN_POINT('',(209.115917770968,-72.01200726879,487.500000551203));
#50284=CARTESIAN_POINT('Origin',(209.115917770968,-69.4720072687899,402.500000551893));
#50285=CARTESIAN_POINT('',(209.115913556758,-74.552007268779,475.448415302943));
#50286=CARTESIAN_POINT('Ctrl Pts',(209.115918249518,-72.012007955791,481.093497239893));
#50287=CARTESIAN_POINT('Ctrl Pts',(209.115914944358,-72.19552121824,480.957556525263));
#50288=CARTESIAN_POINT('Ctrl Pts',(209.115919094578,-72.553339671846,480.653708860583));
#50289=CARTESIAN_POINT('Ctrl Pts',(209.115917378238,-73.060368305257,480.089923311653));
#50290=CARTESIAN_POINT('Ctrl Pts',(209.115918018278,-73.517848719505,479.424975797073));
#50291=CARTESIAN_POINT('Ctrl Pts',(209.115917174468,-73.920471429642,478.645219608543));
#50292=CARTESIAN_POINT('Ctrl Pts',(209.115919909648,-74.254566710336,477.729871629593));
#50293=CARTESIAN_POINT('Ctrl Pts',(209.115909812748,-74.490207324085,476.660407830453));
#50294=CARTESIAN_POINT('Ctrl Pts',(209.115934914358,-74.551992485447,475.867084617373));
#50295=CARTESIAN_POINT('Ctrl Pts',(209.115913556758,-74.552007268779,475.448415302943));
#50296=CARTESIAN_POINT('',(209.115913852141,-74.5520072687782,414.551585800769));
#50297=CARTESIAN_POINT('',(209.115913556758,-74.552007268779,475.448415302943));
#50298=CARTESIAN_POINT('',(209.115918153252,-72.0120048645283,408.90648209161));
#50299=CARTESIAN_POINT('Ctrl Pts',(209.115913556628,-74.5520072687789,414.551585800753));
#50300=CARTESIAN_POINT('Ctrl Pts',(209.115934914698,-74.5519924846919,414.132916486383));
#50301=CARTESIAN_POINT('Ctrl Pts',(209.115909812588,-74.4902073241179,413.339593273533));
#50302=CARTESIAN_POINT('Ctrl Pts',(209.115919909688,-74.2545667103599,412.270129474423));
#50303=CARTESIAN_POINT('Ctrl Pts',(209.115917174468,-73.9204714300629,411.354781495313));
#50304=CARTESIAN_POINT('Ctrl Pts',(209.115918018228,-73.5178487189669,410.575025307573));
#50305=CARTESIAN_POINT('Ctrl Pts',(209.115917378408,-73.0603683067019,409.910077791393));
#50306=CARTESIAN_POINT('Ctrl Pts',(209.115919093958,-72.5533396710129,409.346292244473));
#50307=CARTESIAN_POINT('Ctrl Pts',(209.115914945708,-72.1955212177089,409.042444581383));
#50308=CARTESIAN_POINT('Ctrl Pts',(209.115918249348,-72.0120079562219,408.906503861543));
#50309=CARTESIAN_POINT('',(209.115918249348,-72.0120079562219,408.906503861543));
#50310=CARTESIAN_POINT('Origin',(211.655917770968,-72.01200726879,487.748394648433));
#50311=CARTESIAN_POINT('Origin',(211.655917770968,-72.0120072687899,408.906395497243));
#50312=CARTESIAN_POINT('Origin',(211.655917770968,-72.0120072687899,408.906395497243));
#50313=CARTESIAN_POINT('',(210.277543223595,-70.7420027758393,410.620680576218));
#50314=CARTESIAN_POINT('Origin',(211.655917770968,-72.0120072687899,408.906395497243));
#50315=CARTESIAN_POINT('Origin',(211.655917770968,-72.0119940563109,408.906387830743));
#50316=CARTESIAN_POINT('Origin',(208.730420887858,-72.0120072687899,406.554096622863));
#50317=CARTESIAN_POINT('',(220.926808850179,-70.742084448958,419.183439558327));
#50318=CARTESIAN_POINT('Ctrl Pts',(221.866228196796,-69.4720072829634,417.116184709025));
#50319=CARTESIAN_POINT('Ctrl Pts',(221.793911155898,-69.4720061785357,417.244522483259));
#50320=CARTESIAN_POINT('Ctrl Pts',(221.653554901702,-69.4970261445458,417.504572905438));
#50321=CARTESIAN_POINT('Ctrl Pts',(221.460643988658,-69.6083606205033,417.892354848133));
#50322=CARTESIAN_POINT('Ctrl Pts',(221.288915950418,-69.7913397669245,418.267516591053));
#50323=CARTESIAN_POINT('Ctrl Pts',(221.140717472848,-70.0432002703419,418.618591886083));
#50324=CARTESIAN_POINT('Ctrl Pts',(221.017898657018,-70.3602758159734,418.932833634663));
#50325=CARTESIAN_POINT('Ctrl Pts',(220.954019583338,-70.6094239199469,419.107063289083));
#50326=CARTESIAN_POINT('Ctrl Pts',(220.926793325828,-70.7420108908289,419.183399979823));
#50327=CARTESIAN_POINT('',(210.277557457508,-70.7420071496399,410.620695195203));
#50328=CARTESIAN_POINT('Ctrl Pts',(221.751276938898,-69.4654490974855,416.912272239873));
#50329=CARTESIAN_POINT('Ctrl Pts',(221.733129877708,-69.4642164587727,416.943814007983));
#50330=CARTESIAN_POINT('Ctrl Pts',(221.617992489818,-69.4612105224025,417.145906513633));
#50331=CARTESIAN_POINT('Ctrl Pts',(221.415156312278,-69.5133172277359,417.525769829863));
#50332=CARTESIAN_POINT('Ctrl Pts',(221.172069855068,-69.7138478877061,418.035004402343));
#50333=CARTESIAN_POINT('Ctrl Pts',(220.971244208648,-70.0353627268993,418.505648542643));
#50334=CARTESIAN_POINT('Ctrl Pts',(220.831492939438,-70.4245592719199,418.870035530053));
#50335=CARTESIAN_POINT('Ctrl Pts',(220.767019322678,-70.7132164602069,419.051296804093));
#50336=CARTESIAN_POINT('Ctrl Pts',(220.743986066728,-70.8407847846869,419.117507753173));
#50337=CARTESIAN_POINT('Ctrl Pts',(223.133361772338,-69.6040686792587,417.861603377653));
#50338=CARTESIAN_POINT('Ctrl Pts',(223.117828522468,-69.6011683474858,417.889594372033));
#50339=CARTESIAN_POINT('Ctrl Pts',(223.019091236198,-69.5865972268537,418.069323269803));
#50340=CARTESIAN_POINT('Ctrl Pts',(222.842402306488,-69.6065541544154,418.412681535193));
#50341=CARTESIAN_POINT('Ctrl Pts',(222.618697713768,-69.748647110422,418.894056406763));
#50342=CARTESIAN_POINT('Ctrl Pts',(222.418383540508,-70.0138432058709,419.363994557133));
#50343=CARTESIAN_POINT('Ctrl Pts',(222.265017884668,-70.3700332044191,419.749336964243));
#50344=CARTESIAN_POINT('Ctrl Pts',(222.188478557108,-70.653644403435,419.949352944663));
#50345=CARTESIAN_POINT('Ctrl Pts',(222.160509530328,-70.7819364497499,420.023365919093));
#50346=CARTESIAN_POINT('Ctrl Pts',(224.146167652288,-68.4191356321779,418.494670406743));
#50347=CARTESIAN_POINT('Ctrl Pts',(224.121229218938,-68.4143254993869,418.534145567303));
#50348=CARTESIAN_POINT('Ctrl Pts',(223.962191433298,-68.389321427153,418.787473307343));
#50349=CARTESIAN_POINT('Ctrl Pts',(223.671268120298,-68.4109449839659,419.270074399333));
#50350=CARTESIAN_POINT('Ctrl Pts',(223.288048525248,-68.6097419631932,419.947170649143));
#50351=CARTESIAN_POINT('Ctrl Pts',(222.931550755408,-68.9946417969064,420.611300967703));
#50352=CARTESIAN_POINT('Ctrl Pts',(222.649483805568,-69.5228226663634,421.159560115753));
#50353=CARTESIAN_POINT('Ctrl Pts',(222.505798556868,-69.9489645106603,421.445743086943));
#50354=CARTESIAN_POINT('Ctrl Pts',(222.452989851008,-70.142521288732,421.551828578973));
#50355=CARTESIAN_POINT('Ctrl Pts',(224.078317577708,-66.7429260460049,418.366818202673));
#50356=CARTESIAN_POINT('Ctrl Pts',(224.038561001198,-66.7373054148149,418.424746193413));
#50357=CARTESIAN_POINT('Ctrl Pts',(223.784876123258,-66.7103285449819,418.795940696103));
#50358=CARTESIAN_POINT('Ctrl Pts',(223.319573013478,-66.7662645270549,419.495730784653));
#50359=CARTESIAN_POINT('Ctrl Pts',(222.709982075748,-67.0970793500919,420.454658245053));
#50360=CARTESIAN_POINT('Ctrl Pts',(222.150306245338,-67.6936276079039,421.371481733313));
#50361=CARTESIAN_POINT('Ctrl Pts',(221.714848614868,-68.4779934089825,422.110189095833));
#50362=CARTESIAN_POINT('Ctrl Pts',(221.496099346358,-69.0941315197381,422.489429166423));
#50363=CARTESIAN_POINT('Ctrl Pts',(221.415994006008,-69.3716532420848,422.629330497173));
#50364=CARTESIAN_POINT('Origin',(219.548426388038,-69.4721780198135,420.897754057183));
#50365=CARTESIAN_POINT('Origin',(221.866229658128,-66.9320073823689,417.116182155053));
#50366=CARTESIAN_POINT('Origin',(263.115917770968,-66.93200726879,445.000000551893));
#50367=CARTESIAN_POINT('Origin',(235.232099333908,-66.9320072687899,403.750312439503));
#50368=CARTESIAN_POINT('Ctrl Pts',(237.233549882728,-70.8410255423379,402.628024620243));
#50369=CARTESIAN_POINT('Ctrl Pts',(237.166974214408,-70.7127222484639,402.651184041943));
#50370=CARTESIAN_POINT('Ctrl Pts',(236.984869388708,-70.4229586079244,402.715961802783));
#50371=CARTESIAN_POINT('Ctrl Pts',(236.618402976028,-70.0324228883722,402.856575913253));
#50372=CARTESIAN_POINT('Ctrl Pts',(236.146471696558,-69.711449747235,403.058146362133));
#50373=CARTESIAN_POINT('Ctrl Pts',(235.638095324218,-69.512638144513,403.301110138693));
#50374=CARTESIAN_POINT('Ctrl Pts',(235.260489121208,-69.4612407849914,403.502837229903));
#50375=CARTESIAN_POINT('Ctrl Pts',(235.059875954418,-69.4642146335529,403.617129368273));
#50376=CARTESIAN_POINT('Ctrl Pts',(235.028428642488,-69.4654396674749,403.635221145173));
#50377=CARTESIAN_POINT('Ctrl Pts',(238.139422700518,-70.7821785594619,404.044539750673));
#50378=CARTESIAN_POINT('Ctrl Pts',(238.065000599578,-70.6531438863329,404.072662858133));
#50379=CARTESIAN_POINT('Ctrl Pts',(237.864062326518,-70.3684786785249,404.149556582403));
#50380=CARTESIAN_POINT('Ctrl Pts',(237.476623171508,-70.0112367740756,404.303798588993));
#50381=CARTESIAN_POINT('Ctrl Pts',(237.005646976138,-69.7468008290302,404.504691162843));
#50382=CARTESIAN_POINT('Ctrl Pts',(236.525331980678,-69.6062166524363,404.728125988013));
#50383=CARTESIAN_POINT('Ctrl Pts',(236.184054767208,-69.5867023581791,404.903827170923));
#50384=CARTESIAN_POINT('Ctrl Pts',(236.005640525168,-69.6011587121201,405.001840027323));
#50385=CARTESIAN_POINT('Ctrl Pts',(235.977733092948,-69.6040471487245,405.017326135553));
#50386=CARTESIAN_POINT('Ctrl Pts',(239.667946446748,-70.1428862842576,404.336973689953));
#50387=CARTESIAN_POINT('Ctrl Pts',(239.561274231638,-69.9482081499974,404.390073749173));
#50388=CARTESIAN_POINT('Ctrl Pts',(239.273773460878,-69.5204913988231,404.534422144333));
#50389=CARTESIAN_POINT('Ctrl Pts',(238.722549836198,-68.9908005466803,404.818062860253));
#50390=CARTESIAN_POINT('Ctrl Pts',(238.056991236348,-68.6071038509312,405.175476844673));
#50391=CARTESIAN_POINT('Ctrl Pts',(237.381404445628,-68.4105256300779,405.558075870093));
#50392=CARTESIAN_POINT('Ctrl Pts',(236.901719399648,-68.3894990752359,405.847325697563));
#50393=CARTESIAN_POINT('Ctrl Pts',(236.650244885598,-68.4143084253989,406.005197780233));
#50394=CARTESIAN_POINT('Ctrl Pts',(236.610887702388,-68.4190995018019,406.030060962223));
#50395=CARTESIAN_POINT('Ctrl Pts',(240.745512611478,-69.3721764983919,403.299925922353));
#50396=CARTESIAN_POINT('Ctrl Pts',(240.604838520268,-69.0930496471821,403.380472822573));
#50397=CARTESIAN_POINT('Ctrl Pts',(240.223846195178,-68.4746082940245,403.600235607753));
#50398=CARTESIAN_POINT('Ctrl Pts',(239.481065738028,-67.6878508746749,404.038158442043));
#50399=CARTESIAN_POINT('Ctrl Pts',(238.562058543708,-67.0928621596819,404.599355204583));
#50400=CARTESIAN_POINT('Ctrl Pts',(237.605022300298,-66.7653976675589,405.208017414293));
#50401=CARTESIAN_POINT('Ctrl Pts',(236.909407855438,-66.7105257118319,405.670635844973));
#50402=CARTESIAN_POINT('Ctrl Pts',(236.540930137708,-66.7372867844729,405.922461582133));
#50403=CARTESIAN_POINT('Ctrl Pts',(236.483175678898,-66.7428833566679,405.962098286683));
#50404=CARTESIAN_POINT('',(237.299337446915,-70.7420402776057,402.810888231475));
#50405=CARTESIAN_POINT('Origin',(239.013670773968,-69.4721762071727,401.432509576753));
#50406=CARTESIAN_POINT('Ctrl Pts',(237.299306020227,-70.7420200455038,402.810887527682));
#50407=CARTESIAN_POINT('Ctrl Pts',(237.243212043783,-70.6445951393941,402.830894421642));
#50408=CARTESIAN_POINT('Ctrl Pts',(237.181240654867,-70.5513567221656,402.853463025695));
#50409=CARTESIAN_POINT('Ctrl Pts',(237.089965079941,-70.4311536188862,402.887559389488));
#50410=CARTESIAN_POINT('Ctrl Pts',(237.065170544958,-70.4000028232924,402.896896373708));
#50411=CARTESIAN_POINT('Ctrl Pts',(236.943547013715,-70.2540727483776,402.943096611271));
#50412=CARTESIAN_POINT('Ctrl Pts',(236.838285008499,-70.147886017895,402.984237043943));
#50413=CARTESIAN_POINT('Ctrl Pts',(236.721167126839,-70.047920025344,403.031965775962));
#50414=CARTESIAN_POINT('Ctrl Pts',(236.715633996361,-70.0432370796357,403.034224934696));
#50415=CARTESIAN_POINT('Ctrl Pts',(236.603413091615,-69.9490612742504,403.080131984757));
#50416=CARTESIAN_POINT('Ctrl Pts',(236.491135927334,-69.8694544987991,403.12766427235));
#50417=CARTESIAN_POINT('Ctrl Pts',(236.331150141304,-69.7740400952014,403.198202289507));
#50418=CARTESIAN_POINT('Ctrl Pts',(236.286358613182,-69.7491804686927,403.21823503636));
#50419=CARTESIAN_POINT('Ctrl Pts',(236.16218220769,-69.6852131557635,403.274625319477));
#50420=CARTESIAN_POINT('Ctrl Pts',(236.081996177396,-69.6493657107355,403.311979884422));
#50421=CARTESIAN_POINT('Ctrl Pts',(235.915390721252,-69.5855318937611,403.391686852879));
#50422=CARTESIAN_POINT('Ctrl Pts',(235.828898456121,-69.5581670824827,403.434204879921));
#50423=CARTESIAN_POINT('Ctrl Pts',(235.700509048139,-69.5258783396488,403.499122783802));
#50424=CARTESIAN_POINT('Ctrl Pts',(235.658852883162,-69.5166925224,403.520464743105));
#50425=CARTESIAN_POINT('Ctrl Pts',(235.488419035691,-69.4843334129535,403.608922427488));
#50426=CARTESIAN_POINT('Ctrl Pts',(235.359324546871,-69.4720048208222,403.678623129688));
#50427=CARTESIAN_POINT('Ctrl Pts',(235.23210195903,-69.4720073298541,403.75031096033));
#50428=CARTESIAN_POINT('Origin',(312.119295247928,-72.0120072687901,499.373047478893));
#50429=CARTESIAN_POINT('',(228.736597916929,-70.7420026857022,392.161625909054));
#50430=CARTESIAN_POINT('',(237.299318413618,-70.7420108634959,402.810877563033));
#50431=CARTESIAN_POINT('Origin',(227.022312716318,-72.0120072687899,393.540000551893));
#50432=CARTESIAN_POINT('Origin',(227.022312716318,-72.0120072687899,393.540000551893));
#50433=CARTESIAN_POINT('Origin',(227.022305049898,-72.0119940551319,393.540000551893));
#50434=CARTESIAN_POINT('Ctrl Pts',(225.638731539658,-72.7677512569999,391.539590768683));
#50435=CARTESIAN_POINT('Ctrl Pts',(225.701233575478,-72.8415267130749,391.532135400383));
#50436=CARTESIAN_POINT('Ctrl Pts',(226.003100564118,-73.1792881921419,391.496357986363));
#50437=CARTESIAN_POINT('Ctrl Pts',(226.618188529078,-73.7177818201399,391.426026824253));
#50438=CARTESIAN_POINT('Ctrl Pts',(227.544153998748,-74.2773859034239,391.328484143693));
#50439=CARTESIAN_POINT('Ctrl Pts',(228.602549223918,-74.6941844569289,391.229364067463));
#50440=CARTESIAN_POINT('Ctrl Pts',(229.794873524898,-74.9488215698489,391.135288067703));
#50441=CARTESIAN_POINT('Ctrl Pts',(231.115092556868,-75.0078404229169,391.055676779643));
#50442=CARTESIAN_POINT('Ctrl Pts',(232.135101469358,-74.8793277233339,391.018196529693));
#50443=CARTESIAN_POINT('Ctrl Pts',(232.708118783838,-74.7445966300439,391.007075109083));
#50444=CARTESIAN_POINT('Ctrl Pts',(232.827528105778,-74.7136854275459,391.005217023583));
#50445=CARTESIAN_POINT('Ctrl Pts',(226.729205733288,-72.0150401412129,390.502814873693));
#50446=CARTESIAN_POINT('Ctrl Pts',(226.784485182628,-72.0696574342109,390.501671320983));
#50447=CARTESIAN_POINT('Ctrl Pts',(227.051133216628,-72.3183990485599,390.496604468393));
#50448=CARTESIAN_POINT('Ctrl Pts',(227.591135925408,-72.7034694767339,390.491103408133));
#50449=CARTESIAN_POINT('Ctrl Pts',(228.394849203928,-73.0785538001049,390.497473302493));
#50450=CARTESIAN_POINT('Ctrl Pts',(229.301912439038,-73.3269041512489,390.525172264273));
#50451=CARTESIAN_POINT('Ctrl Pts',(230.309431538478,-73.4353515823529,390.584022187893));
#50452=CARTESIAN_POINT('Ctrl Pts',(231.407183411688,-73.3818065903929,390.686408043543));
#50453=CARTESIAN_POINT('Ctrl Pts',(232.239274844198,-73.2090456373969,390.801031497173));
#50454=CARTESIAN_POINT('Ctrl Pts',(232.700255290318,-73.0666989540409,390.880006490083));
#50455=CARTESIAN_POINT('Ctrl Pts',(232.796017495648,-73.0350067849759,390.897138866913));
#50456=CARTESIAN_POINT('Ctrl Pts',(228.085997126648,-71.0785068454429,390.838423841053));
#50457=CARTESIAN_POINT('Ctrl Pts',(228.125915950258,-71.1136849925869,390.845133249633));
#50458=CARTESIAN_POINT('Ctrl Pts',(228.318823985898,-71.2742945628339,390.878024909003));
#50459=CARTESIAN_POINT('Ctrl Pts',(228.712998825878,-71.5264525149989,390.950035883993));
#50460=CARTESIAN_POINT('Ctrl Pts',(229.309457181038,-71.7799841162819,391.072990587163));
#50461=CARTESIAN_POINT('Ctrl Pts',(229.995069125098,-71.9582914907429,391.232931398903));
#50462=CARTESIAN_POINT('Ctrl Pts',(230.772193181038,-72.0525390598589,391.438419215633));
#50463=CARTESIAN_POINT('Ctrl Pts',(231.638597324058,-72.0476828902759,391.699013951043));
#50464=CARTESIAN_POINT('Ctrl Pts',(232.313310257318,-71.9600636709789,391.931215466993));
#50465=CARTESIAN_POINT('Ctrl Pts',(232.694495845898,-71.8813627885119,392.074251652513));
#50466=CARTESIAN_POINT('Ctrl Pts',(232.774029563598,-71.8636344410639,392.104641802563));
#50467=CARTESIAN_POINT('Ctrl Pts',(228.756126450238,-70.6159509551309,392.310693601373));
#50468=CARTESIAN_POINT('Ctrl Pts',(228.783335561338,-70.6450625854709,392.321281376383));
#50469=CARTESIAN_POINT('Ctrl Pts',(228.915775844658,-70.7803298660319,392.372718306873));
#50470=CARTESIAN_POINT('Ctrl Pts',(229.195806365828,-71.0134407518539,392.480480568223));
#50471=CARTESIAN_POINT('Ctrl Pts',(229.645578187428,-71.2937625231659,392.650805808573));
#50472=CARTESIAN_POINT('Ctrl Pts',(230.195161865718,-71.5496287328339,392.855527628773));
#50473=CARTESIAN_POINT('Ctrl Pts',(230.858125249808,-71.7716399183579,393.098370203183));
#50474=CARTESIAN_POINT('Ctrl Pts',(231.646794450178,-71.9425273223459,393.382263252623));
#50475=CARTESIAN_POINT('Ctrl Pts',(232.305206926388,-72.0096382157559,393.614933045543));
#50476=CARTESIAN_POINT('Ctrl Pts',(232.694885752718,-72.0211411690119,393.751000084983));
#50477=CARTESIAN_POINT('Ctrl Pts',(232.777008130648,-72.0223135621609,393.779603362203));
#50478=CARTESIAN_POINT('Ctrl Pts',(228.736612778339,-70.7420068809478,392.161639950096));
#50479=CARTESIAN_POINT('Ctrl Pts',(228.74403795138,-70.7492044424187,392.164243359666));
#50480=CARTESIAN_POINT('Ctrl Pts',(228.751537755498,-70.7563928376238,392.166872853459));
#50481=CARTESIAN_POINT('Ctrl Pts',(228.759112290133,-70.763571339069,392.169528479623));
#50482=CARTESIAN_POINT('Ctrl Pts',(228.809211693663,-70.8110513042359,392.187093292937));
#50483=CARTESIAN_POINT('Ctrl Pts',(228.862583719871,-70.8580999963968,392.205802451487));
#50484=CARTESIAN_POINT('Ctrl Pts',(228.919273539135,-70.9045511124965,392.225676018046));
#50485=CARTESIAN_POINT('Ctrl Pts',(228.962724221884,-70.9401542019974,392.240908383343));
#50486=CARTESIAN_POINT('Ctrl Pts',(229.008123316606,-70.9754058614114,392.256824573291));
#50487=CARTESIAN_POINT('Ctrl Pts',(229.055472831776,-71.0102232739626,392.273427482023));
#50488=CARTESIAN_POINT('Ctrl Pts',(229.080041424926,-71.0282892423348,392.282042356078));
#50489=CARTESIAN_POINT('Ctrl Pts',(229.105137428495,-71.0462403635194,392.29084252611));
#50490=CARTESIAN_POINT('Ctrl Pts',(229.130755854209,-71.0640622097133,392.299825985934));
#50491=CARTESIAN_POINT('Ctrl Pts',(229.193064119902,-71.1074078992641,392.321675252076));
#50492=CARTESIAN_POINT('Ctrl Pts',(229.258465836879,-71.14998880754,392.344609885107));
#50493=CARTESIAN_POINT('Ctrl Pts',(229.326918348435,-71.1916308944421,392.368610806374));
#50494=CARTESIAN_POINT('Ctrl Pts',(229.36603060828,-71.2154242671967,392.382324405011));
#50495=CARTESIAN_POINT('Ctrl Pts',(229.40613801284,-71.2389111258167,392.396385806151));
#50496=CARTESIAN_POINT('Ctrl Pts',(229.447225366973,-71.2620589077046,392.410788824469));
#50497=CARTESIAN_POINT('Ctrl Pts',(229.494799950007,-71.288861462766,392.427465916615));
#50498=CARTESIAN_POINT('Ctrl Pts',(229.543696252613,-71.3152111239886,392.444609773287));
#50499=CARTESIAN_POINT('Ctrl Pts',(229.59395706903,-71.3410926562254,392.462233906472));
#50500=CARTESIAN_POINT('Ctrl Pts',(229.670815547899,-71.38067050912,392.489184604145));
#50501=CARTESIAN_POINT('Ctrl Pts',(229.750864959679,-71.4191559802305,392.517258475578));
#50502=CARTESIAN_POINT('Ctrl Pts',(229.834329102691,-71.4564687983865,392.54652792326));
#50503=CARTESIAN_POINT('Ctrl Pts',(229.859841020467,-71.4678739541152,392.555474516559));
#50504=CARTESIAN_POINT('Ctrl Pts',(229.885671907711,-71.4791691936545,392.564532782266));
#50505=CARTESIAN_POINT('Ctrl Pts',(229.911827890448,-71.4903512773118,392.573704679131));
#50506=CARTESIAN_POINT('Ctrl Pts',(229.988742853775,-71.5232336034354,392.600675797678));
#50507=CARTESIAN_POINT('Ctrl Pts',(230.068471344098,-71.5551392419008,392.628634979833));
#50508=CARTESIAN_POINT('Ctrl Pts',(230.151226023293,-71.5859845480201,392.657655092177));
#50509=CARTESIAN_POINT('Ctrl Pts',(230.234662022126,-71.6170838036803,392.686914127233));
#50510=CARTESIAN_POINT('Ctrl Pts',(230.321173870445,-71.6471054203405,392.717251501234));
#50511=CARTESIAN_POINT('Ctrl Pts',(230.411024902909,-71.6759139021873,392.748757605007));
#50512=CARTESIAN_POINT('Ctrl Pts',(230.426345128825,-71.6808259486944,392.754129614814));
#50513=CARTESIAN_POINT('Ctrl Pts',(230.441762397531,-71.6857026097513,392.75953558958));
#50514=CARTESIAN_POINT('Ctrl Pts',(230.457277962987,-71.6905430691913,392.76497595883));
#50515=CARTESIAN_POINT('Ctrl Pts',(230.545245222552,-71.7179866034395,392.79582074984));
#50516=CARTESIAN_POINT('Ctrl Pts',(230.63636403198,-71.7442659054211,392.827769177735));
#50517=CARTESIAN_POINT('Ctrl Pts',(230.730813923741,-71.7691988042511,392.860887773716));
#50518=CARTESIAN_POINT('Ctrl Pts',(230.760044347557,-71.7769150566064,392.871137341806));
#50519=CARTESIAN_POINT('Ctrl Pts',(230.789593588474,-71.7845020756735,392.881498908917));
#50520=CARTESIAN_POINT('Ctrl Pts',(230.819466283583,-71.7919537134946,392.891974213097));
#50521=CARTESIAN_POINT('Ctrl Pts',(230.908976721051,-71.8142817745812,392.923362377314));
#50522=CARTESIAN_POINT('Ctrl Pts',(231.001392860546,-71.8353967743901,392.955772267799));
#50523=CARTESIAN_POINT('Ctrl Pts',(231.096866864063,-71.8551008150376,392.989260375604));
#50524=CARTESIAN_POINT('Ctrl Pts',(231.190683495745,-71.8744628052754,393.022167149802));
#50525=CARTESIAN_POINT('Ctrl Pts',(231.287442455986,-71.8924577821863,393.056101914368));
#50526=CARTESIAN_POINT('Ctrl Pts',(231.386931110687,-71.9088265655427,393.090990503202));
#50527=CARTESIAN_POINT('Ctrl Pts',(231.461377080757,-71.9210750973928,393.117097146698));
#50528=CARTESIAN_POINT('Ctrl Pts',(231.537350586221,-71.9324134528414,393.143737550279));
#50529=CARTESIAN_POINT('Ctrl Pts',(231.61474610887,-71.9427410029754,393.170874910618));
#50530=CARTESIAN_POINT('Ctrl Pts',(231.687812320525,-71.9524908559145,393.196494275234));
#50531=CARTESIAN_POINT('Ctrl Pts',(231.762145631757,-71.9613399669065,393.222556457012));
#50532=CARTESIAN_POINT('Ctrl Pts',(231.837658155136,-71.9692011295691,393.249030825801));
#50533=CARTESIAN_POINT('Ctrl Pts',(231.948168690718,-71.9807057285055,393.287775348473));
#50534=CARTESIAN_POINT('Ctrl Pts',(232.061196287319,-71.9900966506596,393.327401492746));
#50535=CARTESIAN_POINT('Ctrl Pts',(232.176755960482,-71.9971271824967,393.367917803244));
#50536=CARTESIAN_POINT('Ctrl Pts',(232.292315633645,-72.0041577143338,393.408434113742));
#50537=CARTESIAN_POINT('Ctrl Pts',(232.410407981347,-72.0088279534613,393.449840809688));
#50538=CARTESIAN_POINT('Ctrl Pts',(232.531007414461,-72.0108586572646,393.492132222973));
#50539=CARTESIAN_POINT('Ctrl Pts',(232.576155932945,-72.0116188869426,393.507964757215));
#50540=CARTESIAN_POINT('Ctrl Pts',(232.621655364709,-72.0120088644348,393.523921124644));
#50541=CARTESIAN_POINT('Ctrl Pts',(232.667503020154,-72.0120105964114,393.540000551869));
#50542=CARTESIAN_POINT('Origin',(232.667503020198,-74.5520072687899,393.540000551893));
#50543=CARTESIAN_POINT('Origin',(220.367523674428,-74.5520072687899,393.540000551893));
#50544=CARTESIAN_POINT('Origin',(317.572435894888,-69.4720072687901,499.134199992603));
#50545=CARTESIAN_POINT('Origin',(239.013637433378,-69.4720072687899,401.432533532013));
#50546=CARTESIAN_POINT('Origin',(239.013637433378,-69.4720072687899,401.432533532013));
#50547=CARTESIAN_POINT('Origin',(219.548450751088,-69.47200726879,420.897720214303));
#50548=CARTESIAN_POINT('Origin',(219.548450751088,-69.47200726879,420.897720214303));
#50549=CARTESIAN_POINT('Origin',(219.548450751088,-69.47200726879,420.897720214303));
#50550=CARTESIAN_POINT('Origin',(207.104559699488,-69.4720072687899,410.891983724703));
#50551=CARTESIAN_POINT('Ctrl Pts',(211.655917770968,-72.0120072687899,414.551585801243));
#50552=CARTESIAN_POINT('Ctrl Pts',(211.615573220631,-72.0120072687893,414.436550636498));
#50553=CARTESIAN_POINT('Ctrl Pts',(211.57601762646,-72.0095636111052,414.323713264967));
#50554=CARTESIAN_POINT('Ctrl Pts',(211.537236944843,-72.004934580418,414.213102620862));
#50555=CARTESIAN_POINT('Ctrl Pts',(211.497128231632,-72.0001470301086,414.098704151893));
#50556=CARTESIAN_POINT('Ctrl Pts',(211.457848731293,-71.9930221141195,413.986687132813));
#50557=CARTESIAN_POINT('Ctrl Pts',(211.41940551576,-71.9838027053749,413.877055455955));
#50558=CARTESIAN_POINT('Ctrl Pts',(211.401061356736,-71.979403429774,413.824741910211));
#50559=CARTESIAN_POINT('Ctrl Pts',(211.382907910837,-71.9745266060013,413.772971132622));
#50560=CARTESIAN_POINT('Ctrl Pts',(211.364947347806,-71.9691951485483,413.721741803245));
#50561=CARTESIAN_POINT('Ctrl Pts',(211.323470638976,-71.9568831008668,413.603436827254));
#50562=CARTESIAN_POINT('Ctrl Pts',(211.283018364773,-71.9421444368132,413.488024602253));
#50563=CARTESIAN_POINT('Ctrl Pts',(211.2436852705,-71.9253093502899,413.375850557814));
#50564=CARTESIAN_POINT('Ctrl Pts',(211.203770283176,-71.9082252058153,413.262017012686));
#50565=CARTESIAN_POINT('Ctrl Pts',(211.165007777648,-71.8889826584265,413.151518239305));
#50566=CARTESIAN_POINT('Ctrl Pts',(211.127528730766,-71.8679429935169,413.044675473092));
#50567=CARTESIAN_POINT('Ctrl Pts',(211.120025920614,-71.8637311304994,413.023286962504));
#50568=CARTESIAN_POINT('Ctrl Pts',(211.112574647037,-71.8594472855253,413.002044838281));
#50569=CARTESIAN_POINT('Ctrl Pts',(211.105176113533,-71.8550944057301,412.980951487548));
#50570=CARTESIAN_POINT('Ctrl Pts',(211.069370613624,-71.8340284692115,412.878869369868));
#50571=CARTESIAN_POINT('Ctrl Pts',(211.034798364851,-71.811350446314,412.780274163183));
#50572=CARTESIAN_POINT('Ctrl Pts',(211.001389235961,-71.7872977520792,412.684998500664));
#50573=CARTESIAN_POINT('Ctrl Pts',(210.966916846553,-71.7624795700572,412.586690647433));
#50574=CARTESIAN_POINT('Ctrl Pts',(210.933683122997,-71.7361978239172,412.491916576845));
#50575=CARTESIAN_POINT('Ctrl Pts',(210.901620789353,-71.7086604136442,412.400480282124));
#50576=CARTESIAN_POINT('Ctrl Pts',(210.894655929852,-71.7026784974274,412.380617693421));
#50577=CARTESIAN_POINT('Ctrl Pts',(210.887746371089,-71.6966371365098,412.360912577864));
#50578=CARTESIAN_POINT('Ctrl Pts',(210.880891458605,-71.6905381476994,412.34136288252));
#50579=CARTESIAN_POINT('Ctrl Pts',(210.848995685452,-71.6621596725513,412.250398534045));
#50580=CARTESIAN_POINT('Ctrl Pts',(210.818278555373,-71.6325417447364,412.162804616693));
#50581=CARTESIAN_POINT('Ctrl Pts',(210.788658026324,-71.6018271779366,412.078337223404));
#50582=CARTESIAN_POINT('Ctrl Pts',(210.758237710562,-71.5702832842081,411.991589118024));
#50583=CARTESIAN_POINT('Ctrl Pts',(210.728974349512,-71.5375825443219,411.908138238221));
#50584=CARTESIAN_POINT('Ctrl Pts',(210.700775922478,-71.5038254269898,411.827724301354));
#50585=CARTESIAN_POINT('Ctrl Pts',(210.697038832652,-71.4993516533435,411.817067178353));
#50586=CARTESIAN_POINT('Ctrl Pts',(210.693320438431,-71.494859252256,411.806463406203));
#50587=CARTESIAN_POINT('Ctrl Pts',(210.689620516852,-71.490348391484,411.795912389948));
#50588=CARTESIAN_POINT('Ctrl Pts',(210.658860846593,-71.4528468966634,411.708195454875));
#50589=CARTESIAN_POINT('Ctrl Pts',(210.629375375526,-71.4140777951987,411.624127971558));
#50590=CARTESIAN_POINT('Ctrl Pts',(210.601096592513,-71.3741434341638,411.543485356505));
#50591=CARTESIAN_POINT('Ctrl Pts',(210.575316107032,-71.3377370861809,411.469967137362));
#50592=CARTESIAN_POINT('Ctrl Pts',(210.550538616785,-71.3003613442115,411.399295251388));
#50593=CARTESIAN_POINT('Ctrl Pts',(210.526705473455,-71.2620580055459,411.331308856496));
#50594=CARTESIAN_POINT('Ctrl Pts',(210.494241662258,-71.2098839243747,411.238702629227));
#50595=CARTESIAN_POINT('Ctrl Pts',(210.463524675797,-71.1559856697735,411.151085654466));
#50596=CARTESIAN_POINT('Ctrl Pts',(210.434593550148,-71.1007413437056,411.068585459237));
#50597=CARTESIAN_POINT('Ctrl Pts',(210.418987135777,-71.0709407111722,411.024082101572));
#50598=CARTESIAN_POINT('Ctrl Pts',(210.403900955729,-71.0407484329972,410.981066958717));
#50599=CARTESIAN_POINT('Ctrl Pts',(210.389345073945,-71.0102237227438,410.939555152717));
#50600=CARTESIAN_POINT('Ctrl Pts',(210.360835380456,-70.9504368856354,410.858248579687));
#50601=CARTESIAN_POINT('Ctrl Pts',(210.334359040546,-70.8893746647691,410.782710452317));
#50602=CARTESIAN_POINT('Ctrl Pts',(210.309876500781,-70.8274387235966,410.712877624817));
#50603=CARTESIAN_POINT('Ctrl Pts',(210.298687198858,-70.7991320220723,410.680961794248));
#50604=CARTESIAN_POINT('Ctrl Pts',(210.28791478507,-70.7706425611211,410.650237145439));
#50605=CARTESIAN_POINT('Ctrl Pts',(210.277557554618,-70.7420072391133,410.62069507443));
#50606=CARTESIAN_POINT('Ctrl Pts',(209.121123721488,-74.7135102960079,414.712287298723));
#50607=CARTESIAN_POINT('Ctrl Pts',(209.122983464708,-74.7444894757819,414.592657233853));
#50608=CARTESIAN_POINT('Ctrl Pts',(209.134105034848,-74.8792977192369,414.019422444493));
#50609=CARTESIAN_POINT('Ctrl Pts',(209.171593985388,-75.0078404201239,412.999175337183));
#50610=CARTESIAN_POINT('Ctrl Pts',(209.251205289358,-74.9488215699039,411.678956306283));
#50611=CARTESIAN_POINT('Ctrl Pts',(209.345281286278,-74.6941844563889,410.486632004503));
#50612=CARTESIAN_POINT('Ctrl Pts',(209.444401360718,-74.2773859031249,409.428236781593));
#50613=CARTESIAN_POINT('Ctrl Pts',(209.541944049408,-73.7177818197019,408.502271304853));
#50614=CARTESIAN_POINT('Ctrl Pts',(209.612256946988,-73.1794278704339,407.887342904063));
#50615=CARTESIAN_POINT('Ctrl Pts',(209.648018171018,-72.8418519885089,407.585607074523));
#50616=CARTESIAN_POINT('Ctrl Pts',(209.655457208818,-72.7682536630759,407.523240000553));
#50617=CARTESIAN_POINT('Ctrl Pts',(209.013153141798,-73.0348272383849,414.680642732713));
#50618=CARTESIAN_POINT('Ctrl Pts',(208.995986491448,-73.0665857466229,414.584704646173));
#50619=CARTESIAN_POINT('Ctrl Pts',(208.916975523978,-73.2090053014829,414.123551936943));
#50620=CARTESIAN_POINT('Ctrl Pts',(208.802325249018,-73.3818065876669,413.291266191913));
#50621=CARTESIAN_POINT('Ctrl Pts',(208.699939410138,-73.4353515827459,412.193514319793));
#50622=CARTESIAN_POINT('Ctrl Pts',(208.641089483568,-73.3269041507879,411.185995219493));
#50623=CARTESIAN_POINT('Ctrl Pts',(208.613390519918,-73.0785538002929,410.278931986753));
#50624=CARTESIAN_POINT('Ctrl Pts',(208.607020634118,-72.7034694752909,409.475218700813));
#50625=CARTESIAN_POINT('Ctrl Pts',(208.612520244838,-72.3184989335639,408.935356080983));
#50626=CARTESIAN_POINT('Ctrl Pts',(208.617583669858,-72.0698969776509,408.668824761813));
#50627=CARTESIAN_POINT('Ctrl Pts',(208.618724302488,-72.0154120774029,408.613665002433));
#50628=CARTESIAN_POINT('Ctrl Pts',(210.220731177198,-71.8635340023709,414.658562876293));
#50629=CARTESIAN_POINT('Ctrl Pts',(210.190282605478,-71.8813001977719,414.578881749843));
#50630=CARTESIAN_POINT('Ctrl Pts',(210.047186932298,-71.9600432143439,414.197550598173));
#50631=CARTESIAN_POINT('Ctrl Pts',(209.814931162538,-72.0476828890719,413.522680104543));
#50632=CARTESIAN_POINT('Ctrl Pts',(209.554336436448,-72.0525390603359,412.656275962093));
#50633=CARTESIAN_POINT('Ctrl Pts',(209.348848618108,-71.9582914907669,411.879151905633));
#50634=CARTESIAN_POINT('Ctrl Pts',(209.188907805368,-71.7799841165459,411.193539962853));
#50635=CARTESIAN_POINT('Ctrl Pts',(209.065953106938,-71.5264525146379,410.597081603543));
#50636=CARTESIAN_POINT('Ctrl Pts',(208.993960798188,-71.2743599704639,410.203009018083));
#50637=CARTESIAN_POINT('Ctrl Pts',(208.961082152008,-71.1138396640759,410.010184514773));
#50638=CARTESIAN_POINT('Ctrl Pts',(208.954386755368,-71.0787464051469,409.970351781083));
#50639=CARTESIAN_POINT('Ctrl Pts',(211.895682611298,-72.0223201904569,414.661556116033));
#50640=CARTESIAN_POINT('Ctrl Pts',(211.867025508458,-72.0211503125039,414.579278414173));
#50641=CARTESIAN_POINT('Ctrl Pts',(211.730904594288,-72.0096538864489,414.189443459553));
#50642=CARTESIAN_POINT('Ctrl Pts',(211.498180472458,-71.9425273227339,413.530877231143));
#50643=CARTESIAN_POINT('Ctrl Pts',(211.214287421758,-71.7716399182749,412.742208030703));
#50644=CARTESIAN_POINT('Ctrl Pts',(210.971444847568,-71.5496287330819,412.079244646653));
#50645=CARTESIAN_POINT('Ctrl Pts',(210.766723027528,-71.2937625227309,411.529660968183));
#50646=CARTESIAN_POINT('Ctrl Pts',(210.596397786528,-71.0134407536249,411.079889147063));
#50647=CARTESIAN_POINT('Ctrl Pts',(210.488663479068,-70.7803903280709,410.799931260843));
#50648=CARTESIAN_POINT('Ctrl Pts',(210.437248133258,-70.6451928569439,410.667545895773));
#50649=CARTESIAN_POINT('Ctrl Pts',(210.426682931138,-70.6161492097429,410.640394546293));
#50650=CARTESIAN_POINT('Origin',(211.655917770968,-74.5520139244089,414.551585800783));
#50651=CARTESIAN_POINT('Origin',(211.655917770968,-74.55200726879,487.748394648433));
#50652=CARTESIAN_POINT('Origin',(211.655917770968,-74.55200726879,475.448415302663));
#50653=CARTESIAN_POINT('Ctrl Pts',(209.655507987758,-72.767751257,482.477186783203));
#50654=CARTESIAN_POINT('Ctrl Pts',(209.648052619458,-72.841526713075,482.414684747383));
#50655=CARTESIAN_POINT('Ctrl Pts',(209.612275205438,-73.179288192142,482.112817758743));
#50656=CARTESIAN_POINT('Ctrl Pts',(209.541944043328,-73.71778182014,481.497729793783));
#50657=CARTESIAN_POINT('Ctrl Pts',(209.444401362768,-74.277385903423,480.571764324113));
#50658=CARTESIAN_POINT('Ctrl Pts',(209.345281286538,-74.694184456929,479.513369098943));
#50659=CARTESIAN_POINT('Ctrl Pts',(209.251205286778,-74.948821569849,478.321044797963));
#50660=CARTESIAN_POINT('Ctrl Pts',(209.171593998718,-75.007840422917,477.000825765993));
#50661=CARTESIAN_POINT('Ctrl Pts',(209.134113748768,-74.879327723334,475.980816853503));
#50662=CARTESIAN_POINT('Ctrl Pts',(209.122992328158,-74.744596630044,475.407799539023));
#50663=CARTESIAN_POINT('Ctrl Pts',(209.121134242658,-74.713685427546,475.288390217083));
#50664=CARTESIAN_POINT('Ctrl Pts',(208.618732092768,-72.015040141213,481.386712589573));
#50665=CARTESIAN_POINT('Ctrl Pts',(208.617588540058,-72.069657434211,481.331433140233));
#50666=CARTESIAN_POINT('Ctrl Pts',(208.612521687468,-72.31839904856,481.064785106233));
#50667=CARTESIAN_POINT('Ctrl Pts',(208.607020627208,-72.703469476734,480.524782397453));
#50668=CARTESIAN_POINT('Ctrl Pts',(208.613390521568,-73.078553800105,479.721069118933));
#50669=CARTESIAN_POINT('Ctrl Pts',(208.641089483348,-73.326904151249,478.814005883823));
#50670=CARTESIAN_POINT('Ctrl Pts',(208.699939406968,-73.435351582353,477.806486784383));
#50671=CARTESIAN_POINT('Ctrl Pts',(208.802325262618,-73.381806590393,476.708734911173));
#50672=CARTESIAN_POINT('Ctrl Pts',(208.916948716248,-73.209045637397,475.876643478663));
#50673=CARTESIAN_POINT('Ctrl Pts',(208.995923709158,-73.066698954042,475.415663032543));
#50674=CARTESIAN_POINT('Ctrl Pts',(209.013056085988,-73.035006784976,475.319900827213));
#50675=CARTESIAN_POINT('Ctrl Pts',(208.954341060128,-71.078506845443,480.029921196213));
#50676=CARTESIAN_POINT('Ctrl Pts',(208.961050468708,-71.113684992587,479.990002372603));
#50677=CARTESIAN_POINT('Ctrl Pts',(208.993942128078,-71.274294562834,479.797094336963));
#50678=CARTESIAN_POINT('Ctrl Pts',(209.065953103068,-71.526452514999,479.402919496983));
#50679=CARTESIAN_POINT('Ctrl Pts',(209.188907806238,-71.779984116282,478.806461141823));
#50680=CARTESIAN_POINT('Ctrl Pts',(209.348848617978,-71.958291490743,478.120849197763));
#50681=CARTESIAN_POINT('Ctrl Pts',(209.554336434708,-72.052539059859,477.343725141823));
#50682=CARTESIAN_POINT('Ctrl Pts',(209.814931170118,-72.047682890276,476.477320998803));
#50683=CARTESIAN_POINT('Ctrl Pts',(210.047132686068,-71.960063670979,475.802608065543));
#50684=CARTESIAN_POINT('Ctrl Pts',(210.190168871588,-71.881362788512,475.421422476963));
#50685=CARTESIAN_POINT('Ctrl Pts',(210.220559021638,-71.863634441064,475.341888759263));
#50686=CARTESIAN_POINT('Ctrl Pts',(210.426610820448,-70.615950955131,479.359791872623));
#50687=CARTESIAN_POINT('Ctrl Pts',(210.437198595458,-70.645062585471,479.332582761523));
#50688=CARTESIAN_POINT('Ctrl Pts',(210.488635525948,-70.780329866032,479.200142478203));
#50689=CARTESIAN_POINT('Ctrl Pts',(210.596397787298,-71.013440751854,478.920111957033));
#50690=CARTESIAN_POINT('Ctrl Pts',(210.766723027648,-71.293762523166,478.470340135433));
#50691=CARTESIAN_POINT('Ctrl Pts',(210.971444847848,-71.549628732834,477.920756457143));
#50692=CARTESIAN_POINT('Ctrl Pts',(211.214287422258,-71.771639918358,477.257793073053));
#50693=CARTESIAN_POINT('Ctrl Pts',(211.498180471698,-71.942527322346,476.469123872683));
#50694=CARTESIAN_POINT('Ctrl Pts',(211.730850264618,-72.009638215756,475.810711396473));
#50695=CARTESIAN_POINT('Ctrl Pts',(211.866917304058,-72.021141169012,475.421032570143));
#50696=CARTESIAN_POINT('Ctrl Pts',(211.895520581278,-72.022313562161,475.338910192213));
#50697=CARTESIAN_POINT('',(210.277543128129,-70.742002685702,479.379320405933));
#50698=CARTESIAN_POINT('Origin',(211.655917770968,-72.011994055132,481.093613272963));
#50699=CARTESIAN_POINT('Ctrl Pts',(210.277557169171,-70.7420068809479,479.379305544522));
#50700=CARTESIAN_POINT('Ctrl Pts',(210.280160578741,-70.7492044424187,479.371880371481));
#50701=CARTESIAN_POINT('Ctrl Pts',(210.282790072534,-70.7563928376239,479.364380567364));
#50702=CARTESIAN_POINT('Ctrl Pts',(210.285445698698,-70.7635713390691,479.356806032728));
#50703=CARTESIAN_POINT('Ctrl Pts',(210.303010512012,-70.8110513042353,479.306706629199));
#50704=CARTESIAN_POINT('Ctrl Pts',(210.321719670561,-70.8580999963955,479.253334602992));
#50705=CARTESIAN_POINT('Ctrl Pts',(210.34159323712,-70.9045511124946,479.196644783729));
#50706=CARTESIAN_POINT('Ctrl Pts',(210.356825602417,-70.9401542019962,479.153194100979));
#50707=CARTESIAN_POINT('Ctrl Pts',(210.372741792365,-70.9754058614108,479.107795006256));
#50708=CARTESIAN_POINT('Ctrl Pts',(210.389344701098,-71.0102232739627,479.060445491085));
#50709=CARTESIAN_POINT('Ctrl Pts',(210.397959575153,-71.0282892423349,479.035876897935));
#50710=CARTESIAN_POINT('Ctrl Pts',(210.406759745185,-71.0462403635195,479.010780894366));
#50711=CARTESIAN_POINT('Ctrl Pts',(210.415743205009,-71.0640622097134,478.985162468652));
#50712=CARTESIAN_POINT('Ctrl Pts',(210.437592471152,-71.1074078992673,478.922854202955));
#50713=CARTESIAN_POINT('Ctrl Pts',(210.460527104185,-71.1499888075461,478.857452485973));
#50714=CARTESIAN_POINT('Ctrl Pts',(210.484528025454,-71.1916308944509,478.788999974412));
#50715=CARTESIAN_POINT('Ctrl Pts',(210.498241624089,-71.2154242672025,478.749887714571));
#50716=CARTESIAN_POINT('Ctrl Pts',(210.512303025228,-71.2389111258196,478.709780310016));
#50717=CARTESIAN_POINT('Ctrl Pts',(210.526706043544,-71.2620589077047,478.668692955888));
#50718=CARTESIAN_POINT('Ctrl Pts',(210.54338313569,-71.2888614627661,478.621118372854));
#50719=CARTESIAN_POINT('Ctrl Pts',(210.560526992361,-71.3152111239887,478.572222070248));
#50720=CARTESIAN_POINT('Ctrl Pts',(210.578151125547,-71.3410926562255,478.521961253831));
#50721=CARTESIAN_POINT('Ctrl Pts',(210.605101823219,-71.3806705091173,478.445102774968));
#50722=CARTESIAN_POINT('Ctrl Pts',(210.633175694648,-71.4191559802251,478.365053363194));
#50723=CARTESIAN_POINT('Ctrl Pts',(210.662445142328,-71.4564687983787,478.281589220188));
#50724=CARTESIAN_POINT('Ctrl Pts',(210.67139173563,-71.4678739541101,478.256077302406));
#50725=CARTESIAN_POINT('Ctrl Pts',(210.680450001339,-71.479169193652,478.230246415156));
#50726=CARTESIAN_POINT('Ctrl Pts',(210.689621898206,-71.4903512773119,478.204090432413));
#50727=CARTESIAN_POINT('Ctrl Pts',(210.716593016753,-71.5232336034355,478.127175469087));
#50728=CARTESIAN_POINT('Ctrl Pts',(210.744552198908,-71.5551392419009,478.047446978764));
#50729=CARTESIAN_POINT('Ctrl Pts',(210.773572311252,-71.5859845480201,477.964692299568));
#50730=CARTESIAN_POINT('Ctrl Pts',(210.802831346308,-71.6170838036805,477.881256300735));
#50731=CARTESIAN_POINT('Ctrl Pts',(210.833168720309,-71.6471054203407,477.794744452416));
#50732=CARTESIAN_POINT('Ctrl Pts',(210.864674824082,-71.6759139021875,477.704893419951));
#50733=CARTESIAN_POINT('Ctrl Pts',(210.870046833889,-71.6808259486946,477.689573194036));
#50734=CARTESIAN_POINT('Ctrl Pts',(210.875452808655,-71.6857026097514,477.67415592533));
#50735=CARTESIAN_POINT('Ctrl Pts',(210.880893177905,-71.6905430691913,477.658640359874));
#50736=CARTESIAN_POINT('Ctrl Pts',(210.911737968914,-71.7179866034388,477.570673100312));
#50737=CARTESIAN_POINT('Ctrl Pts',(210.943686396808,-71.7442659054198,477.479554290886));
#50738=CARTESIAN_POINT('Ctrl Pts',(210.976804992788,-71.7691988042492,477.385104399128));
#50739=CARTESIAN_POINT('Ctrl Pts',(210.987054560879,-71.7769150566051,477.35587397531));
#50740=CARTESIAN_POINT('Ctrl Pts',(210.997416127991,-71.7845020756729,477.32632473439));
#50741=CARTESIAN_POINT('Ctrl Pts',(211.007891432172,-71.7919537134947,477.296452039278));
#50742=CARTESIAN_POINT('Ctrl Pts',(211.039279596389,-71.8142817745812,477.20694160181));
#50743=CARTESIAN_POINT('Ctrl Pts',(211.071689486874,-71.8353967743902,477.114525462315));
#50744=CARTESIAN_POINT('Ctrl Pts',(211.105177594679,-71.8551008150377,477.019051458798));
#50745=CARTESIAN_POINT('Ctrl Pts',(211.138084368878,-71.8744628052758,476.925234827115));
#50746=CARTESIAN_POINT('Ctrl Pts',(211.172019133444,-71.892457782187,476.828475866872));
#50747=CARTESIAN_POINT('Ctrl Pts',(211.206907722279,-71.9088265655436,476.728987212169));
#50748=CARTESIAN_POINT('Ctrl Pts',(211.233014365774,-71.9210750973934,476.654541242101));
#50749=CARTESIAN_POINT('Ctrl Pts',(211.259654769354,-71.9324134528417,476.578567736639));
#50750=CARTESIAN_POINT('Ctrl Pts',(211.286792129693,-71.9427410029755,476.501172213991));
#50751=CARTESIAN_POINT('Ctrl Pts',(211.312411494309,-71.9524908559146,476.428106002336));
#50752=CARTESIAN_POINT('Ctrl Pts',(211.338473676087,-71.9613399669066,476.353772691105));
#50753=CARTESIAN_POINT('Ctrl Pts',(211.364948044876,-71.9692011295693,476.278260167726));
#50754=CARTESIAN_POINT('Ctrl Pts',(211.403692567548,-71.9807057285056,476.167749632144));
#50755=CARTESIAN_POINT('Ctrl Pts',(211.443318711821,-71.9900966506597,476.054722035542));
#50756=CARTESIAN_POINT('Ctrl Pts',(211.483835022319,-71.9971271824968,475.939162362379));
#50757=CARTESIAN_POINT('Ctrl Pts',(211.524351332817,-72.0041577143339,475.823602689217));
#50758=CARTESIAN_POINT('Ctrl Pts',(211.565758028763,-72.0088279534614,475.705510341515));
#50759=CARTESIAN_POINT('Ctrl Pts',(211.608049442047,-72.0108586572647,475.584910908401));
#50760=CARTESIAN_POINT('Ctrl Pts',(211.62388197629,-72.0116188869426,475.539762389916));
#50761=CARTESIAN_POINT('Ctrl Pts',(211.639838343728,-72.012008864435,475.494262958125));
#50762=CARTESIAN_POINT('Ctrl Pts',(211.655917770953,-72.0120105964115,475.44841530268));
#50763=CARTESIAN_POINT('Origin',(317.344642938098,-69.47200726879,390.467477301753));
#50764=CARTESIAN_POINT('',(220.926808864541,-70.7420844858612,470.816561573067));
#50765=CARTESIAN_POINT('Origin',(219.548450751088,-69.47200726879,469.102280889483));
#50766=CARTESIAN_POINT('',(220.926793321158,-70.742010897009,470.816601139763));
#50767=CARTESIAN_POINT('Origin',(219.548450751088,-69.47200726879,469.102280889483));
#50768=CARTESIAN_POINT('Origin',(219.548426423888,-69.4721780735883,469.102247110923));
#50769=CARTESIAN_POINT('Origin',(219.548450751088,-69.47200726879,469.102280889483));
#50770=CARTESIAN_POINT('Origin',(263.115917770968,-69.47200726879,445.000000551893));
#50771=CARTESIAN_POINT('Ctrl Pts',(220.743942614928,-70.841025529003,470.882368461713));
#50772=CARTESIAN_POINT('Ctrl Pts',(220.766984976348,-70.713370319682,470.948607761433));
#50773=CARTESIAN_POINT('Ctrl Pts',(220.831469127998,-70.4246254674543,471.129903538223));
#50774=CARTESIAN_POINT('Ctrl Pts',(220.971244196048,-70.0353627526102,471.494352564573));
#50775=CARTESIAN_POINT('Ctrl Pts',(221.172069843028,-69.7138478805081,471.964996709473));
#50776=CARTESIAN_POINT('Ctrl Pts',(221.415156299428,-69.5133172296706,472.474231282293));
#50777=CARTESIAN_POINT('Ctrl Pts',(221.617949220798,-69.4612216318851,472.854013581933));
#50778=CARTESIAN_POINT('Ctrl Pts',(221.733039042858,-69.4642140921138,473.056027688663));
#50779=CARTESIAN_POINT('Ctrl Pts',(221.751139833958,-69.4654397984221,473.087490581763));
#50780=CARTESIAN_POINT('Ctrl Pts',(222.160456726778,-70.78217857104,469.976495610993));
#50781=CARTESIAN_POINT('Ctrl Pts',(222.188437764768,-70.65379562633,470.050541672503));
#50782=CARTESIAN_POINT('Ctrl Pts',(222.264991790468,-70.3700937558322,470.250598510653));
#50783=CARTESIAN_POINT('Ctrl Pts',(222.418383534888,-70.0138432466795,470.636006555953));
#50784=CARTESIAN_POINT('Ctrl Pts',(222.618697713718,-69.7486471121804,471.105944703483));
#50785=CARTESIAN_POINT('Ctrl Pts',(222.842402309448,-69.6065541583209,471.587319564183));
#50786=CARTESIAN_POINT('Ctrl Pts',(223.019053538838,-69.5866015108655,471.930604628433));
#50787=CARTESIAN_POINT('Ctrl Pts',(223.117750638108,-69.6011568594972,472.110264950363));
#50788=CARTESIAN_POINT('Ctrl Pts',(223.133244421858,-69.6040467889201,472.138186261513));
#50789=CARTESIAN_POINT('Ctrl Pts',(222.452890157098,-70.1428865776801,468.447972465233));
#50790=CARTESIAN_POINT('Ctrl Pts',(222.505721982168,-69.9491917378316,468.554105655433));
#50791=CARTESIAN_POINT('Ctrl Pts',(222.649435816318,-69.5229124374613,468.840347590763));
#50792=CARTESIAN_POINT('Ctrl Pts',(222.931550749668,-68.9946418506585,469.388700140293));
#50793=CARTESIAN_POINT('Ctrl Pts',(223.288048531598,-68.6097419549078,470.052830454413));
#50794=CARTESIAN_POINT('Ctrl Pts',(223.671268133938,-68.410944976237,470.729926687363));
#50795=CARTESIAN_POINT('Ctrl Pts',(223.962129370818,-68.389326074635,471.212424905133));
#50796=CARTESIAN_POINT('Ctrl Pts',(224.121103779498,-68.41430577095,471.465655686903));
#50797=CARTESIAN_POINT('Ctrl Pts',(224.145979255988,-68.419099312272,471.505032467103));
#50798=CARTESIAN_POINT('Ctrl Pts',(221.415842816088,-69.3721769829706,467.370406754793));
#50799=CARTESIAN_POINT('Ctrl Pts',(221.495982783688,-69.0944600128107,467.510370006663));
#50800=CARTESIAN_POINT('Ctrl Pts',(221.714774494368,-68.478126745993,467.889686180993));
#50801=CARTESIAN_POINT('Ctrl Pts',(222.150306228938,-67.693627670348,468.628519370763));
#50802=CARTESIAN_POINT('Ctrl Pts',(222.709982073808,-67.097079327632,469.545342858623));
#50803=CARTESIAN_POINT('Ctrl Pts',(223.319573019498,-66.766264510463,470.504270304253));
#50804=CARTESIAN_POINT('Ctrl Pts',(223.784776866048,-66.710340497797,471.203911197863));
#50805=CARTESIAN_POINT('Ctrl Pts',(224.038360896088,-66.737284122903,471.574962089193));
#50806=CARTESIAN_POINT('Ctrl Pts',(224.078017229698,-66.742883601444,471.632745269773));
#50807=CARTESIAN_POINT('Ctrl Pts',(220.926793321158,-70.742010897009,470.816601139763));
#50808=CARTESIAN_POINT('Ctrl Pts',(220.954019546588,-70.609423932937,470.892937850223));
#50809=CARTESIAN_POINT('Ctrl Pts',(221.017898643648,-70.3602758137923,471.067167472223));
#50810=CARTESIAN_POINT('Ctrl Pts',(221.140717502368,-70.0432002664185,471.381409203203));
#50811=CARTESIAN_POINT('Ctrl Pts',(221.288915933368,-69.7913397688457,471.732484521923));
#50812=CARTESIAN_POINT('Ctrl Pts',(221.460643994418,-69.6083606197754,472.107646252993));
#50813=CARTESIAN_POINT('Ctrl Pts',(221.65355487452,-69.4970261598067,472.495428146088));
#50814=CARTESIAN_POINT('Ctrl Pts',(221.7939110984,-69.4720061889133,472.755478514282));
#50815=CARTESIAN_POINT('Ctrl Pts',(221.866228108069,-69.4720072829599,472.883816237293));
#50816=CARTESIAN_POINT('Origin',(221.866229658798,-66.93200726879,472.883818989273));
#50817=CARTESIAN_POINT('Origin',(263.115917770968,-66.93200726879,445.000000551893));
#50818=CARTESIAN_POINT('Origin',(317.464909153118,-72.01200726879,396.015965372443));
#50819=CARTESIAN_POINT('Origin',(211.655917770968,-72.01200726879,481.093605606543));
#50820=CARTESIAN_POINT('Origin',(211.655917770968,-72.01200726879,481.093605606543));
#50821=CARTESIAN_POINT('Origin',(305.864311867508,-72.0120072687901,496.460000551893));
#50822=CARTESIAN_POINT('Origin',(227.022312716318,-72.01200726879,496.460000551893));
#50823=CARTESIAN_POINT('Origin',(227.022312716318,-72.01200726879,496.460000551893));
#50824=CARTESIAN_POINT('Ctrl Pts',(300.593104002278,-72.7677512570001,498.460410335103));
#50825=CARTESIAN_POINT('Ctrl Pts',(300.530601966458,-72.8415267130751,498.467865703403));
#50826=CARTESIAN_POINT('Ctrl Pts',(300.228734977818,-73.1792881921421,498.503643117423));
#50827=CARTESIAN_POINT('Ctrl Pts',(299.613647012858,-73.7177818201391,498.573974279533));
#50828=CARTESIAN_POINT('Ctrl Pts',(298.687681543188,-74.2773859034231,498.671516960093));
#50829=CARTESIAN_POINT('Ctrl Pts',(297.629286318018,-74.6941844569291,498.770637036323));
#50830=CARTESIAN_POINT('Ctrl Pts',(296.436962017048,-74.9488215698491,498.864713036083));
#50831=CARTESIAN_POINT('Ctrl Pts',(295.116742985068,-75.0078404229171,498.944324324143));
#50832=CARTESIAN_POINT('Ctrl Pts',(294.096734072578,-74.8793277233351,498.981804574093));
#50833=CARTESIAN_POINT('Ctrl Pts',(293.523716758098,-74.7445966300441,498.992925994703));
#50834=CARTESIAN_POINT('Ctrl Pts',(293.404307436158,-74.7136854275461,498.994784080203));
#50835=CARTESIAN_POINT('Ctrl Pts',(299.502629808648,-72.0150401412131,499.497186230093));
#50836=CARTESIAN_POINT('Ctrl Pts',(299.447350359308,-72.0696574342111,499.498329782803));
#50837=CARTESIAN_POINT('Ctrl Pts',(299.180702325308,-72.3183990485601,499.503396635393));
#50838=CARTESIAN_POINT('Ctrl Pts',(298.640699616528,-72.7034694767341,499.508897695653));
#50839=CARTESIAN_POINT('Ctrl Pts',(297.836986338008,-73.0785538001051,499.502527801293));
#50840=CARTESIAN_POINT('Ctrl Pts',(296.929923102898,-73.3269041512491,499.474828839513));
#50841=CARTESIAN_POINT('Ctrl Pts',(295.922404003468,-73.4353515823531,499.415978915893));
#50842=CARTESIAN_POINT('Ctrl Pts',(294.824652130248,-73.3818065903941,499.313593060243));
#50843=CARTESIAN_POINT('Ctrl Pts',(293.992560697738,-73.2090456373971,499.198969606623));
#50844=CARTESIAN_POINT('Ctrl Pts',(293.531580251618,-73.0666989540421,499.119994613703));
#50845=CARTESIAN_POINT('Ctrl Pts',(293.435818046288,-73.0350067849761,499.102862236873));
#50846=CARTESIAN_POINT('Ctrl Pts',(298.145838415288,-71.0785068454431,499.161577262733));
#50847=CARTESIAN_POINT('Ctrl Pts',(298.105919591678,-71.1136849925871,499.154867854153));
#50848=CARTESIAN_POINT('Ctrl Pts',(297.913011556038,-71.2742945628341,499.121976194783));
#50849=CARTESIAN_POINT('Ctrl Pts',(297.518836716058,-71.5264525149991,499.049965219793));
#50850=CARTESIAN_POINT('Ctrl Pts',(296.922378360898,-71.7799841162821,498.927010516623));
#50851=CARTESIAN_POINT('Ctrl Pts',(296.236766416838,-71.9582914907431,498.767069704883));
#50852=CARTESIAN_POINT('Ctrl Pts',(295.459642360898,-72.0525390598591,498.561581888153));
#50853=CARTESIAN_POINT('Ctrl Pts',(294.593238217878,-72.0476828902761,498.300987152743));
#50854=CARTESIAN_POINT('Ctrl Pts',(293.918525284618,-71.9600636709791,498.068785636793));
#50855=CARTESIAN_POINT('Ctrl Pts',(293.537339696038,-71.8813627885121,497.925749451273));
#50856=CARTESIAN_POINT('Ctrl Pts',(293.457805978338,-71.8636344410641,497.895359301223));
#50857=CARTESIAN_POINT('Ctrl Pts',(297.475709091698,-70.6159509551311,497.689307502413));
#50858=CARTESIAN_POINT('Ctrl Pts',(297.448499980598,-70.6450625854711,497.678719727403));
#50859=CARTESIAN_POINT('Ctrl Pts',(297.316059697278,-70.7803298660321,497.627282796913));
#50860=CARTESIAN_POINT('Ctrl Pts',(297.036029176108,-71.0134407518541,497.519520535563));
#50861=CARTESIAN_POINT('Ctrl Pts',(296.586257354508,-71.2937625231661,497.349195295213));
#50862=CARTESIAN_POINT('Ctrl Pts',(296.036673676218,-71.5496287328341,497.144473475013));
#50863=CARTESIAN_POINT('Ctrl Pts',(295.373710292128,-71.7716399183581,496.901630900603));
#50864=CARTESIAN_POINT('Ctrl Pts',(294.585041091768,-71.9425273223461,496.617737851163));
#50865=CARTESIAN_POINT('Ctrl Pts',(293.926628615548,-72.0096382157561,496.385068058243));
#50866=CARTESIAN_POINT('Ctrl Pts',(293.536949789218,-72.0211411690121,496.249001018803));
#50867=CARTESIAN_POINT('Ctrl Pts',(293.454827411288,-72.0223135621611,496.220397741583));
#50868=CARTESIAN_POINT('Origin',(263.115917770968,-56.01200726879,445.000000551893));
#50869=CARTESIAN_POINT('',(262.871473015597,-53.47200726879,489.709332148996));
#50870=CARTESIAN_POINT('Origin',(263.115917770968,-53.47200726879,445.000000551893));
#50871=CARTESIAN_POINT('Origin',(262.871473014686,-56.01200726879,489.709332315644));
#50872=CARTESIAN_POINT('Origin',(263.115917770968,-53.47200726879,445.000000551893));
#50873=CARTESIAN_POINT('',(263.50896067409,-53.47200726879,483.287981846615));
#50874=CARTESIAN_POINT('Origin',(263.115917770968,-53.47200726879,445.000000551893));
#50875=CARTESIAN_POINT('Origin',(263.115917770968,-56.01200726879,445.000000551893));
#50876=CARTESIAN_POINT('',(263.115917770968,-56.01200726879,480.750000551893));
#50877=CARTESIAN_POINT('',(263.482887849132,-56.01200726879,480.748117047196));
#50878=CARTESIAN_POINT('Origin',(263.115917770968,-56.01200726879,445.000000551893));
#50879=CARTESIAN_POINT('Origin',(263.115917770968,-56.01200726879,445.000000551893));
#50880=CARTESIAN_POINT('Origin',(263.508960688251,-56.01200726879,483.287983226163));
#50881=CARTESIAN_POINT('Origin',(263.115917770968,-86.89200726879,445.000000551893));
#50882=CARTESIAN_POINT('',(263.115917770968,-55.25000726879,480.750000551893));
#50883=CARTESIAN_POINT('Origin',(263.115917770968,-55.25000726879,445.000000551893));
#50884=CARTESIAN_POINT('',(263.115917770968,-86.89200726879,480.750000551893));
#50885=CARTESIAN_POINT('Origin',(263.115917770968,-55.25000726879,445.000000551893));
#50886=CARTESIAN_POINT('',(263.115917770968,-55.25000726879,472.315000551893));
#50887=CARTESIAN_POINT('Origin',(263.115917770968,-55.25000726879,445.000000551893));
#50888=CARTESIAN_POINT('Origin',(263.115917770968,-86.89200726879,445.000000551893));
#50889=CARTESIAN_POINT('',(263.115917770968,-56.01200726879,472.315000551893));
#50890=CARTESIAN_POINT('Origin',(263.115917770968,-56.01200726879,445.000000551893));
#50891=CARTESIAN_POINT('',(263.115917770968,-86.89200726879,472.315000551893));
#50892=CARTESIAN_POINT('Origin',(263.115917770968,-56.01200726879,445.000000551893));
#50893=CARTESIAN_POINT('',(263.115917770968,-56.01200726879,468.435000551893));
#50894=CARTESIAN_POINT('Origin',(263.115917770968,-56.01200726879,445.000000551893));
#50895=CARTESIAN_POINT('Origin',(263.115917770968,-86.89200726879,445.000000551893));
#50896=CARTESIAN_POINT('',(263.115917770968,-36.07200726879,468.435000551893));
#50897=CARTESIAN_POINT('Origin',(263.115917770968,-36.07200726879,445.000000551893));
#50898=CARTESIAN_POINT('',(263.115917770968,-86.89200726879,468.435000551893));
#50899=CARTESIAN_POINT('Origin',(263.115917770968,-36.07200726879,445.000000551893));
#50900=CARTESIAN_POINT('',(263.115917770968,-36.07200726879,460.000000551893));
#50901=CARTESIAN_POINT('Origin',(263.115917770968,-36.07200726879,445.000000551893));
#50902=CARTESIAN_POINT('Origin',(263.115917770968,-86.89200726879,445.000000551893));
#50903=CARTESIAN_POINT('',(263.115917770968,-84.47200726879,460.000000551893));
#50904=CARTESIAN_POINT('Origin',(263.115917770968,-84.47200726879,445.000000551893));
#50905=CARTESIAN_POINT('',(263.115917770968,-86.89200726879,460.000000551893));
#50906=CARTESIAN_POINT('Origin',(263.115917770968,-84.47200726879,445.000000551893));
#50907=CARTESIAN_POINT('',(263.115917770968,-84.47200726879,468.435000551893));
#50908=CARTESIAN_POINT('Origin',(263.115917770968,-84.47200726879,445.000000551893));
#50909=CARTESIAN_POINT('Origin',(263.115917770968,-86.89200726879,445.000000551893));
#50910=CARTESIAN_POINT('',(263.115917770968,-76.33200726879,468.435000551893));
#50911=CARTESIAN_POINT('Origin',(263.115917770968,-76.33200726879,445.000000551893));
#50912=CARTESIAN_POINT('',(263.115917770968,-86.89200726879,468.435000551893));
#50913=CARTESIAN_POINT('Origin',(263.115917770968,-76.33200726879,445.000000551893));
#50914=CARTESIAN_POINT('',(263.115917770968,-76.33200726879,472.315000551893));
#50915=CARTESIAN_POINT('Origin',(263.115917770968,-76.33200726879,445.000000551893));
#50916=CARTESIAN_POINT('Origin',(263.115917770968,-86.89200726879,445.000000551893));
#50917=CARTESIAN_POINT('',(263.115917770968,-77.0940072687901,472.315000551893));
#50918=CARTESIAN_POINT('Origin',(263.115917770968,-77.09400726879,445.000000551893));
#50919=CARTESIAN_POINT('',(263.115917770968,-86.89200726879,472.315000551893));
#50920=CARTESIAN_POINT('Origin',(263.115917770968,-77.09400726879,445.000000551893));
#50921=CARTESIAN_POINT('',(263.115917770968,-77.09400726879,480.750000551893));
#50922=CARTESIAN_POINT('Origin',(263.115917770968,-77.09400726879,445.000000551893));
#50923=CARTESIAN_POINT('Origin',(263.115917770968,-85.47200726879,445.000000551893));
#50924=CARTESIAN_POINT('',(263.115917770968,-81.66200726879,480.750000551893));
#50925=CARTESIAN_POINT('Origin',(263.115917770968,-81.66200726879,445.000000551893));
#50926=CARTESIAN_POINT('',(263.115917770968,-85.47200726879,480.750000551893));
#50927=CARTESIAN_POINT('Origin',(263.115917770968,-81.66200726879,445.000000551893));
#50928=CARTESIAN_POINT('',(293.115917770968,-81.66200726879,403.500000551893));
#50929=CARTESIAN_POINT('',(304.615917770968,-81.66200726879,415.000000551893));
#50930=CARTESIAN_POINT('Origin',(304.615917770968,-81.66200726879,403.500000551893));
#50931=CARTESIAN_POINT('',(304.615917770968,-81.66200726879,475.000000551893));
#50932=CARTESIAN_POINT('',(304.615917770968,-81.66200726879,415.000000551893));
#50933=CARTESIAN_POINT('',(293.115917770968,-81.66200726879,486.500000551893));
#50934=CARTESIAN_POINT('Origin',(304.615917770968,-81.6620072687901,486.500000551893));
#50935=CARTESIAN_POINT('',(233.115917770968,-81.66200726879,486.500000551893));
#50936=CARTESIAN_POINT('',(293.115917770968,-81.66200726879,486.500000551893));
#50937=CARTESIAN_POINT('',(221.615917770968,-81.66200726879,475.000000551893));
#50938=CARTESIAN_POINT('Origin',(221.615917770968,-81.66200726879,486.500000551893));
#50939=CARTESIAN_POINT('',(221.615917770968,-81.6620072687899,415.000000551893));
#50940=CARTESIAN_POINT('',(221.615917770968,-81.66200726879,475.000000551893));
#50941=CARTESIAN_POINT('',(233.115917770968,-81.6620072687899,403.500000551893));
#50942=CARTESIAN_POINT('Origin',(221.615917770968,-81.6620072687899,403.500000551893));
#50943=CARTESIAN_POINT('',(233.115917770968,-81.6620072687899,403.500000551893));
#50944=CARTESIAN_POINT('Origin',(304.615917770968,-85.47200726879,403.500000551893));
#50945=CARTESIAN_POINT('',(304.615917770968,-85.47200726879,415.000000551893));
#50946=CARTESIAN_POINT('',(293.115917770968,-85.47200726879,403.500000551893));
#50947=CARTESIAN_POINT('Origin',(233.115917770968,-85.4720072687899,403.500000551893));
#50948=CARTESIAN_POINT('',(233.115917770968,-85.4720072687899,403.500000551893));
#50949=CARTESIAN_POINT('Origin',(221.615917770968,-85.4720072687899,403.500000551893));
#50950=CARTESIAN_POINT('',(221.615917770968,-85.47200726879,415.000000551893));
#50951=CARTESIAN_POINT('Origin',(221.615917770968,-85.47200726879,475.000000551893));
#50952=CARTESIAN_POINT('',(221.615917770968,-85.47200726879,475.000000551893));
#50953=CARTESIAN_POINT('Origin',(221.615917770968,-85.47200726879,486.500000551893));
#50954=CARTESIAN_POINT('',(233.115917770968,-85.47200726879,486.500000551893));
#50955=CARTESIAN_POINT('Origin',(293.115917770968,-85.4720072687901,486.500000551893));
#50956=CARTESIAN_POINT('',(293.115917770968,-85.4720072687901,486.500000551893));
#50957=CARTESIAN_POINT('Origin',(304.615917770968,-85.4720072687901,486.500000551893));
#50958=CARTESIAN_POINT('',(304.615917770968,-85.4720072687901,475.000000551893));
#50959=CARTESIAN_POINT('Origin',(304.615917770968,-85.47200726879,415.000000551893));
#50960=CARTESIAN_POINT('',(0.,0.,0.));
#50961=CARTESIAN_POINT('Origin',(221.615917770968,-69.5720072687899,403.500000551893));
#50962=CARTESIAN_POINT('',(215.615917770968,-69.5720072687899,403.500000551893));
#50963=CARTESIAN_POINT('',(221.615917770968,-69.5720072687899,397.500000551893));
#50964=CARTESIAN_POINT('Origin',(221.615917770968,-69.5720072687899,403.500000551893));
#50965=CARTESIAN_POINT('Origin',(221.615917770968,-69.5720072687899,403.500000551893));
#50966=CARTESIAN_POINT('',(215.515917770968,-69.4720072687899,403.500000551893));
#50967=CARTESIAN_POINT('Origin',(215.515917770968,-69.5720072687899,403.500000551893));
#50968=CARTESIAN_POINT('Origin',(221.615917770968,-69.4720072687899,403.500000551893));
#50969=CARTESIAN_POINT('Origin',(221.615917770968,-86.6595072687899,403.500000551893));
#50970=CARTESIAN_POINT('',(221.615917770968,-98.39846976879,409.500000551893));
#50971=CARTESIAN_POINT('',(221.615917770968,-98.3984697687899,397.500000551893));
#50972=CARTESIAN_POINT('Origin',(221.615917770968,-98.3984697687899,403.500000551893));
#50973=CARTESIAN_POINT('Origin',(221.615917770968,-98.3984697687899,403.500000551893));
#50974=CARTESIAN_POINT('',(221.615917770968,-86.6595072687899,397.500000551893));
#50975=CARTESIAN_POINT('Origin',(221.615917770968,-69.4720072687899,411.000000551893));
#50976=CARTESIAN_POINT('',(221.615917770968,-69.4720072687899,394.500000551893));
#50977=CARTESIAN_POINT('Origin',(221.615917770968,-69.4720072687899,403.500000551893));
#50978=CARTESIAN_POINT('Origin',(221.615917770968,-98.9352385187899,403.500000551893));
#50979=CARTESIAN_POINT('',(221.615917770968,-99.4720072687899,408.426463051893));
#50980=CARTESIAN_POINT('',(221.615917770968,-98.9352385187899,408.963231801893));
#50981=CARTESIAN_POINT('Origin',(221.615917770968,-99.4720072687899,403.500000551893));
#50982=CARTESIAN_POINT('Origin',(221.615917770968,-99.4720072687899,406.500000551893));
#50983=CARTESIAN_POINT('Origin',(221.615917770968,-58.6720072687899,403.500000551893));
#50984=CARTESIAN_POINT('',(212.615917770968,-58.6720072687899,403.500000551893));
#50985=CARTESIAN_POINT('',(221.615917770968,-58.6720072687899,394.500000551893));
#50986=CARTESIAN_POINT('Origin',(221.615917770968,-58.6720072687899,403.500000551893));
#50987=CARTESIAN_POINT('Origin',(221.615917770968,-58.6720072687899,403.500000551893));
#50988=CARTESIAN_POINT('',(213.815917770968,-57.4720072687899,403.500000551893));
#50989=CARTESIAN_POINT('Origin',(213.815917770968,-58.6720072687899,403.500000551893));
#50990=CARTESIAN_POINT('Origin',(221.615917770968,-57.4720072687899,403.500000551893));
#50991=CARTESIAN_POINT('Origin',(221.615917770968,-57.4720072687899,410.886751897841));
#50992=CARTESIAN_POINT('',(224.502669116916,-57.4720072687899,408.500000551893));
#50993=CARTESIAN_POINT('',(218.72916642502,-57.4720072687899,408.500000551893));
#50994=CARTESIAN_POINT('',(220.172542097994,-57.4720072687899,408.500000551893));
#50995=CARTESIAN_POINT('',(215.842415079072,-57.4720072687899,403.500000551893));
#50996=CARTESIAN_POINT('',(216.564102915559,-57.4720072687899,404.750000551893));
#50997=CARTESIAN_POINT('',(218.72916642502,-57.4720072687899,398.500000551893));
#50998=CARTESIAN_POINT('',(218.007478588533,-57.4720072687899,399.750000551893));
#50999=CARTESIAN_POINT('',(224.502669116916,-57.4720072687899,398.500000551893));
#51000=CARTESIAN_POINT('',(223.059293443942,-57.4720072687899,398.500000551893));
#51001=CARTESIAN_POINT('',(227.389420462865,-57.4720072687899,403.500000551893));
#51002=CARTESIAN_POINT('',(226.667732626378,-57.4720072687899,402.250000551893));
#51003=CARTESIAN_POINT('',(225.224356953403,-57.4720072687899,407.250000551893));
#51004=CARTESIAN_POINT('Origin',(221.615917770968,-63.4720072687899,403.500000551893));
#51005=CARTESIAN_POINT('',(221.615917770968,-63.4720072687899,394.500000551893));
#51006=CARTESIAN_POINT('Origin',(227.389420462865,-57.4720072687899,403.500000551893));
#51007=CARTESIAN_POINT('',(227.389420462865,-63.4720072687899,403.500000551893));
#51008=CARTESIAN_POINT('',(224.502669116916,-63.4720072687899,398.500000551893));
#51009=CARTESIAN_POINT('Ctrl Pts',(227.389420462865,-63.4720072687899,403.500000551893));
#51010=CARTESIAN_POINT('Ctrl Pts',(225.94604478989,-64.3053406021233,401.000000551893));
#51011=CARTESIAN_POINT('Ctrl Pts',(224.502669116916,-63.4720072687899,398.500000551893));
#51012=CARTESIAN_POINT('',(227.389420462865,-60.4720072687899,403.500000551893));
#51013=CARTESIAN_POINT('',(224.502669116916,-60.4720072687899,398.500000551893));
#51014=CARTESIAN_POINT('Origin',(224.502669116916,-57.4720072687899,408.500000551893));
#51015=CARTESIAN_POINT('',(224.502669116916,-63.4720072687899,408.500000551893));
#51016=CARTESIAN_POINT('Ctrl Pts',(224.502669116916,-63.4720072687899,408.500000551893));
#51017=CARTESIAN_POINT('Ctrl Pts',(225.946044789891,-64.3053406021233,406.000000551893));
#51018=CARTESIAN_POINT('Ctrl Pts',(227.389420462865,-63.4720072687899,403.500000551893));
#51019=CARTESIAN_POINT('',(224.502669116916,-60.4720072687899,408.500000551893));
#51020=CARTESIAN_POINT('Origin',(218.72916642502,-57.4720072687899,408.500000551893));
#51021=CARTESIAN_POINT('',(218.72916642502,-63.4720072687899,408.500000551893));
#51022=CARTESIAN_POINT('Ctrl Pts',(218.72916642502,-63.4720072687899,408.500000551893));
#51023=CARTESIAN_POINT('Ctrl Pts',(221.615917770968,-64.3053406021233,408.500000551893));
#51024=CARTESIAN_POINT('Ctrl Pts',(224.502669116916,-63.4720072687899,408.500000551893));
#51025=CARTESIAN_POINT('',(218.72916642502,-60.4720072687899,408.500000551893));
#51026=CARTESIAN_POINT('Origin',(215.842415079072,-57.4720072687899,403.500000551893));
#51027=CARTESIAN_POINT('',(215.842415079072,-63.4720072687899,403.500000551893));
#51028=CARTESIAN_POINT('Ctrl Pts',(215.842415079072,-63.4720072687899,403.500000551893));
#51029=CARTESIAN_POINT('Ctrl Pts',(217.285790752046,-64.3053406021233,406.000000551893));
#51030=CARTESIAN_POINT('Ctrl Pts',(218.72916642502,-63.4720072687899,408.500000551893));
#51031=CARTESIAN_POINT('',(215.842415079072,-60.4720072687899,403.500000551893));
#51032=CARTESIAN_POINT('Origin',(224.502669116916,-57.4720072687899,398.500000551893));
#51033=CARTESIAN_POINT('',(221.615917770968,-63.9185892561751,398.500000551893));
#51034=CARTESIAN_POINT('Ctrl Pts',(224.502669116916,-63.4720072687899,398.500000551893));
#51035=CARTESIAN_POINT('Ctrl Pts',(222.955663733124,-63.9185892561751,398.500000551893));
#51036=CARTESIAN_POINT('Ctrl Pts',(221.615917770968,-63.9185892561751,398.500000551893));
#51037=CARTESIAN_POINT('',(218.72916642502,-63.4720072687899,398.500000551893));
#51038=CARTESIAN_POINT('',(218.72916642502,-60.4720072687899,398.500000551893));
#51039=CARTESIAN_POINT('Ctrl Pts',(221.615917770968,-63.9185892561751,398.500000551893));
#51040=CARTESIAN_POINT('Ctrl Pts',(220.276171808813,-63.9185892561751,398.500000551893));
#51041=CARTESIAN_POINT('Ctrl Pts',(218.72916642502,-63.4720072687899,398.500000551893));
#51042=CARTESIAN_POINT('Origin',(218.72916642502,-57.4720072687899,398.500000551893));
#51043=CARTESIAN_POINT('Ctrl Pts',(218.72916642502,-63.4720072687899,398.500000551893));
#51044=CARTESIAN_POINT('Ctrl Pts',(217.285790752046,-64.3053406021233,401.000000551893));
#51045=CARTESIAN_POINT('Ctrl Pts',(215.842415079072,-63.4720072687899,403.500000551893));
#51046=CARTESIAN_POINT('Origin',(221.615917770968,-65.1386739354566,403.500000551893));
#51047=CARTESIAN_POINT('',(221.615917770968,-66.8053406021233,403.500000551893));
#51048=CARTESIAN_POINT('',(221.615917770968,-65.1386739354566,400.613249205945));
#51049=CARTESIAN_POINT('',(0.,0.,0.));
#51050=CARTESIAN_POINT('Origin',(474.015917770968,-92.9720072687899,380.000000551893));
#51051=CARTESIAN_POINT('',(474.015917770968,-92.9720072687899,375.000000551893));
#51052=CARTESIAN_POINT('',(474.015917770968,-97.9720072687899,380.000000551893));
#51053=CARTESIAN_POINT('Origin',(474.015917770968,-92.9720072687899,380.000000551893));
#51054=CARTESIAN_POINT('Origin',(474.015917770968,-92.9720072687899,380.000000551893));
#51055=CARTESIAN_POINT('',(474.115917770968,-92.9720072687899,374.900000551893));
#51056=CARTESIAN_POINT('Origin',(474.015917770968,-92.9720072687899,374.900000551893));
#51057=CARTESIAN_POINT('Origin',(474.115917770968,-92.9720072687899,380.000000551893));
#51058=CARTESIAN_POINT('Origin',(459.740917770968,-92.9720072687899,380.000000551893));
#51059=CARTESIAN_POINT('',(450.036092770968,-87.9720072687899,380.000000551893));
#51060=CARTESIAN_POINT('',(450.036092770968,-97.9720072687899,380.000000551893));
#51061=CARTESIAN_POINT('Origin',(450.036092770968,-92.9720072687899,380.000000551893));
#51062=CARTESIAN_POINT('Origin',(450.036092770968,-92.9720072687899,380.000000551893));
#51063=CARTESIAN_POINT('',(459.740917770968,-97.9720072687899,380.000000551893));
#51064=CARTESIAN_POINT('Origin',(474.115917770968,-86.4720072687899,380.000000551893));
#51065=CARTESIAN_POINT('',(474.115917770968,-100.97200726879,380.000000551893));
#51066=CARTESIAN_POINT('Origin',(474.115917770968,-92.9720072687899,380.000000551893));
#51067=CARTESIAN_POINT('Origin',(449.576005270968,-92.9720072687899,380.000000551893));
#51068=CARTESIAN_POINT('',(449.115917770968,-88.8921822687899,380.000000551893));
#51069=CARTESIAN_POINT('',(449.576005270968,-88.4320947687899,380.000000551893));
#51070=CARTESIAN_POINT('Origin',(449.115917770968,-92.9720072687899,380.000000551893));
#51071=CARTESIAN_POINT('Origin',(449.115917770968,-90.4720072687899,380.000000551893));
#51072=CARTESIAN_POINT('Origin',(483.115917770968,-92.9720072687899,380.000000551893));
#51073=CARTESIAN_POINT('',(483.115917770968,-92.9720072687899,372.000000551893));
#51074=CARTESIAN_POINT('',(483.115917770968,-100.97200726879,380.000000551893));
#51075=CARTESIAN_POINT('Origin',(483.115917770968,-92.9720072687899,380.000000551893));
#51076=CARTESIAN_POINT('Origin',(483.115917770968,-92.9720072687899,380.000000551893));
#51077=CARTESIAN_POINT('',(484.115917770968,-92.9720072687899,373.000000551893));
#51078=CARTESIAN_POINT('Origin',(483.115917770968,-92.9720072687899,373.000000551893));
#51079=CARTESIAN_POINT('Origin',(484.115917770968,-92.9720072687899,380.000000551893));
#51080=CARTESIAN_POINT('Origin',(484.115917770968,-86.6626061920314,380.000000551893));
#51081=CARTESIAN_POINT('',(484.115917770968,-88.9720072687899,382.309401628651));
#51082=CARTESIAN_POINT('',(484.115917770968,-88.9720072687899,377.690599475134));
#51083=CARTESIAN_POINT('',(484.115917770968,-88.9720072687899,378.845300013513));
#51084=CARTESIAN_POINT('',(484.115917770968,-92.9720072687899,375.381198398376));
#51085=CARTESIAN_POINT('',(484.115917770968,-91.9720072687899,375.958548667565));
#51086=CARTESIAN_POINT('',(484.115917770968,-96.9720072687899,377.690599475134));
#51087=CARTESIAN_POINT('',(484.115917770968,-95.9720072687899,377.113249205944));
#51088=CARTESIAN_POINT('',(484.115917770968,-96.9720072687899,382.309401628651));
#51089=CARTESIAN_POINT('',(484.115917770968,-96.9720072687899,381.154701090272));
#51090=CARTESIAN_POINT('',(484.115917770968,-92.97200726879,384.61880270541));
#51091=CARTESIAN_POINT('',(484.115917770968,-93.9720072687899,384.04145243622));
#51092=CARTESIAN_POINT('',(484.115917770968,-89.9720072687899,382.886751897841));
#51093=CARTESIAN_POINT('Origin',(479.115917770968,-92.9720072687899,380.000000551893));
#51094=CARTESIAN_POINT('',(479.115917770968,-100.97200726879,380.000000551893));
#51095=CARTESIAN_POINT('Origin',(484.115917770968,-92.97200726879,384.61880270541));
#51096=CARTESIAN_POINT('',(479.115917770968,-92.97200726879,384.61880270541));
#51097=CARTESIAN_POINT('',(479.115917770968,-96.9720072687899,382.309401628651));
#51098=CARTESIAN_POINT('Ctrl Pts',(479.115917770968,-92.97200726879,384.61880270541));
#51099=CARTESIAN_POINT('Ctrl Pts',(478.449251104301,-94.9720072687899,383.46410216703));
#51100=CARTESIAN_POINT('Ctrl Pts',(479.115917770968,-96.9720072687899,382.309401628651));
#51101=CARTESIAN_POINT('',(481.615917770968,-92.97200726879,384.61880270541));
#51102=CARTESIAN_POINT('',(481.615917770968,-96.9720072687899,382.309401628651));
#51103=CARTESIAN_POINT('Origin',(484.115917770968,-88.9720072687899,382.309401628651));
#51104=CARTESIAN_POINT('',(479.115917770968,-88.9720072687899,382.309401628651));
#51105=CARTESIAN_POINT('Ctrl Pts',(479.115917770968,-88.9720072687899,382.309401628651));
#51106=CARTESIAN_POINT('Ctrl Pts',(478.449251104301,-90.9720072687899,383.46410216703));
#51107=CARTESIAN_POINT('Ctrl Pts',(479.115917770968,-92.9720072687899,384.61880270541));
#51108=CARTESIAN_POINT('',(481.615917770968,-88.9720072687899,382.309401628651));
#51109=CARTESIAN_POINT('Origin',(484.115917770968,-88.9720072687899,377.690599475134));
#51110=CARTESIAN_POINT('',(479.115917770968,-88.9720072687899,377.690599475134));
#51111=CARTESIAN_POINT('Ctrl Pts',(479.115917770968,-88.9720072687899,377.690599475134));
#51112=CARTESIAN_POINT('Ctrl Pts',(478.449251104301,-88.9720072687899,380.000000551893));
#51113=CARTESIAN_POINT('Ctrl Pts',(479.115917770968,-88.9720072687899,382.309401628651));
#51114=CARTESIAN_POINT('',(481.615917770968,-88.9720072687899,377.690599475134));
#51115=CARTESIAN_POINT('Origin',(484.115917770968,-92.9720072687899,375.381198398376));
#51116=CARTESIAN_POINT('',(479.115917770968,-92.9720072687899,375.381198398376));
#51117=CARTESIAN_POINT('Ctrl Pts',(479.115917770968,-92.9720072687899,375.381198398376));
#51118=CARTESIAN_POINT('Ctrl Pts',(478.449251104301,-90.9720072687899,376.535898936755));
#51119=CARTESIAN_POINT('Ctrl Pts',(479.115917770968,-88.9720072687899,377.690599475134));
#51120=CARTESIAN_POINT('',(481.615917770968,-92.9720072687899,375.381198398376));
#51121=CARTESIAN_POINT('Origin',(484.115917770968,-96.9720072687899,382.309401628651));
#51122=CARTESIAN_POINT('',(478.75865218106,-96.9720072687899,380.000000551893));
#51123=CARTESIAN_POINT('Ctrl Pts',(479.115917770968,-96.9720072687899,382.309401628651));
#51124=CARTESIAN_POINT('Ctrl Pts',(478.75865218106,-96.9720072687899,381.071797321617));
#51125=CARTESIAN_POINT('Ctrl Pts',(478.75865218106,-96.9720072687899,380.000000551893));
#51126=CARTESIAN_POINT('',(479.115917770968,-96.9720072687899,377.690599475134));
#51127=CARTESIAN_POINT('',(481.615917770968,-96.9720072687899,377.690599475134));
#51128=CARTESIAN_POINT('Ctrl Pts',(478.75865218106,-96.9720072687899,380.000000551893));
#51129=CARTESIAN_POINT('Ctrl Pts',(478.75865218106,-96.9720072687899,378.928203782168));
#51130=CARTESIAN_POINT('Ctrl Pts',(479.115917770968,-96.9720072687899,377.690599475134));
#51131=CARTESIAN_POINT('Origin',(484.115917770968,-96.9720072687899,377.690599475134));
#51132=CARTESIAN_POINT('Ctrl Pts',(479.115917770968,-96.9720072687899,377.690599475134));
#51133=CARTESIAN_POINT('Ctrl Pts',(478.449251104301,-94.9720072687899,376.535898936755));
#51134=CARTESIAN_POINT('Ctrl Pts',(479.115917770968,-92.9720072687899,375.381198398376));
#51135=CARTESIAN_POINT('Origin',(477.782584437634,-92.9720072687899,380.000000551893));
#51136=CARTESIAN_POINT('',(476.449251104301,-92.9720072687899,380.000000551893));
#51137=CARTESIAN_POINT('',(477.782584437634,-95.2814083455484,380.000000551893));
#51138=CARTESIAN_POINT('',(0.,0.,0.));
#51139=CARTESIAN_POINT('Origin',(416.615917770968,-291.37200726879,403.500000551892));
#51140=CARTESIAN_POINT('',(411.615917770968,-291.37200726879,403.500000551892));
#51141=CARTESIAN_POINT('',(416.615917770968,-291.37200726879,408.500000551892));
#51142=CARTESIAN_POINT('Origin',(416.615917770968,-291.37200726879,403.500000551892));
#51143=CARTESIAN_POINT('Origin',(416.615917770968,-291.37200726879,403.500000551892));
#51144=CARTESIAN_POINT('',(411.515917770968,-291.47200726879,403.500000551892));
#51145=CARTESIAN_POINT('Origin',(411.515917770968,-291.37200726879,403.500000551892));
#51146=CARTESIAN_POINT('Origin',(416.615917770968,-291.47200726879,403.500000551892));
#51147=CARTESIAN_POINT('Origin',(416.615917770968,-274.47200726879,403.500000551892));
#51148=CARTESIAN_POINT('',(416.615917770968,-262.39218226879,398.500000551892));
#51149=CARTESIAN_POINT('',(416.615917770968,-262.39218226879,408.500000551892));
#51150=CARTESIAN_POINT('Origin',(416.615917770968,-262.39218226879,403.500000551892));
#51151=CARTESIAN_POINT('Origin',(416.615917770968,-262.39218226879,403.500000551892));
#51152=CARTESIAN_POINT('',(416.615917770968,-274.47200726879,408.500000551892));
#51153=CARTESIAN_POINT('Origin',(416.615917770968,-291.47200726879,397.000000551892));
#51154=CARTESIAN_POINT('',(416.615917770968,-291.47200726879,411.500000551892));
#51155=CARTESIAN_POINT('Origin',(416.615917770968,-291.47200726879,403.500000551892));
#51156=CARTESIAN_POINT('Origin',(416.615917770968,-261.93209476879,403.500000551892));
#51157=CARTESIAN_POINT('',(416.615917770968,-261.47200726879,399.420175551892));
#51158=CARTESIAN_POINT('',(416.615917770968,-261.93209476879,398.960088051892));
#51159=CARTESIAN_POINT('Origin',(416.615917770968,-261.47200726879,403.500000551892));
#51160=CARTESIAN_POINT('Origin',(416.615917770968,-261.47200726879,401.000000551892));
#51161=CARTESIAN_POINT('Origin',(416.615917770968,-300.47200726879,403.500000551892));
#51162=CARTESIAN_POINT('',(408.615917770968,-300.47200726879,403.500000551892));
#51163=CARTESIAN_POINT('',(416.615917770968,-300.47200726879,411.500000551892));
#51164=CARTESIAN_POINT('Origin',(416.615917770968,-300.47200726879,403.500000551892));
#51165=CARTESIAN_POINT('Origin',(416.615917770968,-300.47200726879,403.500000551892));
#51166=CARTESIAN_POINT('',(409.615917770968,-301.47200726879,403.500000551892));
#51167=CARTESIAN_POINT('Origin',(409.615917770968,-300.47200726879,403.500000551892));
#51168=CARTESIAN_POINT('Origin',(416.615917770968,-301.47200726879,403.500000551892));
#51169=CARTESIAN_POINT('Origin',(416.615917770968,-301.47200726879,397.190599475133));
#51170=CARTESIAN_POINT('',(418.925318847726,-301.47200726879,399.500000551892));
#51171=CARTESIAN_POINT('',(414.306516694209,-301.47200726879,399.500000551892));
#51172=CARTESIAN_POINT('',(415.461217232588,-301.47200726879,399.500000551892));
#51173=CARTESIAN_POINT('',(411.997115617451,-301.47200726879,403.500000551892));
#51174=CARTESIAN_POINT('',(412.57446588664,-301.47200726879,402.500000551892));
#51175=CARTESIAN_POINT('',(414.306516694209,-301.47200726879,407.500000551892));
#51176=CARTESIAN_POINT('',(413.72916642502,-301.47200726879,406.500000551892));
#51177=CARTESIAN_POINT('',(418.925318847726,-301.47200726879,407.500000551892));
#51178=CARTESIAN_POINT('',(417.770618309347,-301.47200726879,407.500000551892));
#51179=CARTESIAN_POINT('',(421.234719924485,-301.47200726879,403.500000551892));
#51180=CARTESIAN_POINT('',(420.657369655295,-301.47200726879,404.500000551892));
#51181=CARTESIAN_POINT('',(419.502669116916,-301.47200726879,400.500000551892));
#51182=CARTESIAN_POINT('Origin',(416.615917770968,-296.47200726879,403.500000551892));
#51183=CARTESIAN_POINT('',(416.615917770968,-296.47200726879,411.500000551892));
#51184=CARTESIAN_POINT('Origin',(421.234719924485,-301.47200726879,403.500000551892));
#51185=CARTESIAN_POINT('',(421.234719924485,-296.47200726879,403.500000551892));
#51186=CARTESIAN_POINT('',(418.925318847726,-296.47200726879,407.500000551892));
#51187=CARTESIAN_POINT('Ctrl Pts',(421.234719924485,-296.47200726879,403.500000551892));
#51188=CARTESIAN_POINT('Ctrl Pts',(420.080019386106,-295.805340602123,405.500000551892));
#51189=CARTESIAN_POINT('Ctrl Pts',(418.925318847726,-296.47200726879,407.500000551892));
#51190=CARTESIAN_POINT('',(421.234719924485,-298.97200726879,403.500000551892));
#51191=CARTESIAN_POINT('',(418.925318847726,-298.97200726879,407.500000551892));
#51192=CARTESIAN_POINT('Origin',(418.925318847726,-301.47200726879,399.500000551892));
#51193=CARTESIAN_POINT('',(418.925318847726,-296.47200726879,399.500000551892));
#51194=CARTESIAN_POINT('Ctrl Pts',(418.925318847726,-296.47200726879,399.500000551892));
#51195=CARTESIAN_POINT('Ctrl Pts',(420.080019386106,-295.805340602123,401.500000551892));
#51196=CARTESIAN_POINT('Ctrl Pts',(421.234719924485,-296.47200726879,403.500000551892));
#51197=CARTESIAN_POINT('',(418.925318847726,-298.97200726879,399.500000551892));
#51198=CARTESIAN_POINT('Origin',(414.306516694209,-301.47200726879,399.500000551892));
#51199=CARTESIAN_POINT('',(414.306516694209,-296.47200726879,399.500000551892));
#51200=CARTESIAN_POINT('Ctrl Pts',(414.306516694209,-296.47200726879,399.500000551892));
#51201=CARTESIAN_POINT('Ctrl Pts',(416.615917770968,-295.805340602123,399.500000551892));
#51202=CARTESIAN_POINT('Ctrl Pts',(418.925318847726,-296.47200726879,399.500000551892));
#51203=CARTESIAN_POINT('',(414.306516694209,-298.97200726879,399.500000551892));
#51204=CARTESIAN_POINT('Origin',(411.997115617451,-301.47200726879,403.500000551892));
#51205=CARTESIAN_POINT('',(411.997115617451,-296.47200726879,403.500000551892));
#51206=CARTESIAN_POINT('Ctrl Pts',(411.997115617451,-296.47200726879,403.500000551892));
#51207=CARTESIAN_POINT('Ctrl Pts',(413.15181615583,-295.805340602123,401.500000551892));
#51208=CARTESIAN_POINT('Ctrl Pts',(414.306516694209,-296.47200726879,399.500000551892));
#51209=CARTESIAN_POINT('',(411.997115617451,-298.97200726879,403.500000551892));
#51210=CARTESIAN_POINT('Origin',(418.925318847726,-301.47200726879,407.500000551892));
#51211=CARTESIAN_POINT('',(416.615917770968,-296.114741678882,407.500000551892));
#51212=CARTESIAN_POINT('Ctrl Pts',(418.925318847726,-296.47200726879,407.500000551892));
#51213=CARTESIAN_POINT('Ctrl Pts',(417.687714540692,-296.114741678882,407.500000551892));
#51214=CARTESIAN_POINT('Ctrl Pts',(416.615917770968,-296.114741678882,407.500000551892));
#51215=CARTESIAN_POINT('',(414.306516694209,-296.47200726879,407.500000551892));
#51216=CARTESIAN_POINT('',(414.306516694209,-298.97200726879,407.500000551892));
#51217=CARTESIAN_POINT('Ctrl Pts',(416.615917770968,-296.114741678882,407.500000551892));
#51218=CARTESIAN_POINT('Ctrl Pts',(415.544121001243,-296.114741678882,407.500000551892));
#51219=CARTESIAN_POINT('Ctrl Pts',(414.306516694209,-296.47200726879,407.500000551892));
#51220=CARTESIAN_POINT('Origin',(414.306516694209,-301.47200726879,407.500000551892));
#51221=CARTESIAN_POINT('Ctrl Pts',(414.306516694209,-296.47200726879,407.500000551892));
#51222=CARTESIAN_POINT('Ctrl Pts',(413.15181615583,-295.805340602123,405.500000551892));
#51223=CARTESIAN_POINT('Ctrl Pts',(411.997115617451,-296.47200726879,403.500000551892));
#51224=CARTESIAN_POINT('Origin',(416.615917770968,-295.138673935457,403.500000551892));
#51225=CARTESIAN_POINT('',(416.615917770968,-293.805340602123,403.500000551892));
#51226=CARTESIAN_POINT('',(416.615917770968,-295.138673935457,405.80940162865));
#51227=CARTESIAN_POINT('',(0.,0.,0.));
#51228=CARTESIAN_POINT('Origin',(444.115917770964,-290.472007268783,358.999900551893));
#51229=CARTESIAN_POINT('',(444.115917770964,-285.472007268783,358.999900551893));
#51230=CARTESIAN_POINT('',(449.115917770964,-290.472007268783,358.999900551893));
#51231=CARTESIAN_POINT('Origin',(444.115917770964,-290.472007268783,358.999900551893));
#51232=CARTESIAN_POINT('Origin',(444.115917770964,-290.472007268783,358.999900551893));
#51233=CARTESIAN_POINT('',(444.115917770964,-285.072007268783,359.399900551893));
#51234=CARTESIAN_POINT('Origin',(444.115917770964,-285.072007268783,358.999900551893));
#51235=CARTESIAN_POINT('Origin',(444.115917770964,-290.472007268783,359.399900551893));
#51236=CARTESIAN_POINT('Origin',(444.115917770964,-290.472007268783,344.649900551893));
#51237=CARTESIAN_POINT('',(439.115917770964,-290.472007268783,335.320175551893));
#51238=CARTESIAN_POINT('',(449.115917770964,-290.472007268783,335.320175551893));
#51239=CARTESIAN_POINT('Origin',(444.115917770964,-290.472007268783,335.320175551893));
#51240=CARTESIAN_POINT('Origin',(444.115917770964,-290.472007268783,335.320175551893));
#51241=CARTESIAN_POINT('',(449.115917770964,-290.472007268783,344.649900551893));
#51242=CARTESIAN_POINT('Origin',(437.965917770964,-290.472007268783,359.399900551893));
#51243=CARTESIAN_POINT('',(451.415917770964,-290.472007268783,359.399900551893));
#51244=CARTESIAN_POINT('Origin',(444.115917770964,-290.472007268783,359.399900551893));
#51245=CARTESIAN_POINT('Origin',(444.115917770964,-290.472007268783,334.860038051893));
#51246=CARTESIAN_POINT('',(440.036092770964,-290.472007268783,334.399900551893));
#51247=CARTESIAN_POINT('',(439.576005270964,-290.472007268783,334.860038051893));
#51248=CARTESIAN_POINT('Origin',(444.115917770964,-290.472007268783,334.399900551893));
#51249=CARTESIAN_POINT('Origin',(441.615917770964,-290.472007268783,334.399900551893));
#51250=CARTESIAN_POINT('Origin',(444.115917770964,-290.472007268783,365.672734961985));
#51251=CARTESIAN_POINT('',(437.187714540689,-286.472007268783,366.030000551893));
#51252=CARTESIAN_POINT('',(439.497115617447,-282.472007268783,365.315469372077));
#51253=CARTESIAN_POINT('Ctrl Pts',(437.187714540689,-286.472007268783,366.030000551893));
#51254=CARTESIAN_POINT('Ctrl Pts',(438.259511310413,-284.615600808232,366.030000551893));
#51255=CARTESIAN_POINT('Ctrl Pts',(439.497115617447,-282.472007268783,365.315469372077));
#51256=CARTESIAN_POINT('',(444.115917770964,-282.472007268783,366.030000551893));
#51257=CARTESIAN_POINT('Origin',(444.115917770964,-290.472007268783,366.030000551893));
#51258=CARTESIAN_POINT('Ctrl Pts',(439.497115617447,-282.472007268783,365.315469372077));
#51259=CARTESIAN_POINT('Ctrl Pts',(441.972324231515,-282.472007268783,366.030000551893));
#51260=CARTESIAN_POINT('Ctrl Pts',(444.115917770964,-282.472007268783,366.030000551893));
#51261=CARTESIAN_POINT('Origin',(444.115917770964,-290.472007268783,365.672734961985));
#51262=CARTESIAN_POINT('',(448.734719924481,-282.472007268783,365.315469372077));
#51263=CARTESIAN_POINT('',(451.04412100124,-286.472007268783,366.030000551893));
#51264=CARTESIAN_POINT('Ctrl Pts',(448.734719924481,-282.472007268783,365.315469372077));
#51265=CARTESIAN_POINT('Ctrl Pts',(449.972324231515,-284.615600808232,366.030000551893));
#51266=CARTESIAN_POINT('Ctrl Pts',(451.04412100124,-286.472007268783,366.030000551893));
#51267=CARTESIAN_POINT('Ctrl Pts',(444.115917770964,-282.472007268783,366.030000551893));
#51268=CARTESIAN_POINT('Ctrl Pts',(446.259511310413,-282.472007268783,366.030000551893));
#51269=CARTESIAN_POINT('Ctrl Pts',(448.734719924481,-282.472007268783,365.315469372077));
#51270=CARTESIAN_POINT('Origin',(444.115917770964,-290.472007268783,366.030000551893));
#51271=CARTESIAN_POINT('Origin',(444.115917770964,-290.472007268783,365.672734961985));
#51272=CARTESIAN_POINT('',(437.187714540689,-294.472007268783,366.030000551893));
#51273=CARTESIAN_POINT('',(434.87831346393,-290.472007268783,365.315469372077));
#51274=CARTESIAN_POINT('Ctrl Pts',(437.187714540689,-294.472007268783,366.030000551893));
#51275=CARTESIAN_POINT('Ctrl Pts',(436.115917770964,-292.615600808232,366.030000551893));
#51276=CARTESIAN_POINT('Ctrl Pts',(434.87831346393,-290.472007268783,365.315469372077));
#51277=CARTESIAN_POINT('Origin',(444.115917770964,-290.472007268783,366.030000551893));
#51278=CARTESIAN_POINT('Ctrl Pts',(434.87831346393,-290.472007268783,365.315469372077));
#51279=CARTESIAN_POINT('Ctrl Pts',(436.115917770964,-288.328413729334,366.030000551893));
#51280=CARTESIAN_POINT('Ctrl Pts',(437.187714540689,-286.472007268783,366.030000551893));
#51281=CARTESIAN_POINT('Origin',(444.115917770964,-290.472007268783,365.672734961985));
#51282=CARTESIAN_POINT('',(453.353522077998,-290.472007268783,365.315469372077));
#51283=CARTESIAN_POINT('',(451.04412100124,-294.472007268783,366.030000551893));
#51284=CARTESIAN_POINT('Ctrl Pts',(453.353522077998,-290.472007268783,365.315469372077));
#51285=CARTESIAN_POINT('Ctrl Pts',(452.115917770964,-292.615600808232,366.030000551893));
#51286=CARTESIAN_POINT('Ctrl Pts',(451.04412100124,-294.472007268783,366.030000551893));
#51287=CARTESIAN_POINT('Ctrl Pts',(451.04412100124,-286.472007268783,366.030000551893));
#51288=CARTESIAN_POINT('Ctrl Pts',(452.115917770964,-288.328413729334,366.030000551893));
#51289=CARTESIAN_POINT('Ctrl Pts',(453.353522077998,-290.472007268783,365.315469372077));
#51290=CARTESIAN_POINT('Origin',(444.115917770964,-290.472007268783,366.030000551893));
#51291=CARTESIAN_POINT('Origin',(444.115917770964,-290.472007268783,365.672734961985));
#51292=CARTESIAN_POINT('',(444.115917770964,-298.472007268783,366.030000551893));
#51293=CARTESIAN_POINT('',(439.497115617447,-298.472007268783,365.315469372077));
#51294=CARTESIAN_POINT('Ctrl Pts',(444.115917770964,-298.472007268783,366.030000551893));
#51295=CARTESIAN_POINT('Ctrl Pts',(441.972324231515,-298.472007268783,366.030000551893));
#51296=CARTESIAN_POINT('Ctrl Pts',(439.497115617447,-298.472007268783,365.315469372077));
#51297=CARTESIAN_POINT('Origin',(444.115917770964,-290.472007268783,366.030000551893));
#51298=CARTESIAN_POINT('Ctrl Pts',(439.497115617447,-298.472007268783,365.315469372077));
#51299=CARTESIAN_POINT('Ctrl Pts',(438.259511310413,-296.328413729334,366.030000551893));
#51300=CARTESIAN_POINT('Ctrl Pts',(437.187714540689,-294.472007268783,366.030000551893));
#51301=CARTESIAN_POINT('Origin',(444.115917770964,-290.472007268783,365.672734961985));
#51302=CARTESIAN_POINT('',(448.734719924481,-298.472007268783,365.315469372077));
#51303=CARTESIAN_POINT('Ctrl Pts',(448.734719924481,-298.472007268783,365.315469372077));
#51304=CARTESIAN_POINT('Ctrl Pts',(446.259511310413,-298.472007268783,366.030000551893));
#51305=CARTESIAN_POINT('Ctrl Pts',(444.115917770964,-298.472007268783,366.030000551893));
#51306=CARTESIAN_POINT('Ctrl Pts',(451.04412100124,-294.472007268783,366.030000551893));
#51307=CARTESIAN_POINT('Ctrl Pts',(449.972324231515,-296.328413729334,366.030000551893));
#51308=CARTESIAN_POINT('Ctrl Pts',(448.734719924481,-298.472007268783,365.315469372077));
#51309=CARTESIAN_POINT('Origin',(444.115917770964,-290.472007268783,366.030000551893));
#51310=CARTESIAN_POINT('Origin',(448.734719924481,-298.472007268783,360.000000551893));
#51311=CARTESIAN_POINT('',(439.497115617447,-298.472007268783,360.000000551893));
#51312=CARTESIAN_POINT('',(439.497115617447,-298.472007268783,360.000000551893));
#51313=CARTESIAN_POINT('',(448.734719924481,-298.472007268783,360.000000551893));
#51314=CARTESIAN_POINT('',(448.734719924481,-298.472007268783,360.000000551893));
#51315=CARTESIAN_POINT('',(448.734719924481,-298.472007268783,360.000000551893));
#51316=CARTESIAN_POINT('Origin',(439.497115617447,-298.472007268783,360.000000551893));
#51317=CARTESIAN_POINT('',(434.87831346393,-290.472007268783,360.000000551893));
#51318=CARTESIAN_POINT('',(434.87831346393,-290.472007268783,360.000000551893));
#51319=CARTESIAN_POINT('',(439.497115617447,-298.472007268783,360.000000551893));
#51320=CARTESIAN_POINT('Origin',(434.87831346393,-290.472007268783,360.000000551893));
#51321=CARTESIAN_POINT('',(439.497115617447,-282.472007268783,360.000000551893));
#51322=CARTESIAN_POINT('',(439.497115617447,-282.472007268783,360.000000551893));
#51323=CARTESIAN_POINT('',(434.87831346393,-290.472007268783,360.000000551893));
#51324=CARTESIAN_POINT('Origin',(444.115917770964,-290.472007268783,360.000000551893));
#51325=CARTESIAN_POINT('',(448.734719924481,-282.472007268783,360.000000551893));
#51326=CARTESIAN_POINT('',(439.497115617447,-282.472007268783,360.000000551893));
#51327=CARTESIAN_POINT('',(453.353522077998,-290.472007268783,360.000000551893));
#51328=CARTESIAN_POINT('',(448.734719924481,-282.472007268783,360.000000551893));
#51329=CARTESIAN_POINT('',(453.353522077998,-290.472007268783,360.000000551893));
#51330=CARTESIAN_POINT('',(451.415917770964,-290.472007268783,360.000000551893));
#51331=CARTESIAN_POINT('Origin',(444.115917770964,-290.472007268783,360.000000551893));
#51332=CARTESIAN_POINT('Origin',(439.497115617447,-282.472007268783,360.000000551893));
#51333=CARTESIAN_POINT('',(448.734719924481,-282.472007268783,360.000000551893));
#51334=CARTESIAN_POINT('Origin',(448.734719924481,-282.472007268783,360.000000551893));
#51335=CARTESIAN_POINT('',(453.353522077998,-290.472007268783,360.000000551893));
#51336=CARTESIAN_POINT('Origin',(453.353522077998,-290.472007268783,360.000000551893));
#51337=CARTESIAN_POINT('Origin',(444.115917770964,-290.472007268783,366.030000551893));
#51338=CARTESIAN_POINT('Origin',(444.115917770964,-290.472007268783,359.699950551893));
#51339=CARTESIAN_POINT('',(451.415917770964,-290.472007268783,359.699950551893));
#51340=CARTESIAN_POINT('',(0.,0.,0.));
#51341=CARTESIAN_POINT('Origin',(189.88324475895,-96.2393342567687,531.000000551894));
#51342=CARTESIAN_POINT('',(448.348590782989,-96.2393342567688,530.000000551893));
#51343=CARTESIAN_POINT('',(189.88324475895,-96.2393342567687,530.000000551894));
#51344=CARTESIAN_POINT('',(254.49958126496,-96.2393342567687,530.000000551894));
#51345=CARTESIAN_POINT('',(448.348590782989,-96.2393342567688,531.000000551893));
#51346=CARTESIAN_POINT('',(448.348590782989,-96.2393342567688,531.000000551893));
#51347=CARTESIAN_POINT('',(189.88324475895,-96.2393342567687,531.000000551894));
#51348=CARTESIAN_POINT('',(254.49958126496,-96.2393342567687,531.000000551894));
#51349=CARTESIAN_POINT('',(189.88324475895,-96.2393342567687,531.000000551894));
#51350=CARTESIAN_POINT('Origin',(189.88324475895,-264.704680280811,531.000000551894));
#51351=CARTESIAN_POINT('',(189.88324475895,-264.704680280811,530.000000551894));
#51352=CARTESIAN_POINT('',(189.88324475895,-222.5883437748,530.000000551894));
#51353=CARTESIAN_POINT('',(189.88324475895,-264.704680280811,531.000000551894));
#51354=CARTESIAN_POINT('',(189.88324475895,-222.5883437748,531.000000551894));
#51355=CARTESIAN_POINT('',(189.88324475895,-264.704680280811,531.000000551894));
#51356=CARTESIAN_POINT('Origin',(448.348590782989,-264.704680280811,531.000000551893));
#51357=CARTESIAN_POINT('',(448.348590782989,-264.704680280811,530.000000551893));
#51358=CARTESIAN_POINT('',(383.73225427698,-264.704680280811,530.000000551893));
#51359=CARTESIAN_POINT('',(448.348590782989,-264.704680280811,531.000000551893));
#51360=CARTESIAN_POINT('',(383.73225427698,-264.704680280811,531.000000551893));
#51361=CARTESIAN_POINT('',(448.348590782989,-264.704680280811,531.000000551893));
#51362=CARTESIAN_POINT('Origin',(448.348590782989,-96.2393342567688,531.000000551893));
#51363=CARTESIAN_POINT('',(448.348590782989,-138.355670762779,530.000000551893));
#51364=CARTESIAN_POINT('',(448.348590782989,-138.355670762779,531.000000551893));
#51365=CARTESIAN_POINT('Origin',(164.115917770971,-71.4379330950788,530.258819596997));
#51366=CARTESIAN_POINT('',(111.561355465157,-17.9174449629754,730.000000551894));
#51367=CARTESIAN_POINT('',(526.670480076784,-17.9174449629756,730.000000551893));
#51368=CARTESIAN_POINT('',(241.615917770971,-17.9174449629754,730.000000551894));
#51369=CARTESIAN_POINT('',(164.88324475895,-71.2393342567687,531.000000551894));
#51370=CARTESIAN_POINT('',(171.927190344623,-78.2832798424422,504.71163774041));
#51371=CARTESIAN_POINT('',(473.348590782989,-71.2393342567688,531.000000551893));
#51372=CARTESIAN_POINT('',(241.61591777097,-71.2393342567687,531.000000551894));
#51373=CARTESIAN_POINT('',(463.479467784055,-81.1084572557029,494.167932093724));
#51374=CARTESIAN_POINT('Origin',(473.149991944679,-70.4720072687899,530.258819596996));
#51375=CARTESIAN_POINT('',(526.670480076784,-343.026569574604,730.000000551893));
#51376=CARTESIAN_POINT('',(526.670480076784,-125.47200726879,730.000000551893));
#51377=CARTESIAN_POINT('',(473.348590782989,-289.704680280811,531.000000551893));
#51378=CARTESIAN_POINT('',(473.348590782989,-125.47200726879,531.000000551893));
#51379=CARTESIAN_POINT('',(466.304645197316,-282.660734695137,504.711637740409));
#51380=CARTESIAN_POINT('Origin',(474.115917770968,-289.506081442501,530.258819596995));
#51381=CARTESIAN_POINT('',(111.561355465157,-343.026569574604,730.000000551894));
#51382=CARTESIAN_POINT('',(396.61591777097,-343.026569574604,730.000000551893));
#51383=CARTESIAN_POINT('',(164.88324475895,-289.704680280811,531.000000551894));
#51384=CARTESIAN_POINT('',(396.615917770969,-289.704680280811,531.000000551893));
#51385=CARTESIAN_POINT('',(174.752367757884,-279.835557281876,494.167932093725));
#51386=CARTESIAN_POINT('Origin',(165.08184359726,-290.47200726879,530.258819596996));
#51387=CARTESIAN_POINT('',(111.561355465157,-235.47200726879,730.000000551894));
#51388=CARTESIAN_POINT('',(164.88324475895,-235.47200726879,531.000000551894));
#51389=CARTESIAN_POINT('Origin',(319.11591777097,-180.47200726879,531.000000551893));
#51390=CARTESIAN_POINT('Origin',(164.115917770971,-70.4720072687897,530.000000551894));
#51391=CARTESIAN_POINT('',(110.526079284747,-16.8821687825653,730.000000551894));
#51392=CARTESIAN_POINT('',(527.705756257194,-16.8821687825655,730.000000551893));
#51393=CARTESIAN_POINT('',(474.115917770969,-16.8821687825655,730.000000551893));
#51394=CARTESIAN_POINT('',(474.115917770968,-70.4720072687899,530.000000551893));
#51395=CARTESIAN_POINT('',(464.384751125293,-80.2031739144654,493.682792213312));
#51396=CARTESIAN_POINT('',(164.115917770971,-70.4720072687897,530.000000551894));
#51397=CARTESIAN_POINT('',(474.115917770968,-70.4720072687899,530.000000551893));
#51398=CARTESIAN_POINT('',(171.021907003386,-77.3779965012046,504.226497859998));
#51399=CARTESIAN_POINT('Origin',(474.115917770968,-70.4720072687899,530.000000551893));
#51400=CARTESIAN_POINT('',(527.705756257194,-344.061845755014,730.000000551893));
#51401=CARTESIAN_POINT('',(527.705756257194,-290.47200726879,730.000000551893));
#51402=CARTESIAN_POINT('',(474.115917770968,-290.47200726879,530.000000551893));
#51403=CARTESIAN_POINT('',(467.209928538553,-283.566018036375,504.226497859997));
#51404=CARTESIAN_POINT('',(474.115917770968,-290.47200726879,530.000000551893));
#51405=CARTESIAN_POINT('Origin',(474.115917770968,-290.47200726879,530.000000551893));
#51406=CARTESIAN_POINT('',(110.526079284747,-344.061845755014,730.000000551894));
#51407=CARTESIAN_POINT('',(164.115917770972,-344.061845755014,730.000000551894));
#51408=CARTESIAN_POINT('',(164.115917770971,-290.47200726879,530.000000551894));
#51409=CARTESIAN_POINT('',(173.847084416646,-280.740840623114,493.682792213313));
#51410=CARTESIAN_POINT('',(164.115917770971,-290.47200726879,530.000000551894));
#51411=CARTESIAN_POINT('Origin',(164.115917770971,-290.47200726879,530.000000551894));
#51412=CARTESIAN_POINT('',(110.526079284747,-70.4720072687898,730.000000551894));
#51413=CARTESIAN_POINT('',(164.115917770971,-70.4720072687897,530.000000551894));
#51414=CARTESIAN_POINT('Origin',(319.115917770971,-180.47200726879,730.000000551893));
#51415=CARTESIAN_POINT('Origin',(319.11591777097,-180.47200726879,530.000000551893));
#51416=CARTESIAN_POINT('',(0.,0.,0.));
#51417=CARTESIAN_POINT('Origin',(184.115917770964,-90.4720072687828,342.208039952213));
#51418=CARTESIAN_POINT('',(184.115917770964,-86.4720072687828,340.208039952213));
#51419=CARTESIAN_POINT('Origin',(184.115917770964,-90.4720072687828,340.208039952213));
#51420=CARTESIAN_POINT('',(184.115917770964,-86.4720072687828,338.208039952213));
#51421=CARTESIAN_POINT('',(184.115917770964,-86.4720072687828,342.208039952213));
#51422=CARTESIAN_POINT('Origin',(184.115917770964,-90.4720072687828,338.208039952213));
#51423=CARTESIAN_POINT('Origin',(454.115917770966,-90.4720072687829,342.208039952212));
#51424=CARTESIAN_POINT('',(454.115917770966,-86.4720072687829,340.208039952212));
#51425=CARTESIAN_POINT('Origin',(454.115917770966,-90.4720072687829,340.208039952212));
#51426=CARTESIAN_POINT('',(454.115917770966,-86.4720072687829,338.208039952212));
#51427=CARTESIAN_POINT('',(454.115917770966,-86.4720072687829,342.208039952212));
#51428=CARTESIAN_POINT('Origin',(454.115917770966,-90.4720072687829,338.208039952212));
#51429=CARTESIAN_POINT('Origin',(319.115917770965,-270.472007268783,342.208039952213));
#51430=CARTESIAN_POINT('',(319.115917770965,-266.472007268783,340.208039952213));
#51431=CARTESIAN_POINT('Origin',(319.115917770965,-270.472007268783,340.208039952213));
#51432=CARTESIAN_POINT('',(319.115917770965,-266.472007268783,338.208039952213));
#51433=CARTESIAN_POINT('',(319.115917770965,-266.472007268783,342.208039952213));
#51434=CARTESIAN_POINT('Origin',(319.115917770965,-270.472007268783,338.208039952213));
#51435=CARTESIAN_POINT('Origin',(184.115917770964,-270.472007268783,342.208039952213));
#51436=CARTESIAN_POINT('',(184.115917770964,-266.472007268783,340.208039952213));
#51437=CARTESIAN_POINT('Origin',(184.115917770964,-270.472007268783,340.208039952213));
#51438=CARTESIAN_POINT('',(184.115917770964,-266.472007268783,338.208039952213));
#51439=CARTESIAN_POINT('',(184.115917770964,-266.472007268783,342.208039952213));
#51440=CARTESIAN_POINT('Origin',(184.115917770964,-270.472007268783,338.208039952213));
#51441=CARTESIAN_POINT('Origin',(454.115917770966,-270.472007268783,342.208039952212));
#51442=CARTESIAN_POINT('',(454.115917770966,-266.472007268783,340.208039952212));
#51443=CARTESIAN_POINT('Origin',(454.115917770966,-270.472007268783,340.208039952212));
#51444=CARTESIAN_POINT('',(454.115917770966,-266.472007268783,338.208039952212));
#51445=CARTESIAN_POINT('',(454.115917770966,-266.472007268783,342.208039952212));
#51446=CARTESIAN_POINT('Origin',(454.115917770966,-270.472007268783,338.208039952212));
#51447=CARTESIAN_POINT('Origin',(319.115917770965,-90.4720072687829,342.208039952213));
#51448=CARTESIAN_POINT('',(319.115917770965,-86.4720072687829,340.208039952213));
#51449=CARTESIAN_POINT('Origin',(319.115917770965,-90.4720072687829,340.208039952213));
#51450=CARTESIAN_POINT('',(319.115917770965,-86.4720072687829,338.208039952213));
#51451=CARTESIAN_POINT('',(319.115917770965,-86.4720072687829,342.208039952213));
#51452=CARTESIAN_POINT('Origin',(319.115917770965,-90.4720072687829,338.208039952213));
#51453=CARTESIAN_POINT('Origin',(319.115917770966,-180.472007268783,338.208039952213));
#51454=CARTESIAN_POINT('',(174.115917770964,-280.472007268783,338.208039952213));
#51455=CARTESIAN_POINT('',(174.115917770964,-80.4720072687829,338.208039952213));
#51456=CARTESIAN_POINT('',(174.115917770964,-280.472007268783,338.208039952213));
#51457=CARTESIAN_POINT('',(464.115917770967,-80.472007268783,338.208039952212));
#51458=CARTESIAN_POINT('',(174.115917770964,-80.4720072687829,338.208039952213));
#51459=CARTESIAN_POINT('',(464.115917770967,-280.472007268783,338.208039952212));
#51460=CARTESIAN_POINT('',(464.115917770967,-80.472007268783,338.208039952212));
#51461=CARTESIAN_POINT('',(464.115917770967,-280.472007268783,338.208039952212));
#51462=CARTESIAN_POINT('',(444.115917770971,-99.3429750107207,338.208039952212));
#51463=CARTESIAN_POINT('',(444.115917770971,-260.472007268783,338.208039952212));
#51464=CARTESIAN_POINT('',(444.115917770971,-54.7220072688642,338.208039952212));
#51465=CARTESIAN_POINT('',(194.115917770964,-99.3429750107207,338.208039952213));
#51466=CARTESIAN_POINT('',(256.615917770965,-99.3429750107207,338.208039952213));
#51467=CARTESIAN_POINT('',(194.115917770964,-260.472007268783,338.208039952213));
#51468=CARTESIAN_POINT('',(194.115917770964,-55.8481659321689,338.208039952213));
#51469=CARTESIAN_POINT('',(256.615917770965,-260.472007268784,338.208039952213));
#51470=CARTESIAN_POINT('Origin',(464.115917770967,-280.472007268783,340.208039952212));
#51471=CARTESIAN_POINT('',(464.115917770967,-280.472007268783,340.208039952212));
#51472=CARTESIAN_POINT('',(174.115917770964,-280.472007268783,340.208039952213));
#51473=CARTESIAN_POINT('',(464.115917770967,-280.472007268783,340.208039952212));
#51474=CARTESIAN_POINT('',(174.115917770964,-280.472007268783,340.208039952213));
#51475=CARTESIAN_POINT('',(464.115917770967,-280.472007268783,340.208039952212));
#51476=CARTESIAN_POINT('Origin',(464.115917770967,-80.472007268783,340.208039952212));
#51477=CARTESIAN_POINT('',(464.115917770967,-80.472007268783,340.208039952212));
#51478=CARTESIAN_POINT('',(464.115917770967,-80.472007268783,340.208039952212));
#51479=CARTESIAN_POINT('',(464.115917770967,-80.472007268783,340.208039952212));
#51480=CARTESIAN_POINT('Origin',(174.115917770964,-80.4720072687829,340.208039952213));
#51481=CARTESIAN_POINT('',(174.115917770964,-80.4720072687829,340.208039952213));
#51482=CARTESIAN_POINT('',(174.115917770964,-80.4720072687829,340.208039952213));
#51483=CARTESIAN_POINT('',(174.115917770964,-80.4720072687829,340.208039952213));
#51484=CARTESIAN_POINT('Origin',(174.115917770964,-280.472007268783,340.208039952213));
#51485=CARTESIAN_POINT('',(174.115917770964,-280.472007268783,340.208039952213));
#51486=CARTESIAN_POINT('Origin',(194.115917770964,-260.472007268783,340.208039952213));
#51487=CARTESIAN_POINT('',(194.115917770963,-260.472007268898,154.208039952213));
#51488=CARTESIAN_POINT('',(194.115917770964,-260.472007268783,340.208039952213));
#51489=CARTESIAN_POINT('',(444.11591777097,-260.472007268898,154.208039952212));
#51490=CARTESIAN_POINT('',(194.115917770963,-260.472007268898,154.208039952213));
#51491=CARTESIAN_POINT('',(444.11591777097,-260.472007268869,201.958039952217));
#51492=CARTESIAN_POINT('Origin',(194.115917770963,68.7756754044452,71.1724431193512));
#51493=CARTESIAN_POINT('',(194.115917770963,4.52799273110809,154.208039952057));
#51494=CARTESIAN_POINT('',(194.115917770963,4.52799273110809,154.208039952057));
#51495=CARTESIAN_POINT('',(194.115917770963,402.527992731008,-14.7919600481777));
#51496=CARTESIAN_POINT('',(194.115917770963,402.527992731008,-14.7919600481777));
#51497=CARTESIAN_POINT('',(194.115917770962,402.527992730891,-212.791960048178));
#51498=CARTESIAN_POINT('',(194.115917770962,402.527992730891,-212.791960048178));
#51499=CARTESIAN_POINT('',(194.115917770963,-260.472007268898,154.208039952213));
#51500=CARTESIAN_POINT('Origin',(195.115917770993,-101.472007268812,340.208039952213));
#51501=CARTESIAN_POINT('',(443.115917770938,-101.472007268812,339.208039952212));
#51502=CARTESIAN_POINT('',(195.115917770993,-101.472007268812,339.208039952213));
#51503=CARTESIAN_POINT('',(194.615917770979,-101.472007268812,339.208039952213));
#51504=CARTESIAN_POINT('',(443.115917770938,-101.472007268812,340.208039952212));
#51505=CARTESIAN_POINT('',(443.115917770938,-101.472007268812,340.208039952212));
#51506=CARTESIAN_POINT('',(195.115917770993,-101.472007268812,340.208039952213));
#51507=CARTESIAN_POINT('',(194.615917770979,-101.472007268812,340.208039952213));
#51508=CARTESIAN_POINT('',(195.115917770993,-101.472007268812,340.208039952213));
#51509=CARTESIAN_POINT('Origin',(194.115917770964,-100.472007268783,339.208039952213));
#51510=CARTESIAN_POINT('',(195.115917770964,-101.055828398547,339.208039952213));
#51511=CARTESIAN_POINT('',(195.115917770964,-15.848165932169,339.208039952213));
#51512=CARTESIAN_POINT('',(443.115917770971,-101.055828398547,339.208039952212));
#51513=CARTESIAN_POINT('',(194.115917770964,-101.055828398547,339.208039952213));
#51514=CARTESIAN_POINT('',(443.115917770971,-14.7220072688642,339.208039952212));
#51515=CARTESIAN_POINT('Origin',(194.115917770964,-259.472007268783,340.208039952212));
#51516=CARTESIAN_POINT('',(443.115917770938,-259.472007268754,340.208039952212));
#51517=CARTESIAN_POINT('',(443.11591777097,-259.472007268898,154.797479056514));
#51518=CARTESIAN_POINT('',(443.11591777097,-259.472007268869,201.958039952216));
#51519=CARTESIAN_POINT('',(195.115917770963,-259.472007268898,154.797479056515));
#51520=CARTESIAN_POINT('',(194.115917770963,-259.472007268898,154.797479056515));
#51521=CARTESIAN_POINT('',(195.115917770993,-259.472007268754,340.208039952213));
#51522=CARTESIAN_POINT('',(195.115917770964,-259.472007268866,205.690241535883));
#51523=CARTESIAN_POINT('',(318.615917770951,-259.472007268754,340.208039952213));
#51524=CARTESIAN_POINT('Origin',(194.115917770963,3.6571684220111,153.716445584019));
#51525=CARTESIAN_POINT('',(443.11591777097,3.82426889735797,153.420439027688));
#51526=CARTESIAN_POINT('',(443.11591777097,31.063708173401,105.167718024321));
#51527=CARTESIAN_POINT('',(195.115917770963,3.82426889735809,153.420439027689));
#51528=CARTESIAN_POINT('',(195.115917770963,29.1938281577981,108.480076909111));
#51529=CARTESIAN_POINT('',(194.115917770963,3.82426889735811,153.420439027689));
#51530=CARTESIAN_POINT('Origin',(194.115917770963,402.137145942621,-15.7124157983407));
#51531=CARTESIAN_POINT('',(443.11591777097,402.527992731007,-15.8783783793395));
#51532=CARTESIAN_POINT('',(443.11591777097,247.586847758508,49.9132133301955));
#51533=CARTESIAN_POINT('',(195.115917770963,402.527992731007,-15.8783783793387));
#51534=CARTESIAN_POINT('',(195.115917770963,245.290036163702,50.8884926254802));
#51535=CARTESIAN_POINT('',(194.115917770963,402.527992731007,-15.8783783793387));
#51536=CARTESIAN_POINT('Origin',(194.115917770963,-259.98770942316,155.082943144922));
#51537=CARTESIAN_POINT('',(443.115917770969,402.527992730892,-211.648976449156));
#51538=CARTESIAN_POINT('',(443.11591777097,-113.940397936033,74.2392579023132));
#51539=CARTESIAN_POINT('',(195.115917770962,402.527992730892,-211.648976449155));
#51540=CARTESIAN_POINT('',(194.115917770962,402.527992730892,-211.648976449155));
#51541=CARTESIAN_POINT('',(195.115917770963,-116.383807447106,75.5917937855191));
#51542=CARTESIAN_POINT('Origin',(195.115917770963,68.7756754044452,71.1724431193512));
#51543=CARTESIAN_POINT('',(195.115917770963,402.527992730975,-70.8097584645117));
#51544=CARTESIAN_POINT('',(195.115917770993,-179.972007268768,340.208039952213));
#51545=CARTESIAN_POINT('Origin',(443.11591777097,71.027992731055,63.7080399520163));
#51546=CARTESIAN_POINT('',(443.11591777097,402.527992730972,-74.5419600481785));
#51547=CARTESIAN_POINT('',(443.115917770938,-100.972007268798,340.208039952212));
#51548=CARTESIAN_POINT('Origin',(194.115917770964,-100.472007268783,340.208039952213));
#51549=CARTESIAN_POINT('Origin',(194.115917770963,4.52799273110809,154.208039952057));
#51550=CARTESIAN_POINT('',(444.11591777097,4.52799273110797,154.208039952056));
#51551=CARTESIAN_POINT('',(444.11591777097,31.934532482498,105.659312392358));
#51552=CARTESIAN_POINT('',(194.115917770963,4.52799273110809,154.208039952057));
#51553=CARTESIAN_POINT('Origin',(194.115917770963,402.527992731008,-14.7919600481777));
#51554=CARTESIAN_POINT('',(444.11591777097,402.527992731008,-14.7919600481785));
#51555=CARTESIAN_POINT('',(444.11591777097,247.977694546895,50.8336690803584));
#51556=CARTESIAN_POINT('',(194.115917770963,402.527992731008,-14.7919600481777));
#51557=CARTESIAN_POINT('Origin',(194.115917770962,402.527992730891,-212.791960048178));
#51558=CARTESIAN_POINT('',(444.115917770969,402.527992730891,-212.791960048178));
#51559=CARTESIAN_POINT('',(444.11591777097,402.527992730972,-74.5419600481785));
#51560=CARTESIAN_POINT('',(194.115917770962,402.527992730891,-212.791960048178));
#51561=CARTESIAN_POINT('Origin',(194.115917770963,-260.472007268898,154.208039952213));
#51562=CARTESIAN_POINT('',(444.11591777097,-114.424695781772,73.3643547096032));
#51563=CARTESIAN_POINT('Origin',(444.11591777097,71.027992731055,63.7080399520163));
#51564=CARTESIAN_POINT('',(0.,0.,0.));
#51565=CARTESIAN_POINT('Ctrl Pts',(376.666251396868,288.32128221579,765.992900062209));
#51566=CARTESIAN_POINT('Ctrl Pts',(377.036265302848,287.705475663881,765.992900062209));
#51567=CARTESIAN_POINT('Ctrl Pts',(377.036265302848,287.705475663881,766.71132055189));
#51568=CARTESIAN_POINT('Ctrl Pts',(377.036265302848,287.705475663881,767.429741041571));
#51569=CARTESIAN_POINT('Ctrl Pts',(376.666251396868,288.32128221579,767.429741041571));
#51570=CARTESIAN_POINT('Ctrl Pts',(376.296237490887,288.937088767699,767.429741041571));
#51571=CARTESIAN_POINT('Ctrl Pts',(376.296237490887,288.937088767699,766.71132055189));
#51572=CARTESIAN_POINT('Ctrl Pts',(376.296237490887,288.937088767699,765.992900062209));
#51573=CARTESIAN_POINT('Ctrl Pts',(376.666251396868,288.32128221579,765.992900062209));
#51574=CARTESIAN_POINT('Ctrl Pts',(376.526601659817,288.237372188339,764.062778007165));
#51575=CARTESIAN_POINT('Ctrl Pts',(377.890701913367,285.967128124481,764.062778007165));
#51576=CARTESIAN_POINT('Ctrl Pts',(377.890701913367,285.967128124481,766.71132055189));
#51577=CARTESIAN_POINT('Ctrl Pts',(377.890701913367,285.967128124481,769.359863096615));
#51578=CARTESIAN_POINT('Ctrl Pts',(376.526601659817,288.237372188339,769.359863096615));
#51579=CARTESIAN_POINT('Ctrl Pts',(375.162501406266,290.507616252197,769.359863096615));
#51580=CARTESIAN_POINT('Ctrl Pts',(375.162501406266,290.507616252197,766.71132055189));
#51581=CARTESIAN_POINT('Ctrl Pts',(375.162501406266,290.507616252197,764.062778007165));
#51582=CARTESIAN_POINT('Ctrl Pts',(376.526601659817,288.237372188339,764.062778007165));
#51583=CARTESIAN_POINT('Ctrl Pts',(375.41696096813,287.570632795434,762.621920551886));
#51584=CARTESIAN_POINT('Ctrl Pts',(377.523157671666,284.065332835937,762.621920551886));
#51585=CARTESIAN_POINT('Ctrl Pts',(377.523157671666,284.065332835938,766.71132055189));
#51586=CARTESIAN_POINT('Ctrl Pts',(377.523157671666,284.065332835938,770.800720551895));
#51587=CARTESIAN_POINT('Ctrl Pts',(375.41696096813,287.570632795435,770.800720551895));
#51588=CARTESIAN_POINT('Ctrl Pts',(373.310764264593,291.075932754932,770.800720551895));
#51589=CARTESIAN_POINT('Ctrl Pts',(373.310764264593,291.075932754932,766.71132055189));
#51590=CARTESIAN_POINT('Ctrl Pts',(373.310764264593,291.075932754931,762.621920551885));
#51591=CARTESIAN_POINT('Ctrl Pts',(375.41696096813,287.570632795434,762.621920551886));
#51592=CARTESIAN_POINT('',(375.855511656978,288.426790399602,763.84112055189));
#51593=CARTESIAN_POINT('',(376.137009774756,288.003281767113,763.84112055189));
#51594=CARTESIAN_POINT('Ctrl Pts',(376.137009774756,288.003281767113,763.84112055189));
#51595=CARTESIAN_POINT('Ctrl Pts',(376.052798999814,288.143432032042,763.84112055189));
#51596=CARTESIAN_POINT('Ctrl Pts',(375.958586636255,288.286094900754,763.84112055189));
#51597=CARTESIAN_POINT('Ctrl Pts',(375.855511656978,288.426790399602,763.84112055189));
#51598=CARTESIAN_POINT('',(375.416960968133,287.570632795437,762.621920551891));
#51599=CARTESIAN_POINT('Ctrl Pts',(376.137009774756,288.003281767113,763.84112055189));
#51600=CARTESIAN_POINT('Ctrl Pts',(375.844583511719,287.827574341685,763.177184192262));
#51601=CARTESIAN_POINT('Ctrl Pts',(375.41696096813,287.570632795434,762.621920551886));
#51602=CARTESIAN_POINT('',(373.310764264593,291.075932754932,766.71132055189));
#51603=CARTESIAN_POINT('Origin',(375.416960968131,287.570632795441,766.71132055189));
#51604=CARTESIAN_POINT('Origin',(375.416960968131,287.570632795441,766.71132055189));
#51605=CARTESIAN_POINT('',(376.378790341087,287.555908422089,763.84112055189));
#51606=CARTESIAN_POINT('Ctrl Pts',(376.378790341087,287.555908422089,763.84112055189));
#51607=CARTESIAN_POINT('Ctrl Pts',(376.302954360659,287.712970762643,763.84112055189));
#51608=CARTESIAN_POINT('Ctrl Pts',(376.221220549696,287.863131502187,763.84112055189));
#51609=CARTESIAN_POINT('Ctrl Pts',(376.137009774756,288.003281767113,763.84112055189));
#51610=CARTESIAN_POINT('',(376.927890738919,287.885841227039,766.20332055189));
#51611=CARTESIAN_POINT('Ctrl Pts',(376.378790341087,287.555908422089,763.84112055189));
#51612=CARTESIAN_POINT('Ctrl Pts',(376.413152024135,287.576555004236,763.918679595973));
#51613=CARTESIAN_POINT('Ctrl Pts',(376.445439414504,287.595955225601,763.995893204523));
#51614=CARTESIAN_POINT('Ctrl Pts',(376.629084043068,287.7063000508,764.460067136705));
#51615=CARTESIAN_POINT('Ctrl Pts',(376.756707472439,287.782983943575,764.903522004224));
#51616=CARTESIAN_POINT('Ctrl Pts',(376.88357350055,287.859212743759,765.639972564748));
#51617=CARTESIAN_POINT('Ctrl Pts',(376.913676025362,287.877300165452,765.925478638303));
#51618=CARTESIAN_POINT('Ctrl Pts',(376.927890738919,287.885841227039,766.20332055189));
#51619=CARTESIAN_POINT('',(377.59541328164,285.531107824361,766.20332055189));
#51620=CARTESIAN_POINT('Ctrl Pts',(376.927890738919,287.885841227039,766.20332055189));
#51621=CARTESIAN_POINT('Ctrl Pts',(377.056775189666,287.639143162358,766.20332055189));
#51622=CARTESIAN_POINT('Ctrl Pts',(377.173719163355,287.37632927026,766.20332055189));
#51623=CARTESIAN_POINT('Ctrl Pts',(377.426153214203,286.668839131006,766.20332055189));
#51624=CARTESIAN_POINT('Ctrl Pts',(377.526925926107,286.212040226457,766.20332055189));
#51625=CARTESIAN_POINT('Ctrl Pts',(377.582348545998,285.703820684751,766.20332055189));
#51626=CARTESIAN_POINT('Ctrl Pts',(377.589829103932,285.618235482969,766.20332055189));
#51627=CARTESIAN_POINT('Ctrl Pts',(377.59541328164,285.531107824361,766.20332055189));
#51628=CARTESIAN_POINT('',(377.59541328164,285.531107824371,767.21932055189));
#51629=CARTESIAN_POINT('Ctrl Pts',(377.59541328164,285.531107824371,766.20332055189));
#51630=CARTESIAN_POINT('Ctrl Pts',(377.609032781063,285.539291245225,766.377007671755));
#51631=CARTESIAN_POINT('Ctrl Pts',(377.615272057358,285.543040180642,766.547816572197));
#51632=CARTESIAN_POINT('Ctrl Pts',(377.615272057358,285.543040180642,766.71132055189));
#51633=CARTESIAN_POINT('Ctrl Pts',(377.615272057358,285.543040180642,766.874824531583));
#51634=CARTESIAN_POINT('Ctrl Pts',(377.609032781063,285.539291245225,767.045633432026));
#51635=CARTESIAN_POINT('Ctrl Pts',(377.59541328164,285.531107824371,767.21932055189));
#51636=CARTESIAN_POINT('',(376.927890738919,287.885841227039,767.21932055189));
#51637=CARTESIAN_POINT('Ctrl Pts',(377.59541328164,285.531107824371,767.21932055189));
#51638=CARTESIAN_POINT('Ctrl Pts',(377.589829103932,285.618235482975,767.21932055189));
#51639=CARTESIAN_POINT('Ctrl Pts',(377.582348545998,285.703820684754,767.219320551891));
#51640=CARTESIAN_POINT('Ctrl Pts',(377.526925926107,286.212040226456,767.21932055189));
#51641=CARTESIAN_POINT('Ctrl Pts',(377.426153214203,286.668839131006,767.21932055189));
#51642=CARTESIAN_POINT('Ctrl Pts',(377.173719163355,287.37632927026,767.21932055189));
#51643=CARTESIAN_POINT('Ctrl Pts',(377.056775189666,287.639143162358,767.21932055189));
#51644=CARTESIAN_POINT('Ctrl Pts',(376.927890738919,287.885841227039,767.21932055189));
#51645=CARTESIAN_POINT('',(376.378790341087,287.555908422089,769.58152055189));
#51646=CARTESIAN_POINT('Ctrl Pts',(376.927890738919,287.885841227039,767.21932055189));
#51647=CARTESIAN_POINT('Ctrl Pts',(376.913676025362,287.877300165452,767.497162465477));
#51648=CARTESIAN_POINT('Ctrl Pts',(376.88357350055,287.859212743759,767.782668539032));
#51649=CARTESIAN_POINT('Ctrl Pts',(376.75670747244,287.782983943575,768.519119099557));
#51650=CARTESIAN_POINT('Ctrl Pts',(376.629084043068,287.7063000508,768.962573967075));
#51651=CARTESIAN_POINT('Ctrl Pts',(376.445439414505,287.595955225601,769.426747899258));
#51652=CARTESIAN_POINT('Ctrl Pts',(376.413152024135,287.576555004236,769.503961507808));
#51653=CARTESIAN_POINT('Ctrl Pts',(376.378790341087,287.555908422089,769.58152055189));
#51654=CARTESIAN_POINT('',(375.855511656978,288.426790399603,769.58152055189));
#51655=CARTESIAN_POINT('Ctrl Pts',(376.378790341087,287.555908422089,769.58152055189));
#51656=CARTESIAN_POINT('Ctrl Pts',(376.302954360659,287.712970762643,769.58152055189));
#51657=CARTESIAN_POINT('Ctrl Pts',(376.221220549696,287.863131502187,769.58152055189));
#51658=CARTESIAN_POINT('Ctrl Pts',(376.137009774756,288.003281767113,769.58152055189));
#51659=CARTESIAN_POINT('Ctrl Pts',(376.052798999814,288.143432032043,769.58152055189));
#51660=CARTESIAN_POINT('Ctrl Pts',(375.958586636254,288.286094900754,769.58152055189));
#51661=CARTESIAN_POINT('Ctrl Pts',(375.855511656978,288.426790399602,769.58152055189));
#51662=CARTESIAN_POINT('',(376.40461205481,288.756723204552,767.21932055189));
#51663=CARTESIAN_POINT('Ctrl Pts',(375.855511656978,288.426790399602,769.58152055189));
#51664=CARTESIAN_POINT('Ctrl Pts',(375.889873340025,288.447436981749,769.50396150781));
#51665=CARTESIAN_POINT('Ctrl Pts',(375.922160730394,288.466837203112,769.426747899263));
#51666=CARTESIAN_POINT('Ctrl Pts',(376.105805358957,288.577182028312,768.962573967082));
#51667=CARTESIAN_POINT('Ctrl Pts',(376.23342878833,288.653865921087,768.519119099562));
#51668=CARTESIAN_POINT('Ctrl Pts',(376.360294816442,288.730094721272,767.782668539035));
#51669=CARTESIAN_POINT('Ctrl Pts',(376.390397341253,288.748182142965,767.497162465479));
#51670=CARTESIAN_POINT('Ctrl Pts',(376.40461205481,288.756723204552,767.21932055189));
#51671=CARTESIAN_POINT('',(374.638888716418,290.451590997326,767.21932055189));
#51672=CARTESIAN_POINT('Ctrl Pts',(376.40461205481,288.756723204552,767.21932055189));
#51673=CARTESIAN_POINT('Ctrl Pts',(376.247298176951,288.986339146055,767.21932055189));
#51674=CARTESIAN_POINT('Ctrl Pts',(376.070149153641,289.212978194765,767.21932055189));
#51675=CARTESIAN_POINT('Ctrl Pts',(375.563983046572,289.768010733646,767.21932055189));
#51676=CARTESIAN_POINT('Ctrl Pts',(375.207963475924,290.071441852646,767.21932055189));
#51677=CARTESIAN_POINT('Ctrl Pts',(374.785251598902,290.358971743954,767.21932055189));
#51678=CARTESIAN_POINT('Ctrl Pts',(374.713196260225,290.40575650301,767.21932055189));
#51679=CARTESIAN_POINT('Ctrl Pts',(374.638888716418,290.451590997326,767.21932055189));
#51680=CARTESIAN_POINT('',(374.638888716425,290.451590997321,766.20332055189));
#51681=CARTESIAN_POINT('Ctrl Pts',(374.638888716425,290.451590997321,767.219320551891));
#51682=CARTESIAN_POINT('Ctrl Pts',(374.652508215849,290.459774418175,767.045633432026));
#51683=CARTESIAN_POINT('Ctrl Pts',(374.658747492148,290.463523353594,766.874824531583));
#51684=CARTESIAN_POINT('Ctrl Pts',(374.658747492148,290.463523353594,766.71132055189));
#51685=CARTESIAN_POINT('Ctrl Pts',(374.658747492147,290.463523353594,766.547816572197));
#51686=CARTESIAN_POINT('Ctrl Pts',(374.652508215849,290.459774418175,766.377007671755));
#51687=CARTESIAN_POINT('Ctrl Pts',(374.638888716425,290.451590997321,766.20332055189));
#51688=CARTESIAN_POINT('',(376.40461205481,288.756723204552,766.20332055189));
#51689=CARTESIAN_POINT('Ctrl Pts',(374.638888716425,290.451590997321,766.20332055189));
#51690=CARTESIAN_POINT('Ctrl Pts',(374.71319626023,290.405756503006,766.20332055189));
#51691=CARTESIAN_POINT('Ctrl Pts',(374.785251598905,290.358971743952,766.20332055189));
#51692=CARTESIAN_POINT('Ctrl Pts',(375.207963475924,290.071441852646,766.20332055189));
#51693=CARTESIAN_POINT('Ctrl Pts',(375.563983046572,289.768010733645,766.20332055189));
#51694=CARTESIAN_POINT('Ctrl Pts',(376.070149153641,289.212978194765,766.20332055189));
#51695=CARTESIAN_POINT('Ctrl Pts',(376.247298176951,288.986339146055,766.20332055189));
#51696=CARTESIAN_POINT('Ctrl Pts',(376.40461205481,288.756723204552,766.20332055189));
#51697=CARTESIAN_POINT('Ctrl Pts',(376.40461205481,288.756723204552,766.20332055189));
#51698=CARTESIAN_POINT('Ctrl Pts',(376.390397341253,288.748182142965,765.925478638302));
#51699=CARTESIAN_POINT('Ctrl Pts',(376.360294816441,288.730094721272,765.639972564745));
#51700=CARTESIAN_POINT('Ctrl Pts',(376.233428788329,288.653865921087,764.903522004218));
#51701=CARTESIAN_POINT('Ctrl Pts',(376.105805358957,288.577182028312,764.460067136698));
#51702=CARTESIAN_POINT('Ctrl Pts',(375.922160730393,288.466837203112,763.995893204517));
#51703=CARTESIAN_POINT('Ctrl Pts',(375.889873340025,288.447436981749,763.91867959597));
#51704=CARTESIAN_POINT('Ctrl Pts',(375.855511656978,288.426790399602,763.841120551891));
#51705=CARTESIAN_POINT('Origin',(376.179793757718,284.535548590652,766.20332055189));
#51706=CARTESIAN_POINT('',(374.764174233796,286.58574918837,766.20332055189));
#51707=CARTESIAN_POINT('',(374.764174233796,286.58574918837,766.20332055189));
#51708=CARTESIAN_POINT('',(375.980797174348,284.560948590652,766.20332055189));
#51709=CARTESIAN_POINT('',(375.980797174348,284.560948590652,766.20332055189));
#51710=CARTESIAN_POINT('',(375.980797174348,284.560948590652,766.20332055189));
#51711=CARTESIAN_POINT('Origin',(376.798034615854,285.051994385647,767.24472055189));
#51712=CARTESIAN_POINT('',(375.980797174348,284.560948590652,767.21932055189));
#51713=CARTESIAN_POINT('',(375.980797174348,284.560948590652,767.21932055189));
#51714=CARTESIAN_POINT('',(375.980797174348,284.560948590652,767.21932055189));
#51715=CARTESIAN_POINT('Origin',(376.179793757718,284.535548590652,767.21932055189));
#51716=CARTESIAN_POINT('',(374.764174233796,286.58574918837,767.21932055189));
#51717=CARTESIAN_POINT('',(374.764174233796,286.58574918837,767.21932055189));
#51718=CARTESIAN_POINT('',(374.764174233796,286.58574918837,767.21932055189));
#51719=CARTESIAN_POINT('Origin',(374.401714623305,284.575195940938,770.826120551892));
#51720=CARTESIAN_POINT('',(373.348616271536,286.327845920685,762.621920551891));
#51721=CARTESIAN_POINT('',(373.348616271535,286.327845920685,770.80072055189));
#51722=CARTESIAN_POINT('Origin',(373.348616271537,286.327845920682,766.711320551889));
#51723=CARTESIAN_POINT('',(373.348616271535,286.327845920685,770.80072055189));
#51724=CARTESIAN_POINT('Origin',(374.382788619834,286.949239358062,766.71132055189));
#51725=CARTESIAN_POINT('',(371.369430483558,289.90946173752,766.71132055189));
#51726=CARTESIAN_POINT('',(372.276591916296,290.454539317553,766.71132055189));
#51727=CARTESIAN_POINT('Ctrl Pts',(371.369430483558,289.90946173752,766.71132055189));
#51728=CARTESIAN_POINT('Ctrl Pts',(371.369430483558,289.90946173752,767.22482239764));
#51729=CARTESIAN_POINT('Ctrl Pts',(371.421402056011,289.820956939152,767.772546668437));
#51730=CARTESIAN_POINT('Ctrl Pts',(371.630749600074,289.459840243892,768.780098710948));
#51731=CARTESIAN_POINT('Ctrl Pts',(371.787896241397,289.187090160201,769.239924587226));
#51732=CARTESIAN_POINT('Ctrl Pts',(372.145703739212,288.554675965553,769.966293840242));
#51733=CARTESIAN_POINT('Ctrl Pts',(372.370204407377,288.152775767151,770.281075771311));
#51734=CARTESIAN_POINT('Ctrl Pts',(372.852983973292,287.267271061198,770.698283099487));
#51735=CARTESIAN_POINT('Ctrl Pts',(373.111025024257,286.783542579163,770.80072055189));
#51736=CARTESIAN_POINT('Ctrl Pts',(373.348616271537,286.327845920683,770.80072055189));
#51737=CARTESIAN_POINT('Ctrl Pts',(373.348616271537,286.327845920683,762.621920551891));
#51738=CARTESIAN_POINT('Ctrl Pts',(373.111002505848,286.783585769154,762.621920551891));
#51739=CARTESIAN_POINT('Ctrl Pts',(372.852938079792,287.267356915581,762.724377271566));
#51740=CARTESIAN_POINT('Ctrl Pts',(372.370121550201,288.152926064257,763.141657334098));
#51741=CARTESIAN_POINT('Ctrl Pts',(372.145607374458,288.554848085829,763.456492730614));
#51742=CARTESIAN_POINT('Ctrl Pts',(371.78782380032,289.18721640002,764.1829137133));
#51743=CARTESIAN_POINT('Ctrl Pts',(371.630703535562,289.459919977806,764.642713966332));
#51744=CARTESIAN_POINT('Ctrl Pts',(371.42139225148,289.820973577177,765.650191762871));
#51745=CARTESIAN_POINT('Ctrl Pts',(371.369430483558,289.90946173752,766.197867412043));
#51746=CARTESIAN_POINT('Ctrl Pts',(371.369430483558,289.90946173752,766.71132055189));
#51747=CARTESIAN_POINT('Origin',(298.461074890948,247.282959303209,725.690320551891));
#51748=CARTESIAN_POINT('',(373.885000951849,285.281359303215,668.66732055189));
#51749=CARTESIAN_POINT('',(376.030529085239,280.683959303215,668.66732055189));
#51750=CARTESIAN_POINT('Origin',(298.461074890937,247.282959303203,668.667320551891));
#51751=CARTESIAN_POINT('',(371.253366994166,290.107359303215,673.49332055189));
#51752=CARTESIAN_POINT('Ctrl Pts',(373.885000951849,285.281359303215,668.66732055189));
#51753=CARTESIAN_POINT('Ctrl Pts',(373.583544656744,285.879727058503,668.66732055189));
#51754=CARTESIAN_POINT('Ctrl Pts',(373.251819248658,286.518714453873,668.784753798678));
#51755=CARTESIAN_POINT('Ctrl Pts',(372.617063345922,287.705592815822,669.271384941794));
#51756=CARTESIAN_POINT('Ctrl Pts',(372.314344533015,288.253640500934,669.640607097597));
#51757=CARTESIAN_POINT('Ctrl Pts',(371.835180640332,289.105328074275,670.492294670938));
#51758=CARTESIAN_POINT('Ctrl Pts',(371.621425700037,289.4764915362,671.022230122432));
#51759=CARTESIAN_POINT('Ctrl Pts',(371.329992690801,289.977829161081,672.209345568074));
#51760=CARTESIAN_POINT('Ctrl Pts',(371.253366994166,290.107359303215,672.867055516681));
#51761=CARTESIAN_POINT('Ctrl Pts',(371.253366994166,290.107359303215,673.49332055189));
#51762=CARTESIAN_POINT('',(371.253366994166,290.107359303215,682.38332055189));
#51763=CARTESIAN_POINT('',(371.253366994166,290.107359303215,673.49332055189));
#51764=CARTESIAN_POINT('',(373.204954482258,286.602159303215,682.38332055189));
#51765=CARTESIAN_POINT('Origin',(298.461074890986,247.282959303229,682.383320551859));
#51766=CARTESIAN_POINT('',(373.204954482258,286.602159303215,686.95532055189));
#51767=CARTESIAN_POINT('Ctrl Pts',(373.204954482258,286.602159303215,686.95532055189));
#51768=CARTESIAN_POINT('Ctrl Pts',(373.356056756597,286.314921256684,686.95532055189));
#51769=CARTESIAN_POINT('Ctrl Pts',(373.5165937577,286.005315992971,686.898068801918));
#51770=CARTESIAN_POINT('Ctrl Pts',(373.811233600901,285.428803143283,686.655970009764));
#51771=CARTESIAN_POINT('Ctrl Pts',(373.945390667172,285.16199362503,686.470955471717));
#51772=CARTESIAN_POINT('Ctrl Pts',(374.143919780962,284.763585698954,686.05428890552));
#51773=CARTESIAN_POINT('Ctrl Pts',(374.226119215438,284.596772075588,685.806126998833));
#51774=CARTESIAN_POINT('Ctrl Pts',(374.335942776093,284.372944317345,685.256268174833));
#51775=CARTESIAN_POINT('Ctrl Pts',(374.363572364748,284.316159303215,684.954479109466));
#51776=CARTESIAN_POINT('Ctrl Pts',(374.363572364748,284.316159303215,684.384161994314));
#51777=CARTESIAN_POINT('Ctrl Pts',(374.335942776093,284.372944317345,684.082372928947));
#51778=CARTESIAN_POINT('Ctrl Pts',(374.226119215438,284.596772075588,683.532514104947));
#51779=CARTESIAN_POINT('Ctrl Pts',(374.143919780962,284.763585698954,683.28435219826));
#51780=CARTESIAN_POINT('Ctrl Pts',(373.945390667172,285.16199362503,682.867685632063));
#51781=CARTESIAN_POINT('Ctrl Pts',(373.811233600901,285.428803143283,682.682671094016));
#51782=CARTESIAN_POINT('Ctrl Pts',(373.5165937577,286.005315992971,682.440572301862));
#51783=CARTESIAN_POINT('Ctrl Pts',(373.356056756597,286.314921256684,682.38332055189));
#51784=CARTESIAN_POINT('Ctrl Pts',(373.204954482258,286.602159303215,682.38332055189));
#51785=CARTESIAN_POINT('',(371.253366994166,290.107359303215,686.95532055189));
#51786=CARTESIAN_POINT('Origin',(298.461074891001,247.282959303238,686.955320551891));
#51787=CARTESIAN_POINT('',(371.253366994166,290.107359303216,777.88732055189));
#51788=CARTESIAN_POINT('',(371.253366994166,290.107359303215,686.95532055189));
#51789=CARTESIAN_POINT('',(373.885000951849,285.281359303216,782.71332055189));
#51790=CARTESIAN_POINT('Ctrl Pts',(371.253366994166,290.107359303216,777.88732055189));
#51791=CARTESIAN_POINT('Ctrl Pts',(371.253366994166,290.107359303216,778.491450416375));
#51792=CARTESIAN_POINT('Ctrl Pts',(371.32472905797,289.986693795228,779.128069862876));
#51793=CARTESIAN_POINT('Ctrl Pts',(371.59833518068,289.516384392817,780.284025646316));
#51794=CARTESIAN_POINT('Ctrl Pts',(371.799607321366,289.167384391968,780.803853655814));
#51795=CARTESIAN_POINT('Ctrl Pts',(372.269123915821,288.335111563991,781.679535597245));
#51796=CARTESIAN_POINT('Ctrl Pts',(372.578867361069,287.775884973468,782.071237654018));
#51797=CARTESIAN_POINT('Ctrl Pts',(373.231303497597,286.5581054402,782.588143904945));
#51798=CARTESIAN_POINT('Ctrl Pts',(373.57365469508,285.899357878152,782.71332055189));
#51799=CARTESIAN_POINT('Ctrl Pts',(373.885000951849,285.281359303216,782.713320551891));
#51800=CARTESIAN_POINT('',(376.03052908524,280.683959303216,782.713320551891));
#51801=CARTESIAN_POINT('Origin',(298.46107489093,247.282959303201,782.71332055193));
#51802=CARTESIAN_POINT('',(376.030529085239,280.683959303215,668.66732055189));
#51803=CARTESIAN_POINT('',(373.348616271535,286.327845920684,721.60092055189));
#51804=CARTESIAN_POINT('',(371.369430483558,289.909461737519,725.69032055189));
#51805=CARTESIAN_POINT('Ctrl Pts',(373.348616271537,286.327845920682,721.60092055189));
#51806=CARTESIAN_POINT('Ctrl Pts',(373.111025024257,286.783542579163,721.60092055189));
#51807=CARTESIAN_POINT('Ctrl Pts',(372.852983973291,287.267271061198,721.703358004293));
#51808=CARTESIAN_POINT('Ctrl Pts',(372.370204407376,288.152775767151,722.120565332469));
#51809=CARTESIAN_POINT('Ctrl Pts',(372.145703739212,288.554675965552,722.435347263539));
#51810=CARTESIAN_POINT('Ctrl Pts',(371.787896241397,289.187090160201,723.161716516554));
#51811=CARTESIAN_POINT('Ctrl Pts',(371.630749600074,289.459840243892,723.621542392832));
#51812=CARTESIAN_POINT('Ctrl Pts',(371.421402056011,289.820956939152,724.629094435343));
#51813=CARTESIAN_POINT('Ctrl Pts',(371.369430483558,289.909461737519,725.17681870614));
#51814=CARTESIAN_POINT('Ctrl Pts',(371.369430483558,289.909461737519,725.69032055189));
#51815=CARTESIAN_POINT('',(373.348616271535,286.327845920685,729.77972055189));
#51816=CARTESIAN_POINT('',(373.348616271535,286.327845920685,729.77972055189));
#51817=CARTESIAN_POINT('Ctrl Pts',(371.369430483558,289.909461737519,725.69032055189));
#51818=CARTESIAN_POINT('Ctrl Pts',(371.369430483558,289.909461737519,726.203773691737));
#51819=CARTESIAN_POINT('Ctrl Pts',(371.42139225148,289.820973577177,726.751449340909));
#51820=CARTESIAN_POINT('Ctrl Pts',(371.630703535562,289.459919977806,727.758927137448));
#51821=CARTESIAN_POINT('Ctrl Pts',(371.78782380032,289.18721640002,728.218727390481));
#51822=CARTESIAN_POINT('Ctrl Pts',(372.145607374458,288.554848085829,728.945148373167));
#51823=CARTESIAN_POINT('Ctrl Pts',(372.3701215502,288.152926064257,729.259983769682));
#51824=CARTESIAN_POINT('Ctrl Pts',(372.852938079792,287.267356915581,729.677263832215));
#51825=CARTESIAN_POINT('Ctrl Pts',(373.111002505848,286.783585769154,729.77972055189));
#51826=CARTESIAN_POINT('Ctrl Pts',(373.348616271537,286.327845920682,729.77972055189));
#51827=CARTESIAN_POINT('Origin',(372.921059816465,286.602159303215,684.66932055189));
#51828=CARTESIAN_POINT('',(371.478547268182,286.602159303215,686.95532055189));
#51829=CARTESIAN_POINT('',(371.478547268182,286.602159303215,686.95532055189));
#51830=CARTESIAN_POINT('',(371.478547268182,286.602159303215,682.38332055189));
#51831=CARTESIAN_POINT('',(371.478547268182,286.602159303215,682.38332055189));
#51832=CARTESIAN_POINT('Ctrl Pts',(371.478547268183,286.602159303215,686.95532055189));
#51833=CARTESIAN_POINT('Ctrl Pts',(371.633224281162,286.314917331796,686.95532055189));
#51834=CARTESIAN_POINT('Ctrl Pts',(371.797603768875,286.005179180258,686.898077083466));
#51835=CARTESIAN_POINT('Ctrl Pts',(372.099402285304,285.428123066717,686.655618593454));
#51836=CARTESIAN_POINT('Ctrl Pts',(372.236875981077,285.160905498426,686.470232722809));
#51837=CARTESIAN_POINT('Ctrl Pts',(372.439838261473,284.762777340855,686.053077926653));
#51838=CARTESIAN_POINT('Ctrl Pts',(372.523732972395,284.596349167931,685.805291976824));
#51839=CARTESIAN_POINT('Ctrl Pts',(372.635876555797,284.372919981108,685.256004081802));
#51840=CARTESIAN_POINT('Ctrl Pts',(372.664126437096,284.316159303215,684.954404613746));
#51841=CARTESIAN_POINT('Ctrl Pts',(372.664126437096,284.316159303215,684.66932055189));
#51842=CARTESIAN_POINT('Ctrl Pts',(372.664126437096,284.316159303215,684.384236490034));
#51843=CARTESIAN_POINT('Ctrl Pts',(372.635876555797,284.372919981108,684.082637021978));
#51844=CARTESIAN_POINT('Ctrl Pts',(372.523732972394,284.596349167931,683.533349126956));
#51845=CARTESIAN_POINT('Ctrl Pts',(372.439838261473,284.762777340855,683.285563177128));
#51846=CARTESIAN_POINT('Ctrl Pts',(372.236875981077,285.160905498426,682.868408380971));
#51847=CARTESIAN_POINT('Ctrl Pts',(372.099402285304,285.428123066717,682.683022510327));
#51848=CARTESIAN_POINT('Ctrl Pts',(371.797603768875,286.005179180258,682.440564020314));
#51849=CARTESIAN_POINT('Ctrl Pts',(371.633224281162,286.314917331796,682.38332055189));
#51850=CARTESIAN_POINT('Ctrl Pts',(371.478547268183,286.602159303215,682.38332055189));
#51851=CARTESIAN_POINT('Origin',(372.92105981647,207.963759303215,684.669320551891));
#51852=CARTESIAN_POINT('',(373.204954482263,207.963759303215,682.383320551891));
#51853=CARTESIAN_POINT('',(373.204954482263,207.963759303215,686.955320551891));
#51854=CARTESIAN_POINT('Ctrl Pts',(373.204954482263,207.963759303215,682.383320551891));
#51855=CARTESIAN_POINT('Ctrl Pts',(373.356056756602,208.250997349746,682.383320551891));
#51856=CARTESIAN_POINT('Ctrl Pts',(373.516593757705,208.56060261346,682.440572301862));
#51857=CARTESIAN_POINT('Ctrl Pts',(373.811233600906,209.137115463147,682.682671094017));
#51858=CARTESIAN_POINT('Ctrl Pts',(373.945390667178,209.4039249814,682.867685632064));
#51859=CARTESIAN_POINT('Ctrl Pts',(374.143919780967,209.802332907476,683.284352198261));
#51860=CARTESIAN_POINT('Ctrl Pts',(374.226119215443,209.969146530842,683.532514104947));
#51861=CARTESIAN_POINT('Ctrl Pts',(374.335942776098,210.192974289085,684.082372928948));
#51862=CARTESIAN_POINT('Ctrl Pts',(374.363572364753,210.249759303215,684.384161994315));
#51863=CARTESIAN_POINT('Ctrl Pts',(374.363572364753,210.249759303215,684.669320551891));
#51864=CARTESIAN_POINT('Ctrl Pts',(374.363572364753,210.249759303215,684.963578716553));
#51865=CARTESIAN_POINT('Ctrl Pts',(374.334175826209,210.189334883116,685.274176295822));
#51866=CARTESIAN_POINT('Ctrl Pts',(374.217956550179,209.952552131374,685.837113369052));
#51867=CARTESIAN_POINT('Ctrl Pts',(374.131115433866,209.776425542292,686.089546516399));
#51868=CARTESIAN_POINT('Ctrl Pts',(373.928262808842,209.369823722155,686.496148336535));
#51869=CARTESIAN_POINT('Ctrl Pts',(373.796344294332,209.107779573834,686.671708057868));
#51870=CARTESIAN_POINT('Ctrl Pts',(373.508153846187,208.544308012748,686.901203447376));
#51871=CARTESIAN_POINT('Ctrl Pts',(373.351837700045,208.24297712921,686.955320551891));
#51872=CARTESIAN_POINT('Ctrl Pts',(373.204954482263,207.963759303215,686.955320551891));
#51873=CARTESIAN_POINT('',(371.478547268188,207.963759303215,686.955320551891));
#51874=CARTESIAN_POINT('',(371.478547268188,207.963759303215,686.955320551891));
#51875=CARTESIAN_POINT('',(371.478547268188,207.963759303215,682.383320551891));
#51876=CARTESIAN_POINT('Ctrl Pts',(371.478547268188,207.963759303215,682.383320551891));
#51877=CARTESIAN_POINT('Ctrl Pts',(371.633224281167,208.251001274634,682.383320551891));
#51878=CARTESIAN_POINT('Ctrl Pts',(371.79760376888,208.560739426172,682.440564020315));
#51879=CARTESIAN_POINT('Ctrl Pts',(372.099402285309,209.137795539713,682.683022510327));
#51880=CARTESIAN_POINT('Ctrl Pts',(372.236875981082,209.405013108004,682.868408380972));
#51881=CARTESIAN_POINT('Ctrl Pts',(372.439838261478,209.803141265575,683.285563177128));
#51882=CARTESIAN_POINT('Ctrl Pts',(372.5237329724,209.969569438499,683.533349126957));
#51883=CARTESIAN_POINT('Ctrl Pts',(372.635876555802,210.192998625322,684.082637021979));
#51884=CARTESIAN_POINT('Ctrl Pts',(372.664126437101,210.249759303215,684.384236490035));
#51885=CARTESIAN_POINT('Ctrl Pts',(372.664126437101,210.249759303215,684.954404613747));
#51886=CARTESIAN_POINT('Ctrl Pts',(372.635876555802,210.192998625322,685.256004081803));
#51887=CARTESIAN_POINT('Ctrl Pts',(372.5237329724,209.969569438499,685.805291976825));
#51888=CARTESIAN_POINT('Ctrl Pts',(372.439838261478,209.803141265575,686.053077926653));
#51889=CARTESIAN_POINT('Ctrl Pts',(372.236875981082,209.405013108004,686.470232722809));
#51890=CARTESIAN_POINT('Ctrl Pts',(372.099402285309,209.137795539713,686.655618593454));
#51891=CARTESIAN_POINT('Ctrl Pts',(371.79760376888,208.560739426172,686.898077083467));
#51892=CARTESIAN_POINT('Ctrl Pts',(371.633224281167,208.251001274634,686.955320551891));
#51893=CARTESIAN_POINT('Ctrl Pts',(371.478547268188,207.963759303215,686.955320551891));
#51894=CARTESIAN_POINT('',(371.478547268188,207.963759303215,682.383320551891));
#51895=CARTESIAN_POINT('Origin',(371.682267445713,209.284559303216,777.887320551891));
#51896=CARTESIAN_POINT('',(373.885000951854,209.284559303216,782.713320551891));
#51897=CARTESIAN_POINT('',(372.174522500194,209.284559303216,782.713320551891));
#51898=CARTESIAN_POINT('',(373.885000951854,209.284559303216,782.713320551891));
#51899=CARTESIAN_POINT('',(369.479533939571,204.458559303216,777.887320551891));
#51900=CARTESIAN_POINT('Ctrl Pts',(369.479533939572,204.458559303216,777.887320551891));
#51901=CARTESIAN_POINT('Ctrl Pts',(369.479533939572,204.458559303216,778.491422612331));
#51902=CARTESIAN_POINT('Ctrl Pts',(369.552676414562,204.579217013025,779.127610628061));
#51903=CARTESIAN_POINT('Ctrl Pts',(369.832513261083,205.048575241124,780.282107787415));
#51904=CARTESIAN_POINT('Ctrl Pts',(370.038186801401,205.396602802461,780.800937575508));
#51905=CARTESIAN_POINT('Ctrl Pts',(370.518643518807,206.22785337804,781.677437375128));
#51906=CARTESIAN_POINT('Ctrl Pts',(370.836280008281,206.787728781571,782.069981441116));
#51907=CARTESIAN_POINT('Ctrl Pts',(371.504957457393,208.006691272921,782.587944800609));
#51908=CARTESIAN_POINT('Ctrl Pts',(371.855654969797,208.665985231776,782.713320551891));
#51909=CARTESIAN_POINT('Ctrl Pts',(372.174522500194,209.284559303216,782.713320551891));
#51910=CARTESIAN_POINT('',(371.253366994172,204.458559303216,777.887320551891));
#51911=CARTESIAN_POINT('',(369.479533939572,204.458559303216,777.887320551891));
#51912=CARTESIAN_POINT('Ctrl Pts',(373.885000951854,209.284559303216,782.713320551891));
#51913=CARTESIAN_POINT('Ctrl Pts',(373.573654695086,208.66656072828,782.713320551891));
#51914=CARTESIAN_POINT('Ctrl Pts',(373.231303497602,208.007813166231,782.588143904945));
#51915=CARTESIAN_POINT('Ctrl Pts',(372.578867361074,206.790033632963,782.071237654019));
#51916=CARTESIAN_POINT('Ctrl Pts',(372.269123915827,206.230807042441,781.679535597245));
#51917=CARTESIAN_POINT('Ctrl Pts',(371.799607321372,205.398534214463,780.803853655815));
#51918=CARTESIAN_POINT('Ctrl Pts',(371.598335180686,205.049534213614,780.284025646317));
#51919=CARTESIAN_POINT('Ctrl Pts',(371.324729057976,204.579224811203,779.128069862876));
#51920=CARTESIAN_POINT('Ctrl Pts',(371.253366994172,204.458559303216,778.491450416376));
#51921=CARTESIAN_POINT('Ctrl Pts',(371.253366994172,204.458559303216,777.887320551891));
#51922=CARTESIAN_POINT('Origin',(371.278766994172,204.458559303215,732.421320551891));
#51923=CARTESIAN_POINT('',(369.479533939571,204.458559303215,686.955320551891));
#51924=CARTESIAN_POINT('',(369.479533939572,204.458559303215,686.955320551891));
#51925=CARTESIAN_POINT('',(371.253366994171,204.458559303215,686.955320551891));
#51926=CARTESIAN_POINT('',(369.479533939571,204.458559303215,686.955320551891));
#51927=CARTESIAN_POINT('',(371.253366994172,204.458559303216,777.887320551891));
#51928=CARTESIAN_POINT('Origin',(371.278766994165,290.107359303215,677.93832055189));
#51929=CARTESIAN_POINT('',(369.479533939565,290.107359303215,682.38332055189));
#51930=CARTESIAN_POINT('',(369.479533939565,290.107359303215,682.38332055189));
#51931=CARTESIAN_POINT('',(369.479533939565,290.107359303215,673.49332055189));
#51932=CARTESIAN_POINT('',(369.479533939565,290.107359303215,673.49332055189));
#51933=CARTESIAN_POINT('',(369.479533939566,290.107359303215,682.38332055189));
#51934=CARTESIAN_POINT('Origin',(374.382788619839,207.616679248369,725.690320551891));
#51935=CARTESIAN_POINT('',(373.34861627154,208.238072685745,721.600920551891));
#51936=CARTESIAN_POINT('',(373.34861627154,208.238072685745,729.779720551891));
#51937=CARTESIAN_POINT('Origin',(373.348616271542,208.238072685748,725.690320551891));
#51938=CARTESIAN_POINT('',(371.369430483564,204.656456868911,725.690320551891));
#51939=CARTESIAN_POINT('Ctrl Pts',(373.348616271542,208.238072685748,729.779720551891));
#51940=CARTESIAN_POINT('Ctrl Pts',(373.111002505853,207.782332837277,729.779720551891));
#51941=CARTESIAN_POINT('Ctrl Pts',(372.852938079797,207.29856169085,729.677263832216));
#51942=CARTESIAN_POINT('Ctrl Pts',(372.370121550206,206.412992542174,729.259983769683));
#51943=CARTESIAN_POINT('Ctrl Pts',(372.145607374464,206.011070520602,728.945148373167));
#51944=CARTESIAN_POINT('Ctrl Pts',(371.787823800326,205.378702206411,728.218727390481));
#51945=CARTESIAN_POINT('Ctrl Pts',(371.630703535568,205.105998628624,727.758927137449));
#51946=CARTESIAN_POINT('Ctrl Pts',(371.421392251486,204.744945029254,726.75144934091));
#51947=CARTESIAN_POINT('Ctrl Pts',(371.369430483564,204.656456868911,726.203773691738));
#51948=CARTESIAN_POINT('Ctrl Pts',(371.369430483564,204.656456868911,725.690320551891));
#51949=CARTESIAN_POINT('',(373.310764264599,203.489985851499,725.690320551891));
#51950=CARTESIAN_POINT('',(372.276591916302,204.111379288878,725.690320551891));
#51951=CARTESIAN_POINT('Origin',(375.416960968136,206.99528581099,725.690320551891));
#51952=CARTESIAN_POINT('Ctrl Pts',(371.369430483564,204.656456868911,725.690320551891));
#51953=CARTESIAN_POINT('Ctrl Pts',(371.369430483564,204.656456868911,725.176818706141));
#51954=CARTESIAN_POINT('Ctrl Pts',(371.421402056017,204.744961667279,724.629094435344));
#51955=CARTESIAN_POINT('Ctrl Pts',(371.63074960008,205.106078362539,723.621542392833));
#51956=CARTESIAN_POINT('Ctrl Pts',(371.787896241403,205.37882844623,723.161716516555));
#51957=CARTESIAN_POINT('Ctrl Pts',(372.145703739218,206.011242640878,722.435347263539));
#51958=CARTESIAN_POINT('Ctrl Pts',(372.370204407382,206.41314283928,722.12056533247));
#51959=CARTESIAN_POINT('Ctrl Pts',(372.852983973297,207.298647545233,721.703358004294));
#51960=CARTESIAN_POINT('Ctrl Pts',(373.111025024262,207.782376027268,721.600920551891));
#51961=CARTESIAN_POINT('Ctrl Pts',(373.348616271542,208.238072685748,721.600920551891));
#51962=CARTESIAN_POINT('Origin',(298.461074890941,247.282959303216,725.690320551891));
#51963=CARTESIAN_POINT('',(376.030529085244,213.881959303216,782.713320551891));
#51964=CARTESIAN_POINT('Origin',(298.461074890966,247.282959303207,782.713320551852));
#51965=CARTESIAN_POINT('Origin',(298.461074890808,247.282959303293,686.955320551891));
#51966=CARTESIAN_POINT('',(371.253366994171,204.458559303215,682.383320551891));
#51967=CARTESIAN_POINT('Origin',(298.461074890893,247.28295930324,682.383320551859));
#51968=CARTESIAN_POINT('',(371.253366994171,204.458559303215,673.493320551891));
#51969=CARTESIAN_POINT('',(371.253366994171,204.458559303215,682.383320551891));
#51970=CARTESIAN_POINT('',(373.885000951854,209.284559303215,668.667320551891));
#51971=CARTESIAN_POINT('Ctrl Pts',(371.253366994171,204.458559303215,673.493320551891));
#51972=CARTESIAN_POINT('Ctrl Pts',(371.253366994171,204.458559303215,672.867055516681));
#51973=CARTESIAN_POINT('Ctrl Pts',(371.329992690807,204.588089445348,672.209345568075));
#51974=CARTESIAN_POINT('Ctrl Pts',(371.621425700043,205.08942707023,671.022230122433));
#51975=CARTESIAN_POINT('Ctrl Pts',(371.835180640338,205.460590532154,670.492294670939));
#51976=CARTESIAN_POINT('Ctrl Pts',(372.314344533021,206.312278105496,669.640607097597));
#51977=CARTESIAN_POINT('Ctrl Pts',(372.617063345927,206.860325790608,669.271384941795));
#51978=CARTESIAN_POINT('Ctrl Pts',(373.251819248663,208.047204152557,668.784753798678));
#51979=CARTESIAN_POINT('Ctrl Pts',(373.58354465675,208.686191547927,668.667320551891));
#51980=CARTESIAN_POINT('Ctrl Pts',(373.885000951854,209.284559303215,668.667320551891));
#51981=CARTESIAN_POINT('',(376.030529085244,213.881959303215,668.667320551891));
#51982=CARTESIAN_POINT('Origin',(298.461074890985,247.282959303195,668.667320551886));
#51983=CARTESIAN_POINT('',(376.030529085244,213.881959303215,668.667320551891));
#51984=CARTESIAN_POINT('',(373.348616271541,208.238072685746,721.600920551891));
#51985=CARTESIAN_POINT('',(373.34861627154,208.238072685745,762.621920551891));
#51986=CARTESIAN_POINT('',(373.34861627154,208.238072685745,770.800720551891));
#51987=CARTESIAN_POINT('',(373.348616271541,208.238072685747,762.621920551891));
#51988=CARTESIAN_POINT('',(371.369430483564,204.656456868912,766.711320551891));
#51989=CARTESIAN_POINT('Ctrl Pts',(371.369430483564,204.656456868912,766.711320551891));
#51990=CARTESIAN_POINT('Ctrl Pts',(371.369430483564,204.656456868912,766.197867412043));
#51991=CARTESIAN_POINT('Ctrl Pts',(371.421392251486,204.744945029254,765.650191762872));
#51992=CARTESIAN_POINT('Ctrl Pts',(371.630703535568,205.105998628625,764.642713966333));
#51993=CARTESIAN_POINT('Ctrl Pts',(371.787823800326,205.378702206411,764.1829137133));
#51994=CARTESIAN_POINT('Ctrl Pts',(372.145607374464,206.011070520602,763.456492730615));
#51995=CARTESIAN_POINT('Ctrl Pts',(372.370121550206,206.412992542174,763.141657334099));
#51996=CARTESIAN_POINT('Ctrl Pts',(372.852938079797,207.29856169085,762.724377271566));
#51997=CARTESIAN_POINT('Ctrl Pts',(373.111002505853,207.782332837278,762.621920551891));
#51998=CARTESIAN_POINT('Ctrl Pts',(373.348616271542,208.238072685749,762.621920551891));
#51999=CARTESIAN_POINT('Ctrl Pts',(373.348616271542,208.238072685749,770.800720551891));
#52000=CARTESIAN_POINT('Ctrl Pts',(373.111025024263,207.782376027268,770.800720551891));
#52001=CARTESIAN_POINT('Ctrl Pts',(372.852983973297,207.298647545233,770.698283099488));
#52002=CARTESIAN_POINT('Ctrl Pts',(372.370204407382,206.41314283928,770.281075771312));
#52003=CARTESIAN_POINT('Ctrl Pts',(372.145703739218,206.011242640879,769.966293840242));
#52004=CARTESIAN_POINT('Ctrl Pts',(371.787896241403,205.37882844623,769.239924587227));
#52005=CARTESIAN_POINT('Ctrl Pts',(371.63074960008,205.106078362539,768.780098710949));
#52006=CARTESIAN_POINT('Ctrl Pts',(371.421402056017,204.744961667279,767.772546668438));
#52007=CARTESIAN_POINT('Ctrl Pts',(371.369430483564,204.656456868912,767.224822397641));
#52008=CARTESIAN_POINT('Ctrl Pts',(371.369430483564,204.656456868912,766.711320551891));
#52009=CARTESIAN_POINT('Origin',(374.401714623309,209.990722665492,729.805120551895));
#52010=CARTESIAN_POINT('Origin',(371.183235802884,209.539164534576,725.690320551891));
#52011=CARTESIAN_POINT('',(374.600804303953,204.137211032768,725.182320551891));
#52012=CARTESIAN_POINT('',(374.600804303953,204.137211032768,726.198320551891));
#52013=CARTESIAN_POINT('Origin',(369.704973520276,207.078922948123,725.690320551891));
#52014=CARTESIAN_POINT('',(376.383495294708,205.82188363143,726.198320551891));
#52015=CARTESIAN_POINT('Origin',(371.183235802884,209.539164534576,726.198320551891));
#52016=CARTESIAN_POINT('',(375.817427244505,206.162011630486,728.560520551891));
#52017=CARTESIAN_POINT('Origin',(370.92159646083,209.10372354582,725.690320551891));
#52018=CARTESIAN_POINT('',(376.340705928614,207.032893607999,728.560520551891));
#52019=CARTESIAN_POINT('Origin',(371.183235802879,209.539164534579,728.560520551891));
#52020=CARTESIAN_POINT('',(376.906773978816,206.692765608943,726.198320551891));
#52021=CARTESIAN_POINT('Origin',(371.444875144938,209.974605523335,725.69032055189));
#52022=CARTESIAN_POINT('',(377.557328869166,209.057694205718,726.198320551891));
#52023=CARTESIAN_POINT('Origin',(371.183235802885,209.539164534576,726.198320551891));
#52024=CARTESIAN_POINT('',(377.557328869166,209.057694205718,725.182320551891));
#52025=CARTESIAN_POINT('Origin',(372.661498085491,211.999406121051,725.690320551891));
#52026=CARTESIAN_POINT('',(376.906773978816,206.692765608943,725.182320551891));
#52027=CARTESIAN_POINT('Origin',(371.183235802886,209.539164534575,725.182320551891));
#52028=CARTESIAN_POINT('',(376.340705928614,207.032893607999,722.820120551891));
#52029=CARTESIAN_POINT('Origin',(371.444875144939,209.974605523334,725.690320551891));
#52030=CARTESIAN_POINT('',(375.817427244505,206.162011630486,722.820120551891));
#52031=CARTESIAN_POINT('Origin',(371.183235802879,209.539164534579,722.820120551889));
#52032=CARTESIAN_POINT('',(376.383495294708,205.82188363143,725.182320551891));
#52033=CARTESIAN_POINT('Origin',(370.92159646083,209.103723545819,725.69032055189));
#52034=CARTESIAN_POINT('Origin',(371.183235802884,209.539164534576,725.182320551891));
#52035=CARTESIAN_POINT('Origin',(377.582728869161,286.21705079407,726.19832055189));
#52036=CARTESIAN_POINT('',(377.557328869161,285.508224400713,726.19832055189));
#52037=CARTESIAN_POINT('',(376.906773978811,287.873152997488,726.19832055189));
#52038=CARTESIAN_POINT('Origin',(371.183235802878,285.026754071854,726.19832055189));
#52039=CARTESIAN_POINT('',(375.980797174348,284.560948590652,726.19832055189));
#52040=CARTESIAN_POINT('',(375.980797174348,284.560948590652,726.19832055189));
#52041=CARTESIAN_POINT('',(374.764174233796,286.58574918837,726.19832055189));
#52042=CARTESIAN_POINT('',(374.764174233796,286.58574918837,726.19832055189));
#52043=CARTESIAN_POINT('',(374.764174233796,286.58574918837,726.19832055189));
#52044=CARTESIAN_POINT('Origin',(376.788427340403,285.046221752173,726.22372055189));
#52045=CARTESIAN_POINT('',(377.557328869161,285.508224400713,725.18232055189));
#52046=CARTESIAN_POINT('Origin',(372.661498085493,282.566512485378,725.69032055189));
#52047=CARTESIAN_POINT('',(375.980797174348,284.560948590652,725.18232055189));
#52048=CARTESIAN_POINT('',(375.980797174348,284.560948590652,725.18232055189));
#52049=CARTESIAN_POINT('',(375.980797174348,284.560948590652,726.19832055189));
#52050=CARTESIAN_POINT('Origin',(374.401714623305,284.575195940938,729.805120551893));
#52051=CARTESIAN_POINT('Origin',(373.348616271537,286.327845920682,725.69032055189));
#52052=CARTESIAN_POINT('Origin',(374.382788619834,286.949239358062,725.69032055189));
#52053=CARTESIAN_POINT('',(373.310764264593,291.075932754932,725.69032055189));
#52054=CARTESIAN_POINT('Origin',(375.416960968131,287.570632795441,725.69032055189));
#52055=CARTESIAN_POINT('',(372.276591916296,290.454539317552,725.69032055189));
#52056=CARTESIAN_POINT('Origin',(374.382788619839,207.61667924837,766.711320551891));
#52057=CARTESIAN_POINT('Origin',(373.348616271542,208.238072685749,766.71132055189));
#52058=CARTESIAN_POINT('',(373.310764264599,203.4899858515,766.711320551891));
#52059=CARTESIAN_POINT('',(372.276591916302,204.111379288879,766.711320551891));
#52060=CARTESIAN_POINT('Origin',(375.416960968136,206.995285810991,766.711320551891));
#52061=CARTESIAN_POINT('Origin',(376.160751551484,206.667365608943,766.203320551891));
#52062=CARTESIAN_POINT('',(377.557328869166,209.057694205718,766.203320551891));
#52063=CARTESIAN_POINT('',(376.906773978816,206.692765608944,766.203320551891));
#52064=CARTESIAN_POINT('Origin',(371.183235802887,209.539164534575,766.20332055189));
#52065=CARTESIAN_POINT('',(375.980797174353,210.00497001578,766.203320551891));
#52066=CARTESIAN_POINT('',(375.980797174353,210.00497001578,766.203320551891));
#52067=CARTESIAN_POINT('',(374.764174233801,207.980169418061,766.203320551891));
#52068=CARTESIAN_POINT('',(374.764174233801,207.980169418061,766.203320551891));
#52069=CARTESIAN_POINT('',(374.764174233801,207.980169418061,766.203320551891));
#52070=CARTESIAN_POINT('Origin',(376.788427340408,209.519696854259,767.244720551891));
#52071=CARTESIAN_POINT('',(377.557328869166,209.057694205718,767.219320551891));
#52072=CARTESIAN_POINT('Origin',(372.661498085491,211.999406121052,766.711320551891));
#52073=CARTESIAN_POINT('',(375.980797174353,210.00497001578,767.219320551891));
#52074=CARTESIAN_POINT('',(375.980797174353,210.00497001578,767.219320551891));
#52075=CARTESIAN_POINT('',(375.980797174353,210.00497001578,766.203320551891));
#52076=CARTESIAN_POINT('Origin',(376.160751551484,206.667365608943,767.219320551891));
#52077=CARTESIAN_POINT('',(376.906773978816,206.692765608944,767.219320551891));
#52078=CARTESIAN_POINT('Origin',(371.183235802884,209.539164534576,767.219320551891));
#52079=CARTESIAN_POINT('',(374.764174233801,207.980169418061,767.219320551891));
#52080=CARTESIAN_POINT('',(374.764174233801,207.980169418061,767.219320551891));
#52081=CARTESIAN_POINT('',(375.980797174353,210.00497001578,767.219320551891));
#52082=CARTESIAN_POINT('Origin',(375.835474106309,207.336467513502,769.606920551891));
#52083=CARTESIAN_POINT('',(376.340705928614,207.032893608,769.581520551891));
#52084=CARTESIAN_POINT('Origin',(371.444875144934,209.974605523338,766.711320551889));
#52085=CARTESIAN_POINT('',(374.764174233801,207.980169418061,769.581520551891));
#52086=CARTESIAN_POINT('',(374.764174233801,207.980169418061,769.581520551891));
#52087=CARTESIAN_POINT('',(374.764174233801,207.980169418061,767.219320551891));
#52088=CARTESIAN_POINT('Origin',(375.290800739153,206.136611630486,769.581520551891));
#52089=CARTESIAN_POINT('',(375.817427244505,206.162011630486,769.581520551891));
#52090=CARTESIAN_POINT('Origin',(371.183235802886,209.539164534575,769.581520551896));
#52091=CARTESIAN_POINT('',(374.240895549693,207.109287440548,769.581520551891));
#52092=CARTESIAN_POINT('',(374.240895549693,207.109287440548,769.581520551891));
#52093=CARTESIAN_POINT('',(374.764174233801,207.980169418061,769.581520551891));
#52094=CARTESIAN_POINT('Origin',(375.3121954222,206.465585535989,769.606920551891));
#52095=CARTESIAN_POINT('',(376.383495294708,205.82188363143,767.219320551891));
#52096=CARTESIAN_POINT('Origin',(370.921596460826,209.103723545823,766.71132055189));
#52097=CARTESIAN_POINT('',(374.240895549693,207.109287440548,767.219320551891));
#52098=CARTESIAN_POINT('',(374.240895549693,207.109287440548,767.219320551891));
#52099=CARTESIAN_POINT('',(374.240895549693,207.109287440548,769.581520551891));
#52100=CARTESIAN_POINT('Origin',(374.703883951924,204.111811032768,767.219320551891));
#52101=CARTESIAN_POINT('',(374.600804303953,204.137211032768,767.219320551891));
#52102=CARTESIAN_POINT('Origin',(371.183235802884,209.539164534577,767.219320551891));
#52103=CARTESIAN_POINT('',(373.02427260914,205.084486842829,767.219320551891));
#52104=CARTESIAN_POINT('',(373.02427260914,205.084486842829,767.219320551891));
#52105=CARTESIAN_POINT('',(374.240895549693,207.109287440548,767.219320551891));
#52106=CARTESIAN_POINT('Origin',(373.831902775195,204.599213681308,767.244720551891));
#52107=CARTESIAN_POINT('',(374.600804303953,204.137211032768,766.203320551891));
#52108=CARTESIAN_POINT('Origin',(369.704973520302,207.07892294808,766.711320551891));
#52109=CARTESIAN_POINT('',(373.02427260914,205.084486842829,766.203320551891));
#52110=CARTESIAN_POINT('',(373.02427260914,205.084486842829,766.203320551891));
#52111=CARTESIAN_POINT('',(373.02427260914,205.084486842829,767.219320551891));
#52112=CARTESIAN_POINT('Origin',(374.703883951924,204.111811032768,766.203320551891));
#52113=CARTESIAN_POINT('',(376.383495294708,205.82188363143,766.203320551891));
#52114=CARTESIAN_POINT('Origin',(371.183235802884,209.539164534576,766.203320551891));
#52115=CARTESIAN_POINT('',(374.240895549693,207.109287440548,766.203320551891));
#52116=CARTESIAN_POINT('',(374.240895549693,207.109287440548,766.203320551891));
#52117=CARTESIAN_POINT('',(373.02427260914,205.084486842829,766.203320551891));
#52118=CARTESIAN_POINT('Origin',(375.3121954222,206.465585535989,766.228720551891));
#52119=CARTESIAN_POINT('',(375.817427244505,206.162011630486,763.841120551891));
#52120=CARTESIAN_POINT('Origin',(370.921596460832,209.103723545819,766.71132055189));
#52121=CARTESIAN_POINT('',(374.240895549693,207.109287440548,763.841120551891));
#52122=CARTESIAN_POINT('',(374.240895549693,207.109287440548,763.841120551891));
#52123=CARTESIAN_POINT('',(374.240895549693,207.109287440548,766.203320551891));
#52124=CARTESIAN_POINT('Origin',(375.290800739153,206.136611630486,763.841120551891));
#52125=CARTESIAN_POINT('',(376.340705928614,207.032893608,763.841120551891));
#52126=CARTESIAN_POINT('Origin',(371.183235802886,209.539164534575,763.841120551891));
#52127=CARTESIAN_POINT('',(374.764174233801,207.980169418061,763.841120551891));
#52128=CARTESIAN_POINT('',(374.764174233801,207.980169418061,763.841120551891));
#52129=CARTESIAN_POINT('',(374.240895549693,207.109287440548,763.841120551891));
#52130=CARTESIAN_POINT('Origin',(375.835474106309,207.336467513502,766.228720551891));
#52131=CARTESIAN_POINT('Origin',(371.44487514494,209.974605523334,766.711320551891));
#52132=CARTESIAN_POINT('',(374.764174233801,207.980169418061,763.841120551891));
#52133=CARTESIAN_POINT('Origin',(374.502534891747,207.544728429305,769.606920551891));
#52134=CARTESIAN_POINT('Origin',(371.183235802883,209.539164534576,766.711320551891));
#52135=CARTESIAN_POINT('Origin',(374.40171462331,209.990722665493,770.826120551895));
#52136=CARTESIAN_POINT('Origin',(371.682267445707,285.281359303215,673.49332055189));
#52137=CARTESIAN_POINT('',(372.174522500188,285.281359303215,668.66732055189));
#52138=CARTESIAN_POINT('Ctrl Pts',(369.479533939566,290.107359303215,673.49332055189));
#52139=CARTESIAN_POINT('Ctrl Pts',(369.479533939566,290.107359303215,672.866062516448));
#52140=CARTESIAN_POINT('Ctrl Pts',(369.558322308944,289.977425390663,672.207866460247));
#52141=CARTESIAN_POINT('Ctrl Pts',(369.857209361088,289.475707577428,671.020898051897));
#52142=CARTESIAN_POINT('Ctrl Pts',(370.076200297233,289.104596282447,670.491562879109));
#52143=CARTESIAN_POINT('Ctrl Pts',(370.566888715326,288.253205154171,669.640171750834));
#52144=CARTESIAN_POINT('Ctrl Pts',(370.877007932881,287.704996235544,669.271056258472));
#52145=CARTESIAN_POINT('Ctrl Pts',(371.526813678761,286.518227155965,668.784638158735));
#52146=CARTESIAN_POINT('Ctrl Pts',(371.866187207677,285.879501788967,668.66732055189));
#52147=CARTESIAN_POINT('Ctrl Pts',(372.174522500189,285.281359303215,668.66732055189));
#52148=CARTESIAN_POINT('',(373.885000951848,285.281359303215,668.66732055189));
#52149=CARTESIAN_POINT('Origin',(428.12807489095,277.381959303219,670.19132055189));
#52150=CARTESIAN_POINT('',(427.36607489095,282.207959303219,670.19132055189));
#52151=CARTESIAN_POINT('',(427.36607489095,277.381959303219,665.36532055189));
#52152=CARTESIAN_POINT('Origin',(427.36607489095,277.381959303219,670.19132055189));
#52153=CARTESIAN_POINT('',(428.89007489095,282.207959303219,670.19132055189));
#52154=CARTESIAN_POINT('',(428.89007489095,282.207959303219,670.19132055189));
#52155=CARTESIAN_POINT('',(428.89007489095,277.381959303219,665.36532055189));
#52156=CARTESIAN_POINT('Origin',(428.89007489095,277.381959303219,670.19132055189));
#52157=CARTESIAN_POINT('',(428.89007489095,277.381959303219,665.36532055189));
#52158=CARTESIAN_POINT('Origin',(428.128074890954,217.158559303219,665.365320551891));
#52159=CARTESIAN_POINT('',(427.366074890954,217.183959303219,665.365320551891));
#52160=CARTESIAN_POINT('',(427.36607489095,277.381959303219,665.36532055189));
#52161=CARTESIAN_POINT('',(428.890074890954,217.183959303219,665.365320551891));
#52162=CARTESIAN_POINT('',(428.89007489095,277.381959303219,665.36532055189));
#52163=CARTESIAN_POINT('',(428.890074890954,217.183959303219,665.365320551891));
#52164=CARTESIAN_POINT('Origin',(428.128074890954,217.183959303219,670.191320551891));
#52165=CARTESIAN_POINT('',(427.366074890954,212.357959303219,670.191320551891));
#52166=CARTESIAN_POINT('Origin',(427.366074890954,217.183959303219,670.191320551891));
#52167=CARTESIAN_POINT('',(428.890074890954,212.357959303219,670.191320551891));
#52168=CARTESIAN_POINT('Origin',(428.890074890954,217.183959303219,670.19132055189));
#52169=CARTESIAN_POINT('',(428.890074890954,212.357959303219,670.191320551891));
#52170=CARTESIAN_POINT('Origin',(428.915474890955,212.357959303219,725.690320551891));
#52171=CARTESIAN_POINT('',(427.366074890955,212.35795930322,781.189320551891));
#52172=CARTESIAN_POINT('',(427.366074890954,212.357959303219,670.191320551891));
#52173=CARTESIAN_POINT('',(428.890074890955,212.35795930322,781.189320551891));
#52174=CARTESIAN_POINT('',(428.890074890954,212.357959303219,670.191320551891));
#52175=CARTESIAN_POINT('',(428.890074890955,212.35795930322,781.189320551891));
#52176=CARTESIAN_POINT('Origin',(428.128074890954,217.18395930322,781.189320551891));
#52177=CARTESIAN_POINT('',(427.366074890954,217.183959375133,786.015320551891));
#52178=CARTESIAN_POINT('Origin',(427.366074890954,217.183959303219,781.189320551891));
#52179=CARTESIAN_POINT('',(428.890074890954,217.183959375133,786.015320551891));
#52180=CARTESIAN_POINT('Origin',(428.890074890954,217.18395930322,781.189320551891));
#52181=CARTESIAN_POINT('',(428.890074890954,217.183959375133,786.015320551891));
#52182=CARTESIAN_POINT('Origin',(428.128074890955,217.158559375133,786.015320551891));
#52183=CARTESIAN_POINT('',(427.36607489095,277.38195930322,786.01532055189));
#52184=CARTESIAN_POINT('',(427.366074890954,217.183959375133,786.015320551891));
#52185=CARTESIAN_POINT('',(428.89007489095,277.38195930322,786.01532055189));
#52186=CARTESIAN_POINT('',(428.890074890954,217.183959375133,786.015320551891));
#52187=CARTESIAN_POINT('',(428.89007489095,277.38195930322,786.01532055189));
#52188=CARTESIAN_POINT('Origin',(428.12807489095,277.381959303219,781.18932055189));
#52189=CARTESIAN_POINT('',(427.36607489095,282.20795930322,781.18932055189));
#52190=CARTESIAN_POINT('Origin',(427.36607489095,277.38195930322,781.18932055189));
#52191=CARTESIAN_POINT('',(428.89007489095,282.20795930322,781.18932055189));
#52192=CARTESIAN_POINT('Origin',(428.89007489095,277.38195930322,781.18932055189));
#52193=CARTESIAN_POINT('',(428.89007489095,282.20795930322,781.18932055189));
#52194=CARTESIAN_POINT('Origin',(428.91547489095,282.207959303219,725.69032055189));
#52195=CARTESIAN_POINT('',(427.36607489095,282.20795930322,781.18932055189));
#52196=CARTESIAN_POINT('',(428.89007489095,282.20795930322,781.18932055189));
#52197=CARTESIAN_POINT('Origin',(427.366074890955,212.332559303219,725.690320566784));
#52198=CARTESIAN_POINT('',(427.36607489095,280.683959303219,668.66732055189));
#52199=CARTESIAN_POINT('',(427.36607489095,280.68395930322,782.71332055189));
#52200=CARTESIAN_POINT('',(427.36607489095,280.683959303219,668.66732055189));
#52201=CARTESIAN_POINT('',(427.366074890955,213.88195930322,782.713320551891));
#52202=CARTESIAN_POINT('',(427.36607489095,280.68395930322,782.71332055189));
#52203=CARTESIAN_POINT('',(427.366074890954,213.881959303219,668.667320551891));
#52204=CARTESIAN_POINT('',(427.366074890954,213.881959303219,668.667320551891));
#52205=CARTESIAN_POINT('',(427.36607489095,280.683959303219,668.66732055189));
#52206=CARTESIAN_POINT('Origin',(428.890074890955,212.332559303219,725.690320566784));
#52207=CARTESIAN_POINT('',(428.890074890954,220.231959303219,679.10672055189));
#52208=CARTESIAN_POINT('Origin',(428.890074890954,220.231959303219,675.017320551891));
#52209=CARTESIAN_POINT('',(428.890074890951,274.33395930322,780.45272055189));
#52210=CARTESIAN_POINT('Origin',(428.89007489095,274.33395930322,776.36332055189));
#52211=CARTESIAN_POINT('',(428.89007489095,279.032959303219,740.16832055189));
#52212=CARTESIAN_POINT('',(428.89007489095,279.032959303219,711.21232055189));
#52213=CARTESIAN_POINT('',(428.89007489095,279.032959303219,740.16832055189));
#52214=CARTESIAN_POINT('',(428.89007489095,275.984959303219,708.16432055189));
#52215=CARTESIAN_POINT('Origin',(428.89007489095,275.984959303219,711.21232055189));
#52216=CARTESIAN_POINT('',(428.890074890954,218.580959303219,708.164320551891));
#52217=CARTESIAN_POINT('',(428.89007489095,275.984959303219,708.16432055189));
#52218=CARTESIAN_POINT('',(428.890074890954,215.532959303219,711.212320551891));
#52219=CARTESIAN_POINT('Origin',(428.890074890954,218.580959303219,711.212320551891));
#52220=CARTESIAN_POINT('',(428.890074890954,215.532959303219,740.168320551891));
#52221=CARTESIAN_POINT('',(428.890074890954,215.532959303219,711.212320551891));
#52222=CARTESIAN_POINT('',(428.890074890954,218.580959303219,743.216320551891));
#52223=CARTESIAN_POINT('Origin',(428.890074890954,218.580959303219,740.168320551891));
#52224=CARTESIAN_POINT('',(428.89007489095,275.984959303219,743.21632055189));
#52225=CARTESIAN_POINT('',(428.890074890954,218.580959303219,743.216320551891));
#52226=CARTESIAN_POINT('Origin',(428.89007489095,275.984959303219,740.16832055189));
#52227=CARTESIAN_POINT('Origin',(429.41077489095,275.984959303219,711.21232055189));
#52228=CARTESIAN_POINT('',(429.93147489095,279.032959303219,711.21232055189));
#52229=CARTESIAN_POINT('',(429.93147489095,279.032959303219,711.21232055189));
#52230=CARTESIAN_POINT('',(429.93147489095,275.984959303219,708.16432055189));
#52231=CARTESIAN_POINT('Origin',(429.93147489095,275.984959303219,711.21232055189));
#52232=CARTESIAN_POINT('',(429.93147489095,275.984959303219,708.16432055189));
#52233=CARTESIAN_POINT('Origin',(429.410774890954,218.555559303219,708.164320551891));
#52234=CARTESIAN_POINT('',(429.931474890954,218.580959303219,708.164320551891));
#52235=CARTESIAN_POINT('',(429.93147489095,275.984959303219,708.16432055189));
#52236=CARTESIAN_POINT('',(429.931474890954,218.580959303219,708.164320551891));
#52237=CARTESIAN_POINT('Origin',(429.410774890954,218.580959303219,711.21232055189));
#52238=CARTESIAN_POINT('',(429.931474890954,215.532959303219,711.212320551891));
#52239=CARTESIAN_POINT('Origin',(429.931474890954,218.580959303219,711.212320551891));
#52240=CARTESIAN_POINT('',(429.931474890954,215.532959303219,711.212320551891));
#52241=CARTESIAN_POINT('Origin',(429.956874890954,215.532959303219,725.690320551891));
#52242=CARTESIAN_POINT('',(429.931474890954,215.532959303219,740.168320551891));
#52243=CARTESIAN_POINT('',(429.931474890954,215.532959303219,711.212320551891));
#52244=CARTESIAN_POINT('',(429.931474890954,215.532959303219,740.168320551891));
#52245=CARTESIAN_POINT('Origin',(429.410774890954,218.580959303219,740.168320551891));
#52246=CARTESIAN_POINT('',(429.931474890954,218.580959303219,743.216320551891));
#52247=CARTESIAN_POINT('Origin',(429.931474890954,218.580959303219,740.168320551891));
#52248=CARTESIAN_POINT('',(429.931474890954,218.580959303219,743.216320551891));
#52249=CARTESIAN_POINT('Origin',(429.410774890954,218.555559303219,743.216320551891));
#52250=CARTESIAN_POINT('',(429.93147489095,275.984959303219,743.21632055189));
#52251=CARTESIAN_POINT('',(429.931474890954,218.580959303219,743.216320551891));
#52252=CARTESIAN_POINT('',(429.93147489095,275.984959303219,743.21632055189));
#52253=CARTESIAN_POINT('Origin',(429.41077489095,275.984959303219,740.16832055189));
#52254=CARTESIAN_POINT('',(429.93147489095,279.032959303219,740.16832055189));
#52255=CARTESIAN_POINT('Origin',(429.93147489095,275.984959303219,740.16832055189));
#52256=CARTESIAN_POINT('',(429.93147489095,279.032959303219,740.16832055189));
#52257=CARTESIAN_POINT('Origin',(429.95687489095,279.032959303219,725.69032055189));
#52258=CARTESIAN_POINT('',(429.93147489095,279.032959303219,740.16832055189));
#52259=CARTESIAN_POINT('Origin',(429.931474890954,215.507559303219,725.690320551891));
#52260=CARTESIAN_POINT('Origin',(426.353194189194,274.333959303219,776.36332055189));
#52261=CARTESIAN_POINT('',(431.404674890951,274.33395930322,780.45272055189));
#52262=CARTESIAN_POINT('Origin',(431.404674890951,274.33395930322,776.36332055189));
#52263=CARTESIAN_POINT('',(432.812646305297,274.33395930322,775.644900062204));
#52264=CARTESIAN_POINT('',(432.162199060962,272.663631664701,773.974572423685));
#52265=CARTESIAN_POINT('Origin',(426.353194189182,274.693169548068,776.004110307046));
#52266=CARTESIAN_POINT('',(432.162199060962,271.945211175015,774.692992913371));
#52267=CARTESIAN_POINT('Origin',(426.353194189229,272.304421419856,774.333782668527));
#52268=CARTESIAN_POINT('',(432.812646305297,273.615538813534,776.36332055189));
#52269=CARTESIAN_POINT('Origin',(426.35319418918,273.974749058382,776.722530796734));
#52270=CARTESIAN_POINT('',(432.162199060962,271.945211175015,778.033648190409));
#52271=CARTESIAN_POINT('Origin',(426.353194189181,273.974749058382,776.004110307047));
#52272=CARTESIAN_POINT('',(432.162199060962,272.663631664701,778.752068680094));
#52273=CARTESIAN_POINT('Origin',(426.353194189236,272.30442141982,778.392858435289));
#52274=CARTESIAN_POINT('',(432.812646305297,274.33395930322,777.081741041575));
#52275=CARTESIAN_POINT('Origin',(426.35319418918,274.693169548067,776.722530796732));
#52276=CARTESIAN_POINT('',(432.162199060961,276.004286941739,778.752068680094));
#52277=CARTESIAN_POINT('Origin',(426.35319418918,273.97474905837,776.722530796732));
#52278=CARTESIAN_POINT('',(432.162199060961,276.722707431424,778.033648190409));
#52279=CARTESIAN_POINT('Origin',(426.35319418923,276.363497186619,778.39285843529));
#52280=CARTESIAN_POINT('',(432.812646305296,275.052379792905,776.36332055189));
#52281=CARTESIAN_POINT('Origin',(426.35319418918,274.693169548057,776.004110307047));
#52282=CARTESIAN_POINT('',(432.162199060961,276.722707431424,774.692992913371));
#52283=CARTESIAN_POINT('Origin',(426.35319418918,274.693169548056,776.722530796733));
#52284=CARTESIAN_POINT('',(432.162199060961,276.004286941739,773.974572423685));
#52285=CARTESIAN_POINT('Origin',(426.353194189222,276.363497186581,774.333782668528));
#52286=CARTESIAN_POINT('Origin',(426.353194189182,273.974749058371,776.004110307047));
#52287=CARTESIAN_POINT('Origin',(430.147374890951,274.33395930322,776.36332055189));
#52288=CARTESIAN_POINT('',(430.147374890951,274.33395930322,780.45272055189));
#52289=CARTESIAN_POINT('Origin',(426.353194189198,220.231959303218,675.01732055189));
#52290=CARTESIAN_POINT('',(431.404674890954,220.231959303219,679.10672055189));
#52291=CARTESIAN_POINT('Origin',(431.404674890954,220.231959303219,675.017320551891));
#52292=CARTESIAN_POINT('',(432.8126463053,220.231959303219,674.298900062205));
#52293=CARTESIAN_POINT('',(432.162199060965,218.5616316647,672.628572423686));
#52294=CARTESIAN_POINT('Origin',(426.353194189186,220.591169548065,674.658110307049));
#52295=CARTESIAN_POINT('',(432.162199060965,217.843211175014,673.346992913372));
#52296=CARTESIAN_POINT('Origin',(426.35319418923,218.202421419857,672.987782668529));
#52297=CARTESIAN_POINT('',(432.8126463053,219.513538813533,675.017320551891));
#52298=CARTESIAN_POINT('Origin',(426.353194189188,219.872749058377,675.376530796737));
#52299=CARTESIAN_POINT('',(432.162199060965,217.843211175015,676.687648190409));
#52300=CARTESIAN_POINT('Origin',(426.353194189187,219.872749058378,674.658110307044));
#52301=CARTESIAN_POINT('',(432.162199060965,218.5616316647,677.406068680095));
#52302=CARTESIAN_POINT('Origin',(426.353194189245,218.202421419855,677.046858435254));
#52303=CARTESIAN_POINT('',(432.8126463053,220.231959303219,675.735741041576));
#52304=CARTESIAN_POINT('Origin',(426.353194189186,220.591169548064,675.376530796731));
#52305=CARTESIAN_POINT('',(432.162199060965,221.902286941738,677.406068680095));
#52306=CARTESIAN_POINT('Origin',(426.353194189186,219.872749058373,675.376530796731));
#52307=CARTESIAN_POINT('',(432.162199060965,222.620707431423,676.687648190409));
#52308=CARTESIAN_POINT('Origin',(426.35319418924,222.261497186587,677.046858435259));
#52309=CARTESIAN_POINT('',(432.8126463053,220.950379792904,675.017320551891));
#52310=CARTESIAN_POINT('Origin',(426.353194189186,220.591169548059,674.658110307044));
#52311=CARTESIAN_POINT('',(432.162199060965,222.620707431423,673.346992913372));
#52312=CARTESIAN_POINT('Origin',(426.353194189186,220.591169548059,675.376530796737));
#52313=CARTESIAN_POINT('',(432.162199060965,221.902286941738,672.628572423686));
#52314=CARTESIAN_POINT('Origin',(426.353194189235,222.26149718658,672.987782668529));
#52315=CARTESIAN_POINT('Origin',(426.353194189186,219.872749058373,674.658110307051));
#52316=CARTESIAN_POINT('Origin',(430.147374890954,220.231959303219,675.017320551891));
#52317=CARTESIAN_POINT('',(430.147374890954,220.231959303219,679.10672055189));
#52318=CARTESIAN_POINT('Origin',(432.232023881687,222.26149718658,672.987782668529));
#52319=CARTESIAN_POINT('',(430.312474890954,222.620707431423,673.346992913372));
#52320=CARTESIAN_POINT('',(430.312474890954,222.620707431423,673.346992913372));
#52321=CARTESIAN_POINT('',(430.312474890954,221.902286941738,672.628572423686));
#52322=CARTESIAN_POINT('',(430.312474890954,222.620707431423,673.346992913372));
#52323=CARTESIAN_POINT('',(430.312474890954,221.902286941738,672.628572423686));
#52324=CARTESIAN_POINT('Origin',(432.8380463053,221.067123122478,673.463736242946));
#52325=CARTESIAN_POINT('',(430.312474890954,220.231959303219,674.298900062205));
#52326=CARTESIAN_POINT('',(430.312474890954,221.902286941738,672.628572423686));
#52327=CARTESIAN_POINT('',(430.312474890954,220.231959303219,674.298900062205));
#52328=CARTESIAN_POINT('Origin',(432.8380463053,219.39679548396,673.463736242946));
#52329=CARTESIAN_POINT('',(430.312474890954,218.5616316647,672.628572423686));
#52330=CARTESIAN_POINT('',(430.312474890954,220.231959303219,674.298900062205));
#52331=CARTESIAN_POINT('',(430.312474890954,218.5616316647,672.628572423686));
#52332=CARTESIAN_POINT('Origin',(432.232023881687,218.202421419857,672.987782668529));
#52333=CARTESIAN_POINT('',(430.312474890954,217.843211175014,673.346992913372));
#52334=CARTESIAN_POINT('',(430.312474890954,218.5616316647,672.628572423686));
#52335=CARTESIAN_POINT('',(430.312474890954,217.843211175014,673.346992913372));
#52336=CARTESIAN_POINT('Origin',(432.8380463053,218.678374994274,674.182156732631));
#52337=CARTESIAN_POINT('',(430.312474890954,219.513538813533,675.017320551891));
#52338=CARTESIAN_POINT('',(430.312474890954,217.843211175014,673.346992913372));
#52339=CARTESIAN_POINT('',(430.312474890954,219.513538813533,675.017320551891));
#52340=CARTESIAN_POINT('Origin',(432.8380463053,218.678374994274,675.85248437115));
#52341=CARTESIAN_POINT('',(430.312474890954,217.843211175014,676.687648190409));
#52342=CARTESIAN_POINT('',(430.312474890954,219.513538813533,675.017320551891));
#52343=CARTESIAN_POINT('',(430.312474890954,217.843211175014,676.687648190409));
#52344=CARTESIAN_POINT('Origin',(432.232023881687,218.202421419857,677.046858435252));
#52345=CARTESIAN_POINT('',(430.312474890954,218.5616316647,677.406068680095));
#52346=CARTESIAN_POINT('',(430.312474890954,217.843211175014,676.687648190409));
#52347=CARTESIAN_POINT('',(430.312474890954,218.5616316647,677.406068680095));
#52348=CARTESIAN_POINT('Origin',(432.8380463053,219.396795483959,676.570904860836));
#52349=CARTESIAN_POINT('',(430.312474890954,220.231959303219,675.735741041576));
#52350=CARTESIAN_POINT('',(430.312474890954,218.5616316647,677.406068680095));
#52351=CARTESIAN_POINT('',(430.312474890954,220.231959303219,675.735741041576));
#52352=CARTESIAN_POINT('Origin',(432.8380463053,221.067123122478,676.570904860836));
#52353=CARTESIAN_POINT('',(430.312474890954,221.902286941738,677.406068680095));
#52354=CARTESIAN_POINT('',(430.312474890954,220.231959303219,675.735741041576));
#52355=CARTESIAN_POINT('',(430.312474890954,221.902286941738,677.406068680095));
#52356=CARTESIAN_POINT('Origin',(432.232023881687,222.261497186581,677.046858435252));
#52357=CARTESIAN_POINT('',(430.312474890954,222.620707431423,676.687648190409));
#52358=CARTESIAN_POINT('',(430.312474890954,221.902286941738,677.406068680095));
#52359=CARTESIAN_POINT('',(430.312474890954,222.620707431423,676.687648190409));
#52360=CARTESIAN_POINT('Origin',(432.8380463053,221.785543612164,675.85248437115));
#52361=CARTESIAN_POINT('',(430.312474890954,220.950379792904,675.017320551891));
#52362=CARTESIAN_POINT('',(430.312474890954,222.620707431423,676.687648190409));
#52363=CARTESIAN_POINT('',(430.312474890954,220.950379792904,675.017320551891));
#52364=CARTESIAN_POINT('Origin',(432.8380463053,221.785543612164,674.182156732631));
#52365=CARTESIAN_POINT('',(430.312474890954,220.950379792904,675.017320551891));
#52366=CARTESIAN_POINT('Origin',(430.312474890954,217.817811175014,675.017320551891));
#52367=CARTESIAN_POINT('Origin',(432.232023881683,276.363497186581,774.333782668528));
#52368=CARTESIAN_POINT('',(430.31247489095,276.722707431424,774.692992913371));
#52369=CARTESIAN_POINT('',(430.31247489095,276.722707431424,774.692992913371));
#52370=CARTESIAN_POINT('',(430.31247489095,276.004286941739,773.974572423685));
#52371=CARTESIAN_POINT('',(430.31247489095,276.722707431424,774.692992913371));
#52372=CARTESIAN_POINT('',(430.31247489095,276.004286941739,773.974572423685));
#52373=CARTESIAN_POINT('Origin',(432.838046305297,275.169123122479,774.809736242944));
#52374=CARTESIAN_POINT('',(430.312474890951,274.33395930322,775.644900062204));
#52375=CARTESIAN_POINT('',(430.31247489095,276.004286941739,773.974572423685));
#52376=CARTESIAN_POINT('',(430.312474890951,274.33395930322,775.644900062204));
#52377=CARTESIAN_POINT('Origin',(432.838046305297,273.49879548396,774.809736242944));
#52378=CARTESIAN_POINT('',(430.312474890951,272.663631664701,773.974572423685));
#52379=CARTESIAN_POINT('',(430.312474890951,274.33395930322,775.644900062204));
#52380=CARTESIAN_POINT('',(430.312474890951,272.663631664701,773.974572423685));
#52381=CARTESIAN_POINT('Origin',(432.232023881684,272.304421419858,774.333782668528));
#52382=CARTESIAN_POINT('',(430.312474890951,271.945211175015,774.692992913371));
#52383=CARTESIAN_POINT('',(430.312474890951,272.663631664701,773.974572423685));
#52384=CARTESIAN_POINT('',(430.312474890951,271.945211175015,774.692992913371));
#52385=CARTESIAN_POINT('Origin',(432.838046305297,272.780374994275,775.528156732631));
#52386=CARTESIAN_POINT('',(430.312474890951,273.615538813534,776.36332055189));
#52387=CARTESIAN_POINT('',(430.312474890951,271.945211175015,774.692992913371));
#52388=CARTESIAN_POINT('',(430.312474890951,273.615538813534,776.36332055189));
#52389=CARTESIAN_POINT('Origin',(432.838046305297,272.780374994275,777.19848437115));
#52390=CARTESIAN_POINT('',(430.312474890951,271.945211175015,778.033648190409));
#52391=CARTESIAN_POINT('',(430.312474890951,273.615538813534,776.36332055189));
#52392=CARTESIAN_POINT('',(430.312474890951,271.945211175015,778.033648190409));
#52393=CARTESIAN_POINT('Origin',(432.232023881684,272.304421419858,778.392858435251));
#52394=CARTESIAN_POINT('',(430.312474890951,272.663631664701,778.752068680094));
#52395=CARTESIAN_POINT('',(430.312474890951,271.945211175015,778.033648190409));
#52396=CARTESIAN_POINT('',(430.312474890951,272.663631664701,778.752068680094));
#52397=CARTESIAN_POINT('Origin',(432.838046305297,273.49879548396,777.916904860835));
#52398=CARTESIAN_POINT('',(430.312474890951,274.33395930322,777.081741041575));
#52399=CARTESIAN_POINT('',(430.312474890951,272.663631664701,778.752068680094));
#52400=CARTESIAN_POINT('',(430.312474890951,274.33395930322,777.081741041575));
#52401=CARTESIAN_POINT('Origin',(432.838046305297,275.169123122479,777.916904860835));
#52402=CARTESIAN_POINT('',(430.31247489095,276.004286941739,778.752068680094));
#52403=CARTESIAN_POINT('',(430.312474890951,274.33395930322,777.081741041575));
#52404=CARTESIAN_POINT('',(430.31247489095,276.004286941739,778.752068680094));
#52405=CARTESIAN_POINT('Origin',(432.232023881683,276.363497186581,778.392858435251));
#52406=CARTESIAN_POINT('',(430.31247489095,276.722707431424,778.033648190409));
#52407=CARTESIAN_POINT('',(430.31247489095,276.004286941739,778.752068680094));
#52408=CARTESIAN_POINT('',(430.31247489095,276.722707431424,778.033648190409));
#52409=CARTESIAN_POINT('Origin',(432.838046305296,275.887543612165,777.19848437115));
#52410=CARTESIAN_POINT('',(430.312474890951,275.052379792905,776.36332055189));
#52411=CARTESIAN_POINT('',(430.31247489095,276.722707431424,778.033648190409));
#52412=CARTESIAN_POINT('',(430.312474890951,275.052379792905,776.36332055189));
#52413=CARTESIAN_POINT('Origin',(432.838046305296,275.887543612165,775.528156732631));
#52414=CARTESIAN_POINT('',(430.312474890951,275.052379792905,776.36332055189));
#52415=CARTESIAN_POINT('Origin',(430.312474890951,271.919811175015,776.36332055189));
#52416=CARTESIAN_POINT('Origin',(374.502534891742,287.021190177127,769.60692055189));
#52417=CARTESIAN_POINT('',(374.764174233796,286.58574918837,763.84112055189));
#52418=CARTESIAN_POINT('',(374.764174233796,286.58574918837,766.20332055189));
#52419=CARTESIAN_POINT('',(374.240895549687,287.456631165884,763.84112055189));
#52420=CARTESIAN_POINT('',(374.764174233796,286.58574918837,763.84112055189));
#52421=CARTESIAN_POINT('',(374.240895549687,287.456631165884,766.20332055189));
#52422=CARTESIAN_POINT('',(374.240895549687,287.456631165884,763.84112055189));
#52423=CARTESIAN_POINT('',(373.024272609134,289.481431763602,766.20332055189));
#52424=CARTESIAN_POINT('',(374.240895549687,287.456631165884,766.20332055189));
#52425=CARTESIAN_POINT('',(373.024272609134,289.481431763602,767.21932055189));
#52426=CARTESIAN_POINT('',(373.024272609134,289.481431763602,766.20332055189));
#52427=CARTESIAN_POINT('',(374.240895549687,287.456631165884,767.21932055189));
#52428=CARTESIAN_POINT('',(373.024272609134,289.481431763602,767.21932055189));
#52429=CARTESIAN_POINT('',(374.240895549687,287.456631165884,769.58152055189));
#52430=CARTESIAN_POINT('',(374.240895549687,287.456631165884,767.21932055189));
#52431=CARTESIAN_POINT('',(374.764174233796,286.58574918837,769.58152055189));
#52432=CARTESIAN_POINT('',(374.240895549687,287.456631165884,769.58152055189));
#52433=CARTESIAN_POINT('',(374.764174233796,286.58574918837,769.58152055189));
#52434=CARTESIAN_POINT('Origin',(375.846032486357,287.235795207705,769.60692055189));
#52435=CARTESIAN_POINT('',(374.764174233796,286.58574918837,769.58152055189));
#52436=CARTESIAN_POINT('Origin',(375.309842945387,286.56034918837,769.58152055189));
#52437=CARTESIAN_POINT('',(374.240895549687,287.456631165884,769.58152055189));
#52438=CARTESIAN_POINT('Origin',(375.322753802249,288.106677185218,769.60692055189));
#52439=CARTESIAN_POINT('',(374.240895549687,287.456631165884,767.21932055189));
#52440=CARTESIAN_POINT('Origin',(374.714442331972,287.431231165884,767.21932055189));
#52441=CARTESIAN_POINT('',(373.024272609134,289.481431763602,767.21932055189));
#52442=CARTESIAN_POINT('Origin',(373.841510050641,289.972477558598,767.24472055189));
#52443=CARTESIAN_POINT('',(373.024272609134,289.481431763602,766.20332055189));
#52444=CARTESIAN_POINT('Origin',(374.714442331972,287.431231165884,766.20332055189));
#52445=CARTESIAN_POINT('',(374.240895549687,287.456631165884,766.20332055189));
#52446=CARTESIAN_POINT('Origin',(375.322753802249,288.106677185218,766.22872055189));
#52447=CARTESIAN_POINT('',(374.240895549687,287.456631165884,763.84112055189));
#52448=CARTESIAN_POINT('Origin',(375.309842945387,286.56034918837,763.84112055189));
#52449=CARTESIAN_POINT('',(374.764174233796,286.58574918837,763.84112055189));
#52450=CARTESIAN_POINT('Origin',(375.846032486357,287.235795207705,766.22872055189));
#52451=CARTESIAN_POINT('Origin',(371.682267445708,285.281359303216,777.88732055189));
#52452=CARTESIAN_POINT('',(372.174522500189,285.281359303216,782.71332055189));
#52453=CARTESIAN_POINT('',(369.479533939566,290.107359303216,777.88732055189));
#52454=CARTESIAN_POINT('Ctrl Pts',(372.174522500189,285.281359303216,782.713320551891));
#52455=CARTESIAN_POINT('Ctrl Pts',(371.855654969792,285.899933374655,782.713320551891));
#52456=CARTESIAN_POINT('Ctrl Pts',(371.504957457388,286.55922733351,782.587944800608));
#52457=CARTESIAN_POINT('Ctrl Pts',(370.836280008275,287.77818982486,782.069981441115));
#52458=CARTESIAN_POINT('Ctrl Pts',(370.518643518802,288.338065228392,781.677437375128));
#52459=CARTESIAN_POINT('Ctrl Pts',(370.038186801395,289.16931580397,780.800937575508));
#52460=CARTESIAN_POINT('Ctrl Pts',(369.832513261077,289.517343365307,780.282107787414));
#52461=CARTESIAN_POINT('Ctrl Pts',(369.552676414556,289.986701593406,779.12761062806));
#52462=CARTESIAN_POINT('Ctrl Pts',(369.479533939566,290.107359303216,778.49142261233));
#52463=CARTESIAN_POINT('Ctrl Pts',(369.479533939566,290.107359303216,777.88732055189));
#52464=CARTESIAN_POINT('',(373.885000951849,285.281359303216,782.71332055189));
#52465=CARTESIAN_POINT('',(369.479533939566,290.107359303216,777.88732055189));
#52466=CARTESIAN_POINT('Origin',(371.278766994166,290.107359303215,732.42132055189));
#52467=CARTESIAN_POINT('',(369.479533939565,290.107359303215,686.95532055189));
#52468=CARTESIAN_POINT('',(369.479533939565,290.107359303215,686.95532055189));
#52469=CARTESIAN_POINT('',(369.479533939566,290.107359303216,777.88732055189));
#52470=CARTESIAN_POINT('Origin',(373.230354482257,288.354759303215,686.95532055189));
#52471=CARTESIAN_POINT('Origin',(298.461074890953,247.282959303211,686.955320551928));
#52472=CARTESIAN_POINT('Origin',(371.342244210912,286.576759303215,682.38332055189));
#52473=CARTESIAN_POINT('Origin',(298.461074890949,247.282959303209,682.383320551846));
#52474=CARTESIAN_POINT('Origin',(371.682267445712,209.284559303215,673.493320551891));
#52475=CARTESIAN_POINT('',(369.479533939571,204.458559303215,673.493320551891));
#52476=CARTESIAN_POINT('',(369.479533939571,204.458559303215,673.493320551891));
#52477=CARTESIAN_POINT('',(372.174522500193,209.284559303215,668.667320551891));
#52478=CARTESIAN_POINT('Ctrl Pts',(372.174522500194,209.284559303215,668.667320551891));
#52479=CARTESIAN_POINT('Ctrl Pts',(371.855654969797,208.665985231775,668.667320551891));
#52480=CARTESIAN_POINT('Ctrl Pts',(371.504957457392,208.00669127292,668.792696303173));
#52481=CARTESIAN_POINT('Ctrl Pts',(370.83628000828,206.78772878157,669.310659662666));
#52482=CARTESIAN_POINT('Ctrl Pts',(370.518643518807,206.227853378039,669.703203728653));
#52483=CARTESIAN_POINT('Ctrl Pts',(370.0381868014,205.39660280246,670.579703528274));
#52484=CARTESIAN_POINT('Ctrl Pts',(369.832513261083,205.048575241123,671.098533316367));
#52485=CARTESIAN_POINT('Ctrl Pts',(369.552676414562,204.579217013024,672.253030475721));
#52486=CARTESIAN_POINT('Ctrl Pts',(369.479533939571,204.458559303215,672.889218491451));
#52487=CARTESIAN_POINT('Ctrl Pts',(369.479533939571,204.458559303215,673.493320551891));
#52488=CARTESIAN_POINT('',(373.885000951854,209.284559303215,668.667320551891));
#52489=CARTESIAN_POINT('Origin',(399.770298695574,209.259159303217,668.667320551891));
#52490=CARTESIAN_POINT('',(376.030529085239,280.683959303215,668.66732055189));
#52491=CARTESIAN_POINT('',(427.366074890954,213.881959303219,668.667320551891));
#52492=CARTESIAN_POINT('Origin',(298.461074890952,247.28295930321,668.66732055189));
#52493=CARTESIAN_POINT('Origin',(399.770298695574,209.259159303218,782.713320551891));
#52494=CARTESIAN_POINT('Origin',(298.461074890953,247.282959303211,782.713320551891));
#52495=CARTESIAN_POINT('',(427.366074890955,213.88195930322,782.713320551891));
#52496=CARTESIAN_POINT('',(376.03052908524,280.683959303216,782.713320551891));
#52497=CARTESIAN_POINT('Origin',(371.342244210917,204.433159303215,686.955320551891));
#52498=CARTESIAN_POINT('Origin',(298.461074890911,247.282959303233,686.955320551891));
#52499=CARTESIAN_POINT('Origin',(371.342244210917,204.433159303215,682.383320551891));
#52500=CARTESIAN_POINT('',(369.479533939571,204.458559303215,682.383320551891));
#52501=CARTESIAN_POINT('Origin',(298.461074890906,247.282959303239,682.383320551943));
#52502=CARTESIAN_POINT('',(369.479533939571,204.458559303215,682.383320551891));
#52503=CARTESIAN_POINT('Origin',(371.278766994171,204.458559303215,677.938320551891));
#52504=CARTESIAN_POINT('',(369.479533939572,204.458559303215,673.493320551891));
#52505=CARTESIAN_POINT('Origin',(427.391474890954,213.881959303219,725.690320551891));
#52506=CARTESIAN_POINT('',(405.141074890954,213.881959303218,736.86632055189));
#52507=CARTESIAN_POINT('Origin',(405.141074890955,213.881959303218,725.690320551891));
#52508=CARTESIAN_POINT('Origin',(427.39147489095,280.683959303219,725.69032055189));
#52509=CARTESIAN_POINT('Origin',(375.3121954222,206.465585535989,725.207720551891));
#52510=CARTESIAN_POINT('',(374.240895549693,207.109287440548,722.820120551891));
#52511=CARTESIAN_POINT('',(374.240895549693,207.109287440548,722.820120551891));
#52512=CARTESIAN_POINT('',(374.240895549692,207.109287440548,725.182320551891));
#52513=CARTESIAN_POINT('',(374.240895549692,207.109287440548,725.182320551891));
#52514=CARTESIAN_POINT('',(374.240895549692,207.109287440548,725.182320551891));
#52515=CARTESIAN_POINT('Origin',(374.703883951924,204.111811032767,725.182320551891));
#52516=CARTESIAN_POINT('',(373.02427260914,205.084486842829,725.182320551891));
#52517=CARTESIAN_POINT('',(373.02427260914,205.084486842829,725.182320551891));
#52518=CARTESIAN_POINT('',(373.02427260914,205.084486842829,725.182320551891));
#52519=CARTESIAN_POINT('Origin',(375.290800739153,206.136611630486,722.820120551891));
#52520=CARTESIAN_POINT('',(374.764174233801,207.980169418061,722.820120551891));
#52521=CARTESIAN_POINT('',(374.764174233801,207.980169418061,722.820120551891));
#52522=CARTESIAN_POINT('',(374.240895549693,207.109287440548,722.820120551891));
#52523=CARTESIAN_POINT('Origin',(373.82220154347,204.605042769408,726.223720551891));
#52524=CARTESIAN_POINT('',(373.02427260914,205.084486842829,726.198320551891));
#52525=CARTESIAN_POINT('',(373.02427260914,205.084486842829,726.198320551891));
#52526=CARTESIAN_POINT('',(373.02427260914,205.084486842829,726.198320551891));
#52527=CARTESIAN_POINT('Origin',(376.408895294708,205.623249236658,726.198320551891));
#52528=CARTESIAN_POINT('',(374.240895549692,207.109287440548,726.198320551891));
#52529=CARTESIAN_POINT('',(374.240895549692,207.109287440548,726.198320551891));
#52530=CARTESIAN_POINT('',(374.240895549692,207.109287440548,726.198320551891));
#52531=CARTESIAN_POINT('Origin',(375.3121954222,206.465585535989,728.585920551891));
#52532=CARTESIAN_POINT('',(374.240895549693,207.109287440548,728.560520551891));
#52533=CARTESIAN_POINT('',(374.240895549693,207.109287440548,728.560520551891));
#52534=CARTESIAN_POINT('',(374.240895549693,207.109287440548,728.560520551891));
#52535=CARTESIAN_POINT('Origin',(375.290800739153,206.136611630486,728.560520551891));
#52536=CARTESIAN_POINT('',(374.764174233801,207.980169418061,728.560520551891));
#52537=CARTESIAN_POINT('',(374.764174233801,207.980169418061,728.560520551891));
#52538=CARTESIAN_POINT('',(374.764174233801,207.980169418061,728.560520551891));
#52539=CARTESIAN_POINT('Origin',(375.835474106309,207.336467513502,728.585920551891));
#52540=CARTESIAN_POINT('',(374.764174233801,207.980169418061,726.198320551891));
#52541=CARTESIAN_POINT('',(374.764174233801,207.980169418061,726.198320551891));
#52542=CARTESIAN_POINT('',(374.764174233801,207.980169418061,726.198320551891));
#52543=CARTESIAN_POINT('Origin',(376.160751551484,206.667365608943,726.198320551891));
#52544=CARTESIAN_POINT('',(375.980797174353,210.00497001578,726.198320551891));
#52545=CARTESIAN_POINT('',(375.980797174353,210.00497001578,726.198320551891));
#52546=CARTESIAN_POINT('',(375.980797174353,210.00497001578,726.198320551891));
#52547=CARTESIAN_POINT('Origin',(376.788427340408,209.519696854259,726.223720551891));
#52548=CARTESIAN_POINT('',(375.980797174353,210.00497001578,725.182320551891));
#52549=CARTESIAN_POINT('',(375.980797174353,210.00497001578,725.182320551891));
#52550=CARTESIAN_POINT('',(375.980797174353,210.00497001578,725.182320551891));
#52551=CARTESIAN_POINT('Origin',(377.582728869166,208.348867812361,725.182320551891));
#52552=CARTESIAN_POINT('',(374.764174233801,207.980169418061,725.182320551891));
#52553=CARTESIAN_POINT('',(374.764174233801,207.980169418061,725.182320551891));
#52554=CARTESIAN_POINT('',(374.764174233801,207.980169418061,725.182320551891));
#52555=CARTESIAN_POINT('Origin',(405.141074890954,216.421959303218,725.69032055189));
#52556=CARTESIAN_POINT('',(405.141074890954,218.961959303218,736.86632055189));
#52557=CARTESIAN_POINT('',(405.141074890954,216.421959303218,736.86632055189));
#52558=CARTESIAN_POINT('Origin',(405.141074890954,218.961959303218,725.690320551891));
#52559=CARTESIAN_POINT('Origin',(416.342474890954,218.961959303218,725.690320551891));
#52560=CARTESIAN_POINT('Origin',(374.502534891747,207.544728429304,728.585920551891));
#52561=CARTESIAN_POINT('',(374.764174233801,207.980169418061,722.820120551891));
#52562=CARTESIAN_POINT('Origin',(375.835474106309,207.336467513502,725.207720551891));
#52563=CARTESIAN_POINT('Origin',(371.183235802879,285.026754071854,725.69032055189));
#52564=CARTESIAN_POINT('',(376.340705928608,287.533024998432,728.56052055189));
#52565=CARTESIAN_POINT('Origin',(371.444875144932,284.591313083098,725.69032055189));
#52566=CARTESIAN_POINT('',(375.8174272445,288.403906975945,728.56052055189));
#52567=CARTESIAN_POINT('Origin',(371.183235802879,285.026754071854,728.560520551888));
#52568=CARTESIAN_POINT('',(376.383495294702,288.744034975002,726.19832055189));
#52569=CARTESIAN_POINT('Origin',(370.921596460824,285.46219506061,725.69032055189));
#52570=CARTESIAN_POINT('',(374.600804303947,290.428707573663,726.19832055189));
#52571=CARTESIAN_POINT('Origin',(371.183235802879,285.026754071854,726.198320551891));
#52572=CARTESIAN_POINT('',(374.600804303947,290.428707573663,725.18232055189));
#52573=CARTESIAN_POINT('Origin',(369.704973520274,287.486995658328,725.69032055189));
#52574=CARTESIAN_POINT('',(376.383495294702,288.744034975002,725.18232055189));
#52575=CARTESIAN_POINT('Origin',(371.183235802879,285.026754071854,725.18232055189));
#52576=CARTESIAN_POINT('',(375.8174272445,288.403906975945,722.82012055189));
#52577=CARTESIAN_POINT('Origin',(370.921596460822,285.462195060611,725.690320551891));
#52578=CARTESIAN_POINT('',(376.340705928608,287.533024998432,722.82012055189));
#52579=CARTESIAN_POINT('Origin',(371.183235802883,285.026754071857,722.820120551892));
#52580=CARTESIAN_POINT('',(376.906773978811,287.873152997488,725.18232055189));
#52581=CARTESIAN_POINT('Origin',(371.444875144934,284.591313083099,725.69032055189));
#52582=CARTESIAN_POINT('Origin',(371.183235802878,285.026754071854,725.18232055189));
#52583=CARTESIAN_POINT('Origin',(374.502534891741,287.021190177127,728.58592055189));
#52584=CARTESIAN_POINT('',(374.764174233796,286.58574918837,725.18232055189));
#52585=CARTESIAN_POINT('',(375.980797174348,284.560948590652,725.18232055189));
#52586=CARTESIAN_POINT('',(374.764174233796,286.58574918837,722.82012055189));
#52587=CARTESIAN_POINT('',(374.764174233796,286.58574918837,725.18232055189));
#52588=CARTESIAN_POINT('',(374.240895549687,287.456631165883,722.82012055189));
#52589=CARTESIAN_POINT('',(374.764174233796,286.58574918837,722.82012055189));
#52590=CARTESIAN_POINT('',(374.240895549687,287.456631165883,725.18232055189));
#52591=CARTESIAN_POINT('',(374.240895549687,287.456631165883,722.82012055189));
#52592=CARTESIAN_POINT('',(373.024272609134,289.481431763602,725.18232055189));
#52593=CARTESIAN_POINT('',(374.240895549687,287.456631165883,725.18232055189));
#52594=CARTESIAN_POINT('',(373.024272609134,289.481431763602,726.19832055189));
#52595=CARTESIAN_POINT('',(373.024272609134,289.481431763602,725.18232055189));
#52596=CARTESIAN_POINT('',(374.240895549687,287.456631165883,726.19832055189));
#52597=CARTESIAN_POINT('',(373.024272609134,289.481431763602,726.19832055189));
#52598=CARTESIAN_POINT('',(374.240895549687,287.456631165883,728.56052055189));
#52599=CARTESIAN_POINT('',(374.240895549687,287.456631165883,726.19832055189));
#52600=CARTESIAN_POINT('',(374.764174233796,286.58574918837,728.56052055189));
#52601=CARTESIAN_POINT('',(374.240895549687,287.456631165883,728.56052055189));
#52602=CARTESIAN_POINT('',(374.764174233796,286.58574918837,728.56052055189));
#52603=CARTESIAN_POINT('Origin',(375.835474106303,287.229451092929,728.58592055189));
#52604=CARTESIAN_POINT('',(374.764174233796,286.58574918837,728.56052055189));
#52605=CARTESIAN_POINT('Origin',(375.290800739148,286.56034918837,728.56052055189));
#52606=CARTESIAN_POINT('',(374.240895549687,287.456631165883,728.56052055189));
#52607=CARTESIAN_POINT('Origin',(375.312195422195,288.100333070442,728.58592055189));
#52608=CARTESIAN_POINT('',(374.240895549687,287.456631165883,726.19832055189));
#52609=CARTESIAN_POINT('Origin',(374.703883951918,287.431231165883,726.19832055189));
#52610=CARTESIAN_POINT('',(373.024272609134,289.481431763602,726.19832055189));
#52611=CARTESIAN_POINT('Origin',(373.831902775189,289.966704925123,726.22372055189));
#52612=CARTESIAN_POINT('',(373.024272609134,289.481431763602,725.18232055189));
#52613=CARTESIAN_POINT('Origin',(376.408895294702,288.942669369774,725.18232055189));
#52614=CARTESIAN_POINT('',(374.240895549687,287.456631165883,725.18232055189));
#52615=CARTESIAN_POINT('Origin',(375.312195422195,288.100333070442,725.20772055189));
#52616=CARTESIAN_POINT('',(374.240895549687,287.456631165883,722.82012055189));
#52617=CARTESIAN_POINT('Origin',(375.290800739148,286.56034918837,722.82012055189));
#52618=CARTESIAN_POINT('',(374.764174233796,286.58574918837,722.82012055189));
#52619=CARTESIAN_POINT('Origin',(375.835474106303,287.229451092929,725.20772055189));
#52620=CARTESIAN_POINT('',(374.764174233796,286.58574918837,725.18232055189));
#52621=CARTESIAN_POINT('Origin',(376.160751551479,284.535548590652,725.18232055189));
#52622=CARTESIAN_POINT('Origin',(298.461074890946,338.240359303211,792.23832055189));
#52623=CARTESIAN_POINT('',(389.393074890952,247.282959303217,792.238320551891));
#52624=CARTESIAN_POINT('Origin',(298.461074890952,247.282959303211,792.238320551891));
#52625=CARTESIAN_POINT('',(215.530074890953,247.282959303205,792.238320551891));
#52626=CARTESIAN_POINT('Origin',(298.461074890953,247.282959303211,792.238320551891));
#52627=CARTESIAN_POINT('Origin',(224.281150396699,301.177829172505,810.450120551891));
#52628=CARTESIAN_POINT('',(222.545282322562,297.337140574242,810.450120551891));
#52629=CARTESIAN_POINT('',(227.397449580236,304.015575862807,810.450120551891));
#52630=CARTESIAN_POINT('Ctrl Pts',(222.545282322562,297.337140574242,810.450120551891));
#52631=CARTESIAN_POINT('Ctrl Pts',(222.545282322562,297.337140574242,810.968455084256));
#52632=CARTESIAN_POINT('Ctrl Pts',(222.602220666962,297.42383385282,811.521290446934));
#52633=CARTESIAN_POINT('Ctrl Pts',(222.83552034229,297.775023669248,812.538200080674));
#52634=CARTESIAN_POINT('Ctrl Pts',(223.01208514873,298.039367523769,813.002280383611));
#52635=CARTESIAN_POINT('Ctrl Pts',(223.423802412012,298.646085838271,813.735127146313));
#52636=CARTESIAN_POINT('Ctrl Pts',(223.686446736859,299.028898397941,814.052768044994));
#52637=CARTESIAN_POINT('Ctrl Pts',(224.269877629636,299.861980569393,814.474016718618));
#52638=CARTESIAN_POINT('Ctrl Pts',(224.590872208263,300.312106479352,814.577620551891));
#52639=CARTESIAN_POINT('Ctrl Pts',(225.200210908629,301.150789249978,814.577620551891));
#52640=CARTESIAN_POINT('Ctrl Pts',(225.52911330855,301.595169791463,814.474016718618));
#52641=CARTESIAN_POINT('Ctrl Pts',(226.141131475408,302.407482092536,814.052768044994));
#52642=CARTESIAN_POINT('Ctrl Pts',(226.424046294948,302.775567275748,813.735127146313));
#52643=CARTESIAN_POINT('Ctrl Pts',(226.873842070279,303.354619931843,813.002280383611));
#52644=CARTESIAN_POINT('Ctrl Pts',(227.070686489865,303.604229784962,812.538200080674));
#52645=CARTESIAN_POINT('Ctrl Pts',(227.332594288776,303.93463458296,811.521290446934));
#52646=CARTESIAN_POINT('Ctrl Pts',(227.397449580236,304.015575862807,810.968455084256));
#52647=CARTESIAN_POINT('Ctrl Pts',(227.397449580236,304.015575862807,810.450120551891));
#52648=CARTESIAN_POINT('',(226.017018470835,305.018517770768,810.450120551891));
#52649=CARTESIAN_POINT('',(226.707234025536,304.517046816788,810.450120551891));
#52650=CARTESIAN_POINT('',(223.590934913942,301.679300225506,806.322620551891));
#52651=CARTESIAN_POINT('Origin',(223.590934841999,301.679300126486,810.450120551891));
#52652=CARTESIAN_POINT('Origin',(223.590934841999,301.679300126486,810.450120551891));
#52653=CARTESIAN_POINT('Ctrl Pts',(227.397449580236,304.015575862807,810.450120551891));
#52654=CARTESIAN_POINT('Ctrl Pts',(227.397449580236,304.015575862807,809.931786019525));
#52655=CARTESIAN_POINT('Ctrl Pts',(227.332594288776,303.93463458296,809.378950656848));
#52656=CARTESIAN_POINT('Ctrl Pts',(227.070686489865,303.604229784962,808.362041023107));
#52657=CARTESIAN_POINT('Ctrl Pts',(226.873842070279,303.354619931843,807.89796072017));
#52658=CARTESIAN_POINT('Ctrl Pts',(226.424046294948,302.775567275748,807.165113957469));
#52659=CARTESIAN_POINT('Ctrl Pts',(226.141131475408,302.407482092536,806.847473058788));
#52660=CARTESIAN_POINT('Ctrl Pts',(225.52911330855,301.595169791463,806.426224385163));
#52661=CARTESIAN_POINT('Ctrl Pts',(225.200210908628,301.150789249978,806.322620551891));
#52662=CARTESIAN_POINT('Ctrl Pts',(224.590872208263,300.312106479352,806.322620551891));
#52663=CARTESIAN_POINT('Ctrl Pts',(224.269877629636,299.861980569393,806.426224385163));
#52664=CARTESIAN_POINT('Ctrl Pts',(223.686446736859,299.028898397941,806.847473058788));
#52665=CARTESIAN_POINT('Ctrl Pts',(223.423802412012,298.646085838271,807.165113957469));
#52666=CARTESIAN_POINT('Ctrl Pts',(223.01208514873,298.039367523769,807.89796072017));
#52667=CARTESIAN_POINT('Ctrl Pts',(222.83552034229,297.775023669248,808.362041023107));
#52668=CARTESIAN_POINT('Ctrl Pts',(222.602220666962,297.42383385282,809.378950656848));
#52669=CARTESIAN_POINT('Ctrl Pts',(222.545282322562,297.337140574242,809.931786019525));
#52670=CARTESIAN_POINT('Ctrl Pts',(222.545282322562,297.337140574242,810.450120551891));
#52671=CARTESIAN_POINT('Origin',(298.461074890959,153.429959303211,810.460151039948));
#52672=CARTESIAN_POINT('',(298.469433631005,153.429959303211,810.450120551892));
#52673=CARTESIAN_POINT('',(298.461074893041,153.429959303211,810.458479291938));
#52674=CARTESIAN_POINT('Origin',(298.461074890959,153.429959303211,810.450120551892));
#52675=CARTESIAN_POINT('Origin',(298.461074890959,153.429959303211,810.450120551892));
#52676=CARTESIAN_POINT('Origin',(298.461074890958,155.591530062517,810.450120551892));
#52677=CARTESIAN_POINT('',(302.588574890958,156.444683407254,810.450120551892));
#52678=CARTESIAN_POINT('',(294.333574890958,156.444683407254,810.450120551892));
#52679=CARTESIAN_POINT('Ctrl Pts',(302.588574890958,156.444683407255,810.450120551892));
#52680=CARTESIAN_POINT('Ctrl Pts',(302.588574890958,156.444683407255,810.968455084257));
#52681=CARTESIAN_POINT('Ctrl Pts',(302.484971036162,156.439790464884,811.521290446935));
#52682=CARTESIAN_POINT('Ctrl Pts',(302.063722397899,156.422109672155,812.538200080675));
#52683=CARTESIAN_POINT('Ctrl Pts',(301.746081537933,156.409576181953,813.002280383612));
#52684=CARTESIAN_POINT('Ctrl Pts',(301.013234775231,156.386042367265,813.735127146314));
#52685=CARTESIAN_POINT('Ctrl Pts',(300.549154448054,156.373514512576,814.052768044995));
#52686=CARTESIAN_POINT('Ctrl Pts',(299.532244739133,156.355846605548,814.474016718619));
#52687=CARTESIAN_POINT('Ctrl Pts',(298.979409348984,156.350959303211,814.577620551892));
#52688=CARTESIAN_POINT('Ctrl Pts',(297.942740432933,156.350959303211,814.577620551892));
#52689=CARTESIAN_POINT('Ctrl Pts',(297.389905042784,156.355846605548,814.474016718619));
#52690=CARTESIAN_POINT('Ctrl Pts',(296.372995333862,156.373514512576,814.052768044995));
#52691=CARTESIAN_POINT('Ctrl Pts',(295.908915006686,156.386042367265,813.735127146314));
#52692=CARTESIAN_POINT('Ctrl Pts',(295.176068243984,156.409576181952,813.002280383612));
#52693=CARTESIAN_POINT('Ctrl Pts',(294.858427384018,156.422109672155,812.538200080675));
#52694=CARTESIAN_POINT('Ctrl Pts',(294.437178745755,156.439790464884,811.521290446935));
#52695=CARTESIAN_POINT('Ctrl Pts',(294.333574890958,156.444683407254,810.968455084257));
#52696=CARTESIAN_POINT('Ctrl Pts',(294.333574890958,156.444683407254,810.450120551892));
#52697=CARTESIAN_POINT('',(294.333574890958,154.738376717779,810.450120550069));
#52698=CARTESIAN_POINT('',(294.333574890958,155.591530062517,810.450120551892));
#52699=CARTESIAN_POINT('',(298.46107489266,154.73837671778,814.577620551892));
#52700=CARTESIAN_POINT('Origin',(298.461074890958,154.73837671778,810.450120551892));
#52701=CARTESIAN_POINT('Origin',(298.461074890958,154.73837671778,810.450120551892));
#52702=CARTESIAN_POINT('Ctrl Pts',(294.333574890958,156.444683407254,810.450120551892));
#52703=CARTESIAN_POINT('Ctrl Pts',(294.333574890958,156.444683407254,809.931786019526));
#52704=CARTESIAN_POINT('Ctrl Pts',(294.437178745755,156.439790464884,809.378950656849));
#52705=CARTESIAN_POINT('Ctrl Pts',(294.858427384018,156.422109672155,808.362041023108));
#52706=CARTESIAN_POINT('Ctrl Pts',(295.176068243984,156.409576181952,807.897960720171));
#52707=CARTESIAN_POINT('Ctrl Pts',(295.908915006686,156.386042367265,807.16511395747));
#52708=CARTESIAN_POINT('Ctrl Pts',(296.372995333862,156.373514512576,806.847473058789));
#52709=CARTESIAN_POINT('Ctrl Pts',(297.389905042784,156.355846605548,806.426224385164));
#52710=CARTESIAN_POINT('Ctrl Pts',(297.942740432933,156.350959303211,806.322620551892));
#52711=CARTESIAN_POINT('Ctrl Pts',(298.979409348984,156.350959303211,806.322620551892));
#52712=CARTESIAN_POINT('Ctrl Pts',(299.532244739133,156.355846605548,806.426224385164));
#52713=CARTESIAN_POINT('Ctrl Pts',(300.549154448054,156.373514512576,806.847473058789));
#52714=CARTESIAN_POINT('Ctrl Pts',(301.013234775231,156.386042367265,807.165113957469));
#52715=CARTESIAN_POINT('Ctrl Pts',(301.746081537933,156.409576181953,807.897960720171));
#52716=CARTESIAN_POINT('Ctrl Pts',(302.063722397899,156.422109672155,808.362041023108));
#52717=CARTESIAN_POINT('Ctrl Pts',(302.484971036162,156.439790464884,809.378950656849));
#52718=CARTESIAN_POINT('Ctrl Pts',(302.588574890958,156.444683407255,809.931786019526));
#52719=CARTESIAN_POINT('Ctrl Pts',(302.588574890958,156.444683407255,810.450120551892));
#52720=CARTESIAN_POINT('Origin',(379.74015711233,294.209459303217,810.460151039946));
#52721=CARTESIAN_POINT('',(379.735977742307,294.21669818444,810.45012055189));
#52722=CARTESIAN_POINT('',(379.744336482353,294.202220421994,810.450120664857));
#52723=CARTESIAN_POINT('Origin',(379.74015711233,294.209459303217,810.45012055189));
#52724=CARTESIAN_POINT('',(379.740157117303,294.209459294603,810.458479291936));
#52725=CARTESIAN_POINT('Ctrl Pts',(379.740157117303,294.209459294603,810.458479291936));
#52726=CARTESIAN_POINT('Ctrl Pts',(379.738425964101,294.212457739905,810.458479296056));
#52727=CARTESIAN_POINT('Ctrl Pts',(379.737201853204,294.214577962173,810.456031077176));
#52728=CARTESIAN_POINT('Ctrl Pts',(379.735977742307,294.21669818444,810.453582858295));
#52729=CARTESIAN_POINT('Ctrl Pts',(379.735977742307,294.21669818444,810.45012055189));
#52730=CARTESIAN_POINT('Origin',(379.74015711233,294.209459303217,810.45012055189));
#52731=CARTESIAN_POINT('Origin',(377.868181922694,293.128673923564,810.45012055189));
#52732=CARTESIAN_POINT('',(375.065579452827,296.276617105315,810.45012055189));
#52733=CARTESIAN_POINT('',(379.193079452828,289.127577397075,810.45012055189));
#52734=CARTESIAN_POINT('Ctrl Pts',(375.065579452827,296.276617105315,810.45012055189));
#52735=CARTESIAN_POINT('Ctrl Pts',(375.065579452827,296.276617105315,810.968455084256));
#52736=CARTESIAN_POINT('Ctrl Pts',(375.121618792617,296.189340006316,811.521290446933));
#52737=CARTESIAN_POINT('Ctrl Pts',(375.347555127411,295.833368380635,812.538200080674));
#52738=CARTESIAN_POINT('Ctrl Pts',(375.517229878308,295.564550071726,813.002280383611));
#52739=CARTESIAN_POINT('Ctrl Pts',(375.904034141026,294.941653065489,813.735127146312));
#52740=CARTESIAN_POINT('Ctrl Pts',(376.14692374503,294.546011640102,814.052768044993));
#52741=CARTESIAN_POINT('Ctrl Pts',(376.670679455809,293.674175952335,814.474016718618));
#52742=CARTESIAN_POINT('Ctrl Pts',(376.951329678863,293.197850111524,814.57762055189));
#52743=CARTESIAN_POINT('Ctrl Pts',(377.469664136889,292.300068494909,814.57762055189));
#52744=CARTESIAN_POINT('Ctrl Pts',(377.741849303983,291.818855351761,814.474016718618));
#52745=CARTESIAN_POINT('Ctrl Pts',(378.235003302126,290.929351756966,814.052768044993));
#52746=CARTESIAN_POINT('Ctrl Pts',(378.456194025299,290.52118247689,813.735127146313));
#52747=CARTESIAN_POINT('Ctrl Pts',(378.802236525283,289.874751655965,813.002280383611));
#52748=CARTESIAN_POINT('Ctrl Pts',(378.950202634352,289.593399856854,812.538200080674));
#52749=CARTESIAN_POINT('Ctrl Pts',(379.145514937821,289.219747438444,811.521290446933));
#52750=CARTESIAN_POINT('Ctrl Pts',(379.193079452828,289.127577397075,810.968455084256));
#52751=CARTESIAN_POINT('Ctrl Pts',(379.193079452828,289.127577397075,810.45012055189));
#52752=CARTESIAN_POINT('',(380.67078439256,289.980730741812,810.45012055189));
#52753=CARTESIAN_POINT('',(379.931931922694,289.554154069444,810.45012055189));
#52754=CARTESIAN_POINT('Origin',(378.60703439256,293.555250595932,810.45012055189));
#52755=CARTESIAN_POINT('Ctrl Pts',(379.193079452828,289.127577397075,810.45012055189));
#52756=CARTESIAN_POINT('Ctrl Pts',(379.193079452828,289.127577397075,809.931786019525));
#52757=CARTESIAN_POINT('Ctrl Pts',(379.145514937821,289.219747438444,809.378950656847));
#52758=CARTESIAN_POINT('Ctrl Pts',(378.950202634352,289.593399856854,808.362041023107));
#52759=CARTESIAN_POINT('Ctrl Pts',(378.802236525283,289.874751655965,807.89796072017));
#52760=CARTESIAN_POINT('Ctrl Pts',(378.456194025299,290.52118247689,807.165113957468));
#52761=CARTESIAN_POINT('Ctrl Pts',(378.235003302126,290.929351756966,806.847473058788));
#52762=CARTESIAN_POINT('Ctrl Pts',(377.741849303983,291.818855351761,806.426224385163));
#52763=CARTESIAN_POINT('Ctrl Pts',(377.469664136889,292.300068494909,806.32262055189));
#52764=CARTESIAN_POINT('Ctrl Pts',(376.951329678863,293.197850111524,806.32262055189));
#52765=CARTESIAN_POINT('Ctrl Pts',(376.670679455809,293.674175952335,806.426224385163));
#52766=CARTESIAN_POINT('Ctrl Pts',(376.14692374503,294.546011640102,806.847473058788));
#52767=CARTESIAN_POINT('Ctrl Pts',(375.904034141026,294.941653065489,807.165113957468));
#52768=CARTESIAN_POINT('Ctrl Pts',(375.517229878308,295.564550071726,807.89796072017));
#52769=CARTESIAN_POINT('Ctrl Pts',(375.347555127411,295.833368380635,808.362041023107));
#52770=CARTESIAN_POINT('Ctrl Pts',(375.121618792617,296.189340006316,809.378950656847));
#52771=CARTESIAN_POINT('Ctrl Pts',(375.065579452827,296.276617105315,809.931786019525));
#52772=CARTESIAN_POINT('Ctrl Pts',(375.065579452827,296.276617105315,810.45012055189));
#52773=CARTESIAN_POINT('Ctrl Pts',(379.744340671372,294.202222954448,810.450120664856));
#52774=CARTESIAN_POINT('Ctrl Pts',(379.744340671258,294.202222954382,810.458479276214));
#52775=CARTESIAN_POINT('Ctrl Pts',(379.740161365609,294.209461724175,810.458479276214));
#52776=CARTESIAN_POINT('Ctrl Pts',(379.735982059961,294.216700493969,810.458479276214));
#52777=CARTESIAN_POINT('Ctrl Pts',(379.735982060075,294.216700494035,810.450120664856));
#52778=CARTESIAN_POINT('Ctrl Pts',(379.735982060189,294.216700494101,810.441762053498));
#52779=CARTESIAN_POINT('Ctrl Pts',(379.740161365838,294.209461724307,810.441762053498));
#52780=CARTESIAN_POINT('Ctrl Pts',(379.744340671486,294.202222954514,810.441762053498));
#52781=CARTESIAN_POINT('Ctrl Pts',(379.744340671372,294.202222954448,810.450120664856));
#52782=CARTESIAN_POINT('Ctrl Pts',(380.878029350219,292.238616625522,810.450120664856));
#52783=CARTESIAN_POINT('Ctrl Pts',(380.87802931912,292.238616607567,812.725856579518));
#52784=CARTESIAN_POINT('Ctrl Pts',(379.740161370053,294.209461726741,812.725856579518));
#52785=CARTESIAN_POINT('Ctrl Pts',(378.602293420985,296.180306845914,812.725856579518));
#52786=CARTESIAN_POINT('Ctrl Pts',(378.602293452084,296.180306863869,810.450120664856));
#52787=CARTESIAN_POINT('Ctrl Pts',(378.602293483183,296.180306881824,808.174384750194));
#52788=CARTESIAN_POINT('Ctrl Pts',(379.74016143225,294.20946176265,808.174384750194));
#52789=CARTESIAN_POINT('Ctrl Pts',(380.878029381317,292.238616643477,808.174384750194));
#52790=CARTESIAN_POINT('Ctrl Pts',(380.878029350219,292.238616625522,810.450120664856));
#52791=CARTESIAN_POINT('Ctrl Pts',(380.670784378444,289.980730588271,810.45012064421));
#52792=CARTESIAN_POINT('Ctrl Pts',(380.670784322041,289.980730555706,814.577620745582));
#52793=CARTESIAN_POINT('Ctrl Pts',(378.607034286343,293.55525050627,814.577620745582));
#52794=CARTESIAN_POINT('Ctrl Pts',(376.543284250646,297.129770456834,814.577620745582));
#52795=CARTESIAN_POINT('Ctrl Pts',(376.54328430705,297.129770489399,810.45012064421));
#52796=CARTESIAN_POINT('Ctrl Pts',(376.543284363453,297.129770521964,806.322620542838));
#52797=CARTESIAN_POINT('Ctrl Pts',(378.607034399151,293.5552505714,806.322620542838));
#52798=CARTESIAN_POINT('Ctrl Pts',(380.670784434848,289.980730620835,806.322620542838));
#52799=CARTESIAN_POINT('Ctrl Pts',(380.670784378444,289.980730588271,810.45012064421));
#52800=CARTESIAN_POINT('Origin',(373.56256640991,290.633173806373,810.450120552221));
#52801=CARTESIAN_POINT('Origin',(222.532402917877,302.448368586612,810.460151039947));
#52802=CARTESIAN_POINT('',(222.527485814252,302.441609100606,810.450120551891));
#52803=CARTESIAN_POINT('',(222.532399041916,302.448371578067,810.441761677343));
#52804=CARTESIAN_POINT('Origin',(222.532399042082,302.44837157828,810.450120559565));
#52805=CARTESIAN_POINT('Origin',(222.532399042082,302.44837157828,810.450120559565));
#52806=CARTESIAN_POINT('Ctrl Pts',(222.532399041916,302.448371578067,810.441761677343));
#52807=CARTESIAN_POINT('Ctrl Pts',(222.537312269244,302.455134055051,810.441761677354));
#52808=CARTESIAN_POINT('Ctrl Pts',(222.537312269244,302.455134055037,810.450120558723));
#52809=CARTESIAN_POINT('Ctrl Pts',(222.537312269244,302.455134055024,810.458479440092));
#52810=CARTESIAN_POINT('Ctrl Pts',(222.532399041916,302.44837157804,810.458479440081));
#52811=CARTESIAN_POINT('Ctrl Pts',(222.527485814588,302.441609101056,810.45847944007));
#52812=CARTESIAN_POINT('Ctrl Pts',(222.527485814588,302.44160910107,810.450120558701));
#52813=CARTESIAN_POINT('Ctrl Pts',(222.527485814588,302.441609101083,810.441761677332));
#52814=CARTESIAN_POINT('Ctrl Pts',(222.532399041916,302.448371578067,810.441761677343));
#52815=CARTESIAN_POINT('Ctrl Pts',(222.532399078261,302.448371555347,808.17438450705));
#52816=CARTESIAN_POINT('Ctrl Pts',(223.870043204029,304.289480669341,808.174384510044));
#52817=CARTESIAN_POINT('Ctrl Pts',(223.870043204029,304.289480665641,810.450120561705));
#52818=CARTESIAN_POINT('Ctrl Pts',(223.870043204029,304.289480661941,812.725856613366));
#52819=CARTESIAN_POINT('Ctrl Pts',(222.532399078261,302.448371547948,812.725856610373));
#52820=CARTESIAN_POINT('Ctrl Pts',(221.194754952494,300.607262433954,812.72585660738));
#52821=CARTESIAN_POINT('Ctrl Pts',(221.194754952494,300.607262437653,810.450120555719));
#52822=CARTESIAN_POINT('Ctrl Pts',(221.194754952494,300.607262441353,808.174384504057));
#52823=CARTESIAN_POINT('Ctrl Pts',(222.532399078261,302.448371555347,808.17438450705));
#52824=CARTESIAN_POINT('Ctrl Pts',(223.59093498133,301.679300175303,806.322620432803));
#52825=CARTESIAN_POINT('Ctrl Pts',(226.017018749623,305.018517872351,806.322620438231));
#52826=CARTESIAN_POINT('Ctrl Pts',(226.017018749623,305.018517865641,810.45012056289));
#52827=CARTESIAN_POINT('Ctrl Pts',(226.017018749623,305.018517858931,814.577620687549));
#52828=CARTESIAN_POINT('Ctrl Pts',(223.59093498133,301.679300161882,814.57762068212));
#52829=CARTESIAN_POINT('Ctrl Pts',(221.164851213037,298.340082464834,814.577620676692));
#52830=CARTESIAN_POINT('Ctrl Pts',(221.164851213037,298.340082471544,810.450120552033));
#52831=CARTESIAN_POINT('Ctrl Pts',(221.164851213037,298.340082478254,806.322620427374));
#52832=CARTESIAN_POINT('Ctrl Pts',(223.59093498133,301.679300175303,806.322620432803));
#52833=CARTESIAN_POINT('Origin',(228.30724165054,298.25270265549,810.441761811954));
#52834=CARTESIAN_POINT('Ctrl Pts',(298.461074893041,153.429954409153,810.458479290597));
#52835=CARTESIAN_POINT('Ctrl Pts',(298.469433631005,153.429954409156,810.458479290597));
#52836=CARTESIAN_POINT('Ctrl Pts',(298.469433631005,153.429954409155,810.450120552633));
#52837=CARTESIAN_POINT('Ctrl Pts',(298.469433631005,153.429954409154,810.441761814669));
#52838=CARTESIAN_POINT('Ctrl Pts',(298.461074893041,153.429954409152,810.441761814669));
#52839=CARTESIAN_POINT('Ctrl Pts',(298.452716155077,153.429954409149,810.441761814669));
#52840=CARTESIAN_POINT('Ctrl Pts',(298.452716155077,153.42995440915,810.450120552633));
#52841=CARTESIAN_POINT('Ctrl Pts',(298.452716155077,153.429954409151,810.458479290597));
#52842=CARTESIAN_POINT('Ctrl Pts',(298.461074893041,153.429954409153,810.458479290597));
#52843=CARTESIAN_POINT('Ctrl Pts',(298.461074893041,153.429954408731,812.725856457163));
#52844=CARTESIAN_POINT('Ctrl Pts',(300.736810797571,153.429954409393,812.725856457163));
#52845=CARTESIAN_POINT('Ctrl Pts',(300.736810797571,153.429954409158,810.450120552633));
#52846=CARTESIAN_POINT('Ctrl Pts',(300.736810797571,153.429954408923,808.174384648103));
#52847=CARTESIAN_POINT('Ctrl Pts',(298.461074893041,153.429954408261,808.174384648103));
#52848=CARTESIAN_POINT('Ctrl Pts',(296.185338988511,153.429954407599,808.174384648103));
#52849=CARTESIAN_POINT('Ctrl Pts',(296.185338988511,153.429954407834,810.450120552633));
#52850=CARTESIAN_POINT('Ctrl Pts',(296.185338988511,153.429954408069,812.725856457163));
#52851=CARTESIAN_POINT('Ctrl Pts',(298.461074893041,153.429954408731,812.725856457163));
#52852=CARTESIAN_POINT('Ctrl Pts',(298.46107489266,154.738376719567,814.577620554443));
#52853=CARTESIAN_POINT('Ctrl Pts',(302.588574894606,154.738376720767,814.577620554443));
#52854=CARTESIAN_POINT('Ctrl Pts',(302.588574894605,154.738376720341,810.450120552497));
#52855=CARTESIAN_POINT('Ctrl Pts',(302.588574894605,154.738376719914,806.322620550552));
#52856=CARTESIAN_POINT('Ctrl Pts',(298.46107489266,154.738376718714,806.322620550552));
#52857=CARTESIAN_POINT('Ctrl Pts',(294.333574890715,154.738376717513,806.322620550552));
#52858=CARTESIAN_POINT('Ctrl Pts',(294.333574890715,154.73837671794,810.450120552497));
#52859=CARTESIAN_POINT('Ctrl Pts',(294.333574890715,154.738376718366,814.577620554443));
#52860=CARTESIAN_POINT('Ctrl Pts',(298.46107489266,154.738376719567,814.577620554443));
#52861=CARTESIAN_POINT('Origin',(298.461074890965,160.568052534774,810.458479291925));
#52862=CARTESIAN_POINT('Origin',(298.461074890952,247.282959303211,836.688320551891));
#52863=CARTESIAN_POINT('',(389.393074890952,247.282959303217,836.688320551891));
#52864=CARTESIAN_POINT('',(298.461074890946,338.214959303211,836.68832055189));
#52865=CARTESIAN_POINT('Origin',(298.461074890952,247.282959303211,836.688320551891));
#52866=CARTESIAN_POINT('Origin',(298.461074890952,247.282959303211,836.688320551891));
#52867=CARTESIAN_POINT('',(298.461074890947,319.164959303212,855.73832055189));
#52868=CARTESIAN_POINT('Origin',(298.461074890947,319.164959303212,836.68832055189));
#52869=CARTESIAN_POINT('Origin',(298.461074890952,247.282959303211,855.738320551891));
#52870=CARTESIAN_POINT('Origin',(298.461074890952,247.282959303211,814.463320551891));
#52871=CARTESIAN_POINT('',(389.393074890952,247.282959303217,814.463320551891));
#52872=CARTESIAN_POINT('Origin',(298.461074890948,319.190359303212,855.73832055189));
#52873=CARTESIAN_POINT('Origin',(298.461074890952,234.811559303209,601.738320551891));
#52874=CARTESIAN_POINT('',(310.907074890952,247.28295930321,601.738320551891));
#52875=CARTESIAN_POINT('Origin',(298.461074890952,247.282959303209,601.738320551891));
#52876=CARTESIAN_POINT('Origin',(298.461074890952,247.28295930321,696.988320551891));
#52877=CARTESIAN_POINT('',(215.530074890952,247.282959303204,601.738320551891));
#52878=CARTESIAN_POINT('',(215.530074890952,247.282959303205,696.988320551891));
#52879=CARTESIAN_POINT('',(230.969667895203,199.091043562764,601.738320551892));
#52880=CARTESIAN_POINT('Origin',(298.461074890952,247.282959303209,601.738320551891));
#52881=CARTESIAN_POINT('Origin',(298.461074890952,247.282959303209,601.738320551891));
#52882=CARTESIAN_POINT('Origin',(328.699774890951,246.571759303211,559.345720551891));
#52883=CARTESIAN_POINT('',(329.398274890951,246.571759303211,557.521862913425));
#52884=CARTESIAN_POINT('',(328.001274890951,246.571759303211,558.102555467932));
#52885=CARTESIAN_POINT('Origin',(330.846074890951,246.571759303211,562.97566630189));
#52886=CARTESIAN_POINT('',(328.001274890951,246.571759303211,559.320320551891));
#52887=CARTESIAN_POINT('',(328.001274890951,246.571759303211,559.320320551891));
#52888=CARTESIAN_POINT('',(329.398274890951,246.571759303211,559.320320551891));
#52889=CARTESIAN_POINT('',(329.398274890951,246.571759303211,559.320320551891));
#52890=CARTESIAN_POINT('',(329.398274890951,246.571759303211,559.320320551891));
#52891=CARTESIAN_POINT('Origin',(330.846074890951,250.153159303211,559.320320551891));
#52892=CARTESIAN_POINT('',(328.001274890951,247.994159303211,559.320320551891));
#52893=CARTESIAN_POINT('',(328.001274890951,246.571759303211,559.320320551891));
#52894=CARTESIAN_POINT('',(329.398274890951,247.994159303211,559.320320551891));
#52895=CARTESIAN_POINT('',(328.001274890951,247.994159303211,559.320320551891));
#52896=CARTESIAN_POINT('',(330.134874890951,248.730759303211,559.320320551891));
#52897=CARTESIAN_POINT('',(329.398274890951,247.994159303211,559.320320551891));
#52898=CARTESIAN_POINT('',(330.134874890951,250.127759303211,559.320320551891));
#52899=CARTESIAN_POINT('',(330.134874890951,248.730759303211,559.320320551891));
#52900=CARTESIAN_POINT('',(331.557274890951,250.127759303211,559.320320551891));
#52901=CARTESIAN_POINT('',(330.134874890951,250.127759303211,559.320320551891));
#52902=CARTESIAN_POINT('',(331.557274890951,248.730759303211,559.320320551891));
#52903=CARTESIAN_POINT('',(331.557274890951,250.127759303211,559.320320551891));
#52904=CARTESIAN_POINT('',(332.293874890951,247.994159303211,559.320320551891));
#52905=CARTESIAN_POINT('',(331.557274890951,248.730759303211,559.320320551891));
#52906=CARTESIAN_POINT('',(333.690874890951,247.994159303211,559.320320551891));
#52907=CARTESIAN_POINT('',(332.293874890951,247.994159303211,559.320320551891));
#52908=CARTESIAN_POINT('',(333.690874890951,246.571759303211,559.320320551891));
#52909=CARTESIAN_POINT('',(333.690874890951,247.994159303211,559.320320551891));
#52910=CARTESIAN_POINT('',(332.293874890951,246.571759303211,559.320320551891));
#52911=CARTESIAN_POINT('',(333.690874890951,246.571759303211,559.320320551891));
#52912=CARTESIAN_POINT('',(331.557274890951,245.835159303211,559.320320551891));
#52913=CARTESIAN_POINT('',(332.293874890951,246.571759303211,559.320320551891));
#52914=CARTESIAN_POINT('',(331.557274890952,244.438159303211,559.320320551891));
#52915=CARTESIAN_POINT('',(331.557274890951,245.835159303211,559.320320551891));
#52916=CARTESIAN_POINT('',(330.134874890952,244.438159303211,559.320320551891));
#52917=CARTESIAN_POINT('',(331.557274890952,244.438159303211,559.320320551891));
#52918=CARTESIAN_POINT('',(330.134874890951,245.835159303211,559.320320551891));
#52919=CARTESIAN_POINT('',(330.134874890952,244.438159303211,559.320320551891));
#52920=CARTESIAN_POINT('',(330.134874890951,245.835159303211,559.320320551891));
#52921=CARTESIAN_POINT('Origin',(329.766574890951,246.203459303211,559.345720551891));
#52922=CARTESIAN_POINT('',(330.134874890951,245.835159303211,557.521862913425));
#52923=CARTESIAN_POINT('Origin',(329.766574890951,246.20345930321,562.975666301901));
#52924=CARTESIAN_POINT('',(330.134874890951,245.835159303211,559.320320551891));
#52925=CARTESIAN_POINT('Origin',(263.586874890952,244.514359303207,576.363720551891));
#52926=CARTESIAN_POINT('',(266.050674890952,244.514359303207,560.082320551891));
#52927=CARTESIAN_POINT('',(266.050674890952,244.514359303207,576.338320551891));
#52928=CARTESIAN_POINT('',(266.050674890952,244.514359303207,560.082320551891));
#52929=CARTESIAN_POINT('',(262.232252516023,244.514359303207,560.082320551891));
#52930=CARTESIAN_POINT('',(266.050674890952,244.514359303207,560.082320551891));
#52931=CARTESIAN_POINT('',(262.232252516023,244.514359303207,559.828320551891));
#52932=CARTESIAN_POINT('',(262.232252516023,244.514359303207,560.082320551891));
#52933=CARTESIAN_POINT('',(261.123074890952,244.514359303206,559.828320551891));
#52934=CARTESIAN_POINT('',(261.123074890952,244.514359303206,559.828320551891));
#52935=CARTESIAN_POINT('',(261.123074890952,244.514359303207,576.338320551891));
#52936=CARTESIAN_POINT('',(261.123074890952,244.514359303206,559.828320551891));
#52937=CARTESIAN_POINT('',(266.050674890952,244.514359303207,576.338320551891));
#52938=CARTESIAN_POINT('Origin',(263.586874890951,250.051559303207,576.363720551891));
#52939=CARTESIAN_POINT('',(262.232252516023,250.051559303207,559.828320551891));
#52940=CARTESIAN_POINT('',(262.232252516023,250.051559303207,560.082320551891));
#52941=CARTESIAN_POINT('',(262.232252516023,250.051559303207,559.828320551891));
#52942=CARTESIAN_POINT('',(266.050674890951,250.051559303207,560.082320551891));
#52943=CARTESIAN_POINT('',(262.232252516023,250.051559303207,560.082320551891));
#52944=CARTESIAN_POINT('',(266.050674890951,250.051559303207,576.338320551891));
#52945=CARTESIAN_POINT('',(266.050674890951,250.051559303207,560.082320551891));
#52946=CARTESIAN_POINT('',(261.123074890951,250.051559303207,576.338320551891));
#52947=CARTESIAN_POINT('',(261.123074890951,250.051559303207,576.338320551891));
#52948=CARTESIAN_POINT('',(261.123074890951,250.051559303206,559.828320551891));
#52949=CARTESIAN_POINT('',(261.123074890951,250.051559303206,559.828320551891));
#52950=CARTESIAN_POINT('',(262.232252516023,250.051559303207,559.828320551891));
#52951=CARTESIAN_POINT('Origin',(333.335274890951,252.388359303211,559.828320551891));
#52952=CARTESIAN_POINT('',(335.799074890951,242.202959303211,559.828320551891));
#52953=CARTESIAN_POINT('',(330.871474890952,242.202959303211,559.828320551891));
#52954=CARTESIAN_POINT('',(335.799074890951,242.202959303211,559.828320551891));
#52955=CARTESIAN_POINT('',(330.871474890951,252.362959303211,559.828320551891));
#52956=CARTESIAN_POINT('Origin',(330.871474890952,247.282959303211,559.828320551891));
#52957=CARTESIAN_POINT('',(335.799074890951,252.362959303212,559.828320551891));
#52958=CARTESIAN_POINT('',(330.871474890951,252.362959303211,559.828320551891));
#52959=CARTESIAN_POINT('Origin',(335.799074890951,247.282959303211,559.828320551891));
#52960=CARTESIAN_POINT('',(334.68989726588,244.514359303211,559.828320551891));
#52961=CARTESIAN_POINT('',(334.689897265879,250.051559303212,559.828320551891));
#52962=CARTESIAN_POINT('Origin',(330.846074890951,247.282959303211,559.828320551891));
#52963=CARTESIAN_POINT('',(335.799074890951,244.514359303211,559.828320551891));
#52964=CARTESIAN_POINT('',(334.68989726588,244.514359303211,559.828320551891));
#52965=CARTESIAN_POINT('',(335.799074890951,250.051559303212,559.828320551891));
#52966=CARTESIAN_POINT('Origin',(335.799074890951,247.282959303211,559.828320551891));
#52967=CARTESIAN_POINT('',(335.799074890951,250.051559303212,559.828320551891));
#52968=CARTESIAN_POINT('Origin',(335.799074890951,247.282959303211,560.082320551891));
#52969=CARTESIAN_POINT('',(335.799074890951,242.202959303211,560.336320551891));
#52970=CARTESIAN_POINT('',(335.799074890951,252.362959303212,560.336320551891));
#52971=CARTESIAN_POINT('Origin',(335.799074890951,247.282959303211,560.336320551891));
#52972=CARTESIAN_POINT('',(335.799074890951,242.202959303211,559.828320551891));
#52973=CARTESIAN_POINT('',(335.799074890951,252.362959303212,559.828320551891));
#52974=CARTESIAN_POINT('Origin',(333.335274890951,252.362959303211,560.361720551891));
#52975=CARTESIAN_POINT('',(330.871474890951,252.362959303211,560.336320551891));
#52976=CARTESIAN_POINT('',(335.799074890951,252.362959303212,560.336320551891));
#52977=CARTESIAN_POINT('',(330.871474890951,252.362959303211,559.828320551891));
#52978=CARTESIAN_POINT('Origin',(330.871474890952,247.282959303211,560.082320551891));
#52979=CARTESIAN_POINT('',(330.871474890952,242.202959303211,560.336320551891));
#52980=CARTESIAN_POINT('Origin',(330.871474890952,247.282959303211,560.336320551891));
#52981=CARTESIAN_POINT('',(330.871474890952,242.202959303211,559.828320551891));
#52982=CARTESIAN_POINT('Origin',(333.335274890952,242.202959303211,560.361720551891));
#52983=CARTESIAN_POINT('',(330.871474890952,242.202959303211,560.336320551891));
#52984=CARTESIAN_POINT('Origin',(263.586874890951,252.388359303207,559.828320551891));
#52985=CARTESIAN_POINT('',(266.050674890952,242.202959303207,559.828320551891));
#52986=CARTESIAN_POINT('',(261.123074890952,242.202959303206,559.828320551891));
#52987=CARTESIAN_POINT('',(266.050674890952,242.202959303207,559.828320551891));
#52988=CARTESIAN_POINT('',(261.123074890951,252.362959303206,559.828320551891));
#52989=CARTESIAN_POINT('Origin',(261.123074890951,247.282959303206,559.828320551891));
#52990=CARTESIAN_POINT('',(266.050674890951,252.362959303207,559.828320551891));
#52991=CARTESIAN_POINT('',(261.123074890951,252.362959303206,559.828320551891));
#52992=CARTESIAN_POINT('Origin',(266.050674890951,247.282959303207,559.828320551891));
#52993=CARTESIAN_POINT('Origin',(266.076074890951,247.282959303207,559.828320551891));
#52994=CARTESIAN_POINT('Origin',(261.123074890951,247.282959303206,559.828320551891));
#52995=CARTESIAN_POINT('Origin',(266.050674890951,247.282959303207,560.082320551891));
#52996=CARTESIAN_POINT('',(266.050674890952,242.202959303207,560.336320551891));
#52997=CARTESIAN_POINT('',(266.050674890951,252.362959303207,560.336320551891));
#52998=CARTESIAN_POINT('Origin',(266.050674890951,247.282959303207,560.336320551891));
#52999=CARTESIAN_POINT('',(266.050674890952,242.202959303207,559.828320551891));
#53000=CARTESIAN_POINT('',(266.050674890951,252.362959303207,559.828320551891));
#53001=CARTESIAN_POINT('Origin',(263.586874890951,252.362959303207,560.361720551891));
#53002=CARTESIAN_POINT('',(261.123074890951,252.362959303206,560.336320551891));
#53003=CARTESIAN_POINT('',(266.050674890951,252.362959303207,560.336320551891));
#53004=CARTESIAN_POINT('',(261.123074890951,252.362959303206,559.828320551891));
#53005=CARTESIAN_POINT('Origin',(261.123074890951,247.282959303206,560.082320551891));
#53006=CARTESIAN_POINT('',(261.123074890952,242.202959303206,560.336320551891));
#53007=CARTESIAN_POINT('Origin',(261.123074890951,247.282959303206,560.336320551891));
#53008=CARTESIAN_POINT('',(261.123074890952,242.202959303206,559.828320551891));
#53009=CARTESIAN_POINT('Origin',(263.586874890952,242.202959303207,560.361720551891));
#53010=CARTESIAN_POINT('',(261.123074890952,242.202959303206,560.336320551891));
#53011=CARTESIAN_POINT('Origin',(245.702070179666,303.970074014487,585.736320551891));
#53012=CARTESIAN_POINT('',(241.799360179667,300.041964014487,585.736320551891));
#53013=CARTESIAN_POINT('Origin',(245.702070179667,300.041964014487,585.736320551891));
#53014=CARTESIAN_POINT('Origin',(245.702070179667,300.041964014487,573.466215551891));
#53015=CARTESIAN_POINT('',(241.799360179667,300.041964014486,561.196110551891));
#53016=CARTESIAN_POINT('',(241.799360179667,300.041964014486,573.466215551891));
#53017=CARTESIAN_POINT('',(248.878197188823,297.774065743884,561.196110551891));
#53018=CARTESIAN_POINT('Origin',(245.702070179667,300.041964014487,561.196110551891));
#53019=CARTESIAN_POINT('Origin',(245.702070179667,300.041964014487,561.196110551891));
#53020=CARTESIAN_POINT('Origin',(245.702070179667,300.041964014486,561.110131551891));
#53021=CARTESIAN_POINT('',(249.57791667636,297.274434396927,560.336320551891));
#53022=CARTESIAN_POINT('',(248.948169137577,297.724102609188,561.110131551891));
#53023=CARTESIAN_POINT('Origin',(245.702070179667,300.041964014487,560.336320551891));
#53024=CARTESIAN_POINT('Origin',(351.220079602236,198.452064591931,585.736320551891));
#53025=CARTESIAN_POINT('',(347.317369602236,194.523954591931,585.736320551891));
#53026=CARTESIAN_POINT('Origin',(351.220079602236,194.523954591931,585.736320551891));
#53027=CARTESIAN_POINT('Origin',(351.220079602236,194.523954591931,573.466215551891));
#53028=CARTESIAN_POINT('',(347.317369602236,194.523954591931,561.196110551891));
#53029=CARTESIAN_POINT('',(347.317369602236,194.523954591931,573.466215551891));
#53030=CARTESIAN_POINT('',(354.396206611393,192.256056321328,561.196110551891));
#53031=CARTESIAN_POINT('Origin',(351.220079602236,194.523954591931,561.196110551891));
#53032=CARTESIAN_POINT('Origin',(351.220079602236,194.523954591931,561.196110551891));
#53033=CARTESIAN_POINT('Origin',(351.220079602236,194.523954591931,561.110131551891));
#53034=CARTESIAN_POINT('',(355.09592609893,191.756424974372,560.336320551891));
#53035=CARTESIAN_POINT('',(354.466178560147,192.206093186633,561.110131551891));
#53036=CARTESIAN_POINT('Origin',(351.220079602236,194.523954591931,560.336320551891));
#53037=CARTESIAN_POINT('Origin',(351.220079602229,303.970074014494,585.73632055189));
#53038=CARTESIAN_POINT('',(347.317369602229,300.041964014494,585.73632055189));
#53039=CARTESIAN_POINT('Origin',(351.220079602229,300.041964014494,585.73632055189));
#53040=CARTESIAN_POINT('Origin',(351.220079602229,300.041964014494,573.46621555189));
#53041=CARTESIAN_POINT('',(347.317369602229,300.041964014493,561.19611055189));
#53042=CARTESIAN_POINT('',(347.317369602229,300.041964014494,573.46621555189));
#53043=CARTESIAN_POINT('',(354.396206611386,297.774065743891,561.19611055189));
#53044=CARTESIAN_POINT('Origin',(351.220079602229,300.041964014494,561.19611055189));
#53045=CARTESIAN_POINT('Origin',(351.220079602229,300.041964014494,561.19611055189));
#53046=CARTESIAN_POINT('Origin',(351.220079602229,300.041964014494,561.11013155189));
#53047=CARTESIAN_POINT('',(355.095926098923,297.274434396934,560.33632055189));
#53048=CARTESIAN_POINT('',(354.46617856014,297.724102609195,561.11013155189));
#53049=CARTESIAN_POINT('Origin',(351.220079602229,300.041964014494,560.33632055189));
#53050=CARTESIAN_POINT('Origin',(245.702070179674,198.452064591924,585.736320551892));
#53051=CARTESIAN_POINT('',(241.799360179674,194.523954591924,585.736320551892));
#53052=CARTESIAN_POINT('Origin',(245.702070179674,194.523954591924,585.736320551892));
#53053=CARTESIAN_POINT('Origin',(245.702070179674,194.523954591924,573.466215551892));
#53054=CARTESIAN_POINT('',(241.799360179674,194.523954591924,561.196110551892));
#53055=CARTESIAN_POINT('',(241.799360179674,194.523954591924,573.466215551892));
#53056=CARTESIAN_POINT('',(248.878197188831,192.256056321321,561.196110551892));
#53057=CARTESIAN_POINT('Origin',(245.702070179674,194.523954591924,561.196110551892));
#53058=CARTESIAN_POINT('Origin',(245.702070179674,194.523954591924,561.196110551892));
#53059=CARTESIAN_POINT('Origin',(245.702070179674,194.523954591924,561.110131551892));
#53060=CARTESIAN_POINT('',(249.577916676367,191.756424974365,560.336320551892));
#53061=CARTESIAN_POINT('',(248.948169137584,192.206093186626,561.110131551892));
#53062=CARTESIAN_POINT('Origin',(245.702070179674,194.523954591924,560.336320551892));
#53063=CARTESIAN_POINT('Origin',(298.461074890952,247.28295930321,597.598120551891));
#53064=CARTESIAN_POINT('',(231.557799298777,199.510995973107,560.336320551892));
#53065=CARTESIAN_POINT('',(231.028481035561,199.133038803798,597.598120551892));
#53066=CARTESIAN_POINT('Origin',(298.461074890951,247.282959303209,560.336320551891));
#53067=CARTESIAN_POINT('Origin',(298.461074890946,329.516684705051,560.33632055189));
#53068=CARTESIAN_POINT('',(307.224074890956,175.45175930321,560.336320551892));
#53069=CARTESIAN_POINT('Origin',(298.461074890956,175.451759303209,560.336320551892));
#53070=CARTESIAN_POINT('',(217.866874890951,247.282959303203,560.336320551891));
#53071=CARTESIAN_POINT('Origin',(226.629874890951,247.282959303204,560.336320551891));
#53072=CARTESIAN_POINT('',(379.055274890951,247.282959303214,560.336320551891));
#53073=CARTESIAN_POINT('Origin',(370.292274890951,247.282959303214,560.336320551891));
#53074=CARTESIAN_POINT('',(289.698074890947,319.114159303208,560.33632055189));
#53075=CARTESIAN_POINT('Origin',(298.461074890947,319.114159303209,560.33632055189));
#53076=CARTESIAN_POINT('',(355.611074890951,247.282959303213,560.336320551891));
#53077=CARTESIAN_POINT('Origin',(298.461074890951,247.282959303209,560.336320551891));
#53078=CARTESIAN_POINT('Origin',(298.461074890951,247.282959303209,558.812320551891));
#53079=CARTESIAN_POINT('',(355.611074890951,247.282959303213,557.288320551891));
#53080=CARTESIAN_POINT('',(355.611074890951,247.282959303213,558.812320551891));
#53081=CARTESIAN_POINT('Origin',(298.461074890951,247.282959303209,557.288320551891));
#53082=CARTESIAN_POINT('Origin',(298.461074890948,304.458359303209,557.288320551891));
#53083=CARTESIAN_POINT('',(350.912074890951,247.282959303212,557.288320551891));
#53084=CARTESIAN_POINT('Origin',(298.461074890951,247.282959303209,557.288320551891));
#53085=CARTESIAN_POINT('Origin',(298.461074890951,247.282959303209,558.812320551891));
#53086=CARTESIAN_POINT('',(350.912074890951,247.282959303212,560.336320551891));
#53087=CARTESIAN_POINT('',(350.912074890951,247.282959303212,558.812320551891));
#53088=CARTESIAN_POINT('Origin',(298.461074890951,247.282959303209,560.336320551891));
#53089=CARTESIAN_POINT('Origin',(298.461074890948,299.759359303209,560.336320551891));
#53090=CARTESIAN_POINT('',(311.542074890951,247.28295930321,560.336320551891));
#53091=CARTESIAN_POINT('Origin',(298.461074890951,247.282959303209,560.336320551891));
#53092=CARTESIAN_POINT('Origin',(298.461074890951,247.282959303209,558.812320551891));
#53093=CARTESIAN_POINT('',(311.542074890951,247.28295930321,557.288320551891));
#53094=CARTESIAN_POINT('',(311.542074890951,247.28295930321,558.812320551891));
#53095=CARTESIAN_POINT('Origin',(298.461074890951,247.282959303209,557.288320551891));
#53096=CARTESIAN_POINT('Origin',(298.46107489095,260.389359303209,557.288320551891));
#53097=CARTESIAN_POINT('',(310.907074890951,247.28295930321,557.288320551891));
#53098=CARTESIAN_POINT('Origin',(298.461074890951,247.282959303209,557.288320551891));
#53099=CARTESIAN_POINT('Origin',(298.461074890951,247.282959303209,579.513320551891));
#53100=CARTESIAN_POINT('',(310.907074890951,247.28295930321,579.513320551891));
#53101=CARTESIAN_POINT('Origin',(298.461074890956,184.240159303209,567.956320551892));
#53102=CARTESIAN_POINT('',(307.224074890956,175.45175930321,567.956320551892));
#53103=CARTESIAN_POINT('Origin',(298.461074890956,175.451759303209,567.956320551892));
#53104=CARTESIAN_POINT('',(301.255074890956,175.451759303209,567.956320551892));
#53105=CARTESIAN_POINT('Origin',(298.461074890956,175.451759303209,567.956320551892));
#53106=CARTESIAN_POINT('Origin',(298.461074890956,175.451759303209,564.146320551892));
#53107=CARTESIAN_POINT('',(307.224074890956,175.45175930321,564.146320551892));
#53108=CARTESIAN_POINT('Origin',(298.461074890956,175.451759303209,571.766320551892));
#53109=CARTESIAN_POINT('',(301.255074890956,175.451759303209,575.576320551892));
#53110=CARTESIAN_POINT('',(301.255074890956,175.451759303209,571.766320551892));
#53111=CARTESIAN_POINT('Origin',(298.461074890956,175.451759303209,575.576320551892));
#53112=CARTESIAN_POINT('Origin',(298.461074890956,178.271159303209,575.576320551892));
#53113=CARTESIAN_POINT('Origin',(298.461074890947,319.114159303209,564.14632055189));
#53114=CARTESIAN_POINT('',(289.698074890947,319.114159303208,567.95632055189));
#53115=CARTESIAN_POINT('Origin',(298.461074890947,319.114159303209,567.95632055189));
#53116=CARTESIAN_POINT('',(289.698074890947,319.114159303208,564.14632055189));
#53117=CARTESIAN_POINT('Origin',(298.461074890946,327.902559303209,567.95632055189));
#53118=CARTESIAN_POINT('',(295.667074890947,319.114159303209,567.95632055189));
#53119=CARTESIAN_POINT('Origin',(298.461074890947,319.114159303209,567.95632055189));
#53120=CARTESIAN_POINT('Origin',(298.461074890947,319.114159303209,571.76632055189));
#53121=CARTESIAN_POINT('',(295.667074890947,319.114159303209,575.57632055189));
#53122=CARTESIAN_POINT('Origin',(298.461074890947,319.114159303209,575.57632055189));
#53123=CARTESIAN_POINT('',(295.667074890947,319.114159303209,571.76632055189));
#53124=CARTESIAN_POINT('Origin',(298.461074890946,321.933559303209,575.57632055189));
#53125=CARTESIAN_POINT('Origin',(370.292274890951,250.102359303214,575.576320551891));
#53126=CARTESIAN_POINT('',(373.086274890951,247.282959303214,575.576320551891));
#53127=CARTESIAN_POINT('Origin',(370.292274890951,247.282959303214,575.576320551891));
#53128=CARTESIAN_POINT('Origin',(370.292274890951,247.282959303214,571.766320551891));
#53129=CARTESIAN_POINT('',(373.086274890951,247.282959303214,567.956320551891));
#53130=CARTESIAN_POINT('Origin',(370.292274890951,247.282959303214,567.956320551891));
#53131=CARTESIAN_POINT('',(373.086274890951,247.282959303214,571.766320551891));
#53132=CARTESIAN_POINT('Origin',(370.292274890951,256.071359303214,567.956320551891));
#53133=CARTESIAN_POINT('',(379.055274890951,247.282959303214,567.956320551891));
#53134=CARTESIAN_POINT('Origin',(370.292274890951,247.282959303214,567.956320551891));
#53135=CARTESIAN_POINT('Origin',(370.292274890951,247.282959303214,564.146320551891));
#53136=CARTESIAN_POINT('',(379.055274890951,247.282959303214,564.146320551891));
#53137=CARTESIAN_POINT('Origin',(226.629874890951,247.282959303204,564.146320551891));
#53138=CARTESIAN_POINT('',(217.866874890951,247.282959303204,567.956320551891));
#53139=CARTESIAN_POINT('Origin',(226.629874890951,247.282959303204,567.956320551891));
#53140=CARTESIAN_POINT('',(217.866874890951,247.282959303204,564.146320551891));
#53141=CARTESIAN_POINT('Origin',(226.629874890951,256.071359303204,567.956320551891));
#53142=CARTESIAN_POINT('',(223.835874890951,247.282959303204,567.956320551891));
#53143=CARTESIAN_POINT('Origin',(226.629874890951,247.282959303204,567.956320551891));
#53144=CARTESIAN_POINT('Origin',(226.629874890951,247.282959303204,571.766320551891));
#53145=CARTESIAN_POINT('',(223.835874890951,247.282959303204,575.576320551891));
#53146=CARTESIAN_POINT('Origin',(226.629874890951,247.282959303204,575.576320551891));
#53147=CARTESIAN_POINT('',(223.835874890951,247.282959303204,571.766320551891));
#53148=CARTESIAN_POINT('Origin',(226.629874890951,250.102359303204,575.576320551891));
#53149=CARTESIAN_POINT('Origin',(333.335274890952,250.051559303212,576.363720551891));
#53150=CARTESIAN_POINT('',(330.871474890952,250.051559303212,560.082320551891));
#53151=CARTESIAN_POINT('',(330.871474890952,250.051559303212,576.338320551891));
#53152=CARTESIAN_POINT('',(330.871474890952,250.051559303212,560.082320551891));
#53153=CARTESIAN_POINT('',(334.689897265879,250.051559303212,560.082320551891));
#53154=CARTESIAN_POINT('',(330.871474890952,250.051559303212,560.082320551891));
#53155=CARTESIAN_POINT('',(334.689897265879,250.051559303212,560.082320551891));
#53156=CARTESIAN_POINT('',(335.799074890951,250.051559303212,576.338320551891));
#53157=CARTESIAN_POINT('',(335.799074890951,250.051559303212,559.828320551891));
#53158=CARTESIAN_POINT('',(330.871474890952,250.051559303212,576.338320551891));
#53159=CARTESIAN_POINT('Origin',(330.871474890952,247.282959303211,568.210320551891));
#53160=CARTESIAN_POINT('',(330.871474890952,244.514359303211,560.082320551891));
#53161=CARTESIAN_POINT('',(330.871474890952,244.514359303211,576.338320551891));
#53162=CARTESIAN_POINT('',(330.871474890952,244.514359303211,560.082320551891));
#53163=CARTESIAN_POINT('Origin',(330.871474890952,247.282959303211,560.082320551891));
#53164=CARTESIAN_POINT('Origin',(330.871474890952,247.282959303211,576.338320551891));
#53165=CARTESIAN_POINT('Origin',(333.335274890952,244.514359303211,576.363720551891));
#53166=CARTESIAN_POINT('',(334.68989726588,244.514359303211,560.082320551891));
#53167=CARTESIAN_POINT('',(334.68989726588,244.514359303211,559.828320551891));
#53168=CARTESIAN_POINT('',(334.68989726588,244.514359303211,560.082320551891));
#53169=CARTESIAN_POINT('',(335.799074890951,244.514359303211,576.338320551891));
#53170=CARTESIAN_POINT('',(335.799074890951,244.514359303211,576.338320551891));
#53171=CARTESIAN_POINT('',(335.799074890951,244.514359303211,559.828320551891));
#53172=CARTESIAN_POINT('Origin',(263.586874890951,250.076959303207,576.338320551891));
#53173=CARTESIAN_POINT('Origin',(261.123074890951,247.282959303207,576.338320551891));
#53174=CARTESIAN_POINT('Origin',(266.050674890951,247.282959303207,576.338320551891));
#53175=CARTESIAN_POINT('',(268.260474890951,247.282959303207,576.338320551891));
#53176=CARTESIAN_POINT('Origin',(266.076074890951,247.282959303207,576.338320551891));
#53177=CARTESIAN_POINT('Origin',(266.050674890951,247.282959303207,568.210320551891));
#53178=CARTESIAN_POINT('Origin',(266.050674890951,247.282959303207,560.082320551891));
#53179=CARTESIAN_POINT('Origin',(261.123074890951,247.282959303206,568.083320551891));
#53180=CARTESIAN_POINT('Origin',(335.799074890951,247.282959303211,568.083320551891));
#53181=CARTESIAN_POINT('Origin',(335.799074890951,247.282959303212,576.338320551891));
#53182=CARTESIAN_POINT('Origin',(333.335274890951,250.076959303212,576.338320551891));
#53183=CARTESIAN_POINT('',(333.030474890951,247.282959303211,576.338320551891));
#53184=CARTESIAN_POINT('Origin',(330.846074890951,247.282959303211,576.338320551891));
#53185=CARTESIAN_POINT('Origin',(330.846074890952,247.282959303211,559.955320551891));
#53186=CARTESIAN_POINT('Origin',(330.846074890952,247.282959303211,559.828320551891));
#53187=CARTESIAN_POINT('Origin',(330.846074890952,247.282959303211,560.082320551891));
#53188=CARTESIAN_POINT('Origin',(330.846074890951,247.282959303211,568.210320551891));
#53189=CARTESIAN_POINT('',(333.030474890951,247.282959303211,560.082320551891));
#53190=CARTESIAN_POINT('',(333.030474890951,247.282959303211,568.210320551891));
#53191=CARTESIAN_POINT('Origin',(330.846074890951,247.282959303211,560.082320551891));
#53192=CARTESIAN_POINT('Origin',(332.39345946167,250.076959303212,560.082320551891));
#53193=CARTESIAN_POINT('Origin',(330.846074890952,247.282959303211,562.975666301891));
#53194=CARTESIAN_POINT('',(333.690874890951,247.994159303211,558.102555467932));
#53195=CARTESIAN_POINT('',(333.690874890951,246.571759303211,558.102555467932));
#53196=CARTESIAN_POINT('Origin',(333.690874890951,247.282959303212,562.975666301898));
#53197=CARTESIAN_POINT('',(332.293874890951,247.994159303211,557.521862913425));
#53198=CARTESIAN_POINT('Origin',(330.846074890952,247.994159303211,562.97566630189));
#53199=CARTESIAN_POINT('',(331.557274890951,248.730759303211,557.521862913425));
#53200=CARTESIAN_POINT('Origin',(331.92557489095,248.36245930321,562.975666301901));
#53201=CARTESIAN_POINT('',(331.557274890951,250.127759303211,558.102555467932));
#53202=CARTESIAN_POINT('Origin',(331.557274890951,247.282959303212,562.975666301888));
#53203=CARTESIAN_POINT('',(330.134874890951,250.127759303211,558.102555467932));
#53204=CARTESIAN_POINT('Origin',(330.846074890951,250.127759303211,562.97566630189));
#53205=CARTESIAN_POINT('',(330.134874890951,248.730759303211,557.521862913425));
#53206=CARTESIAN_POINT('Origin',(330.134874890951,247.282959303212,562.975666301888));
#53207=CARTESIAN_POINT('',(329.398274890951,247.994159303211,557.521862913425));
#53208=CARTESIAN_POINT('Origin',(329.766574890951,248.362459303211,562.975666301901));
#53209=CARTESIAN_POINT('',(328.001274890951,247.994159303211,558.102555467932));
#53210=CARTESIAN_POINT('Origin',(330.846074890951,247.994159303211,562.97566630189));
#53211=CARTESIAN_POINT('Origin',(328.001274890952,247.282959303211,562.975666301889));
#53212=CARTESIAN_POINT('',(330.134874890952,244.438159303211,558.102555467932));
#53213=CARTESIAN_POINT('Origin',(330.134874890951,247.282959303211,562.975666301889));
#53214=CARTESIAN_POINT('',(331.557274890952,244.438159303211,558.102555467932));
#53215=CARTESIAN_POINT('Origin',(330.846074890952,244.438159303211,562.97566630189));
#53216=CARTESIAN_POINT('',(331.557274890951,245.835159303211,557.521862913425));
#53217=CARTESIAN_POINT('Origin',(331.557274890951,247.282959303211,562.975666301889));
#53218=CARTESIAN_POINT('',(332.293874890951,246.571759303211,557.521862913425));
#53219=CARTESIAN_POINT('Origin',(331.925574890951,246.203459303212,562.975666301901));
#53220=CARTESIAN_POINT('Origin',(330.846074890952,246.571759303211,562.97566630189));
#53221=CARTESIAN_POINT('Origin',(264.528690320232,250.076959303207,560.082320551891));
#53222=CARTESIAN_POINT('Origin',(266.076074890951,247.282959303207,560.082320551891));
#53223=CARTESIAN_POINT('',(268.260474890951,247.282959303207,560.082320551891));
#53224=CARTESIAN_POINT('Origin',(266.076074890951,247.282959303207,560.082320551891));
#53225=CARTESIAN_POINT('Origin',(266.076074890951,247.282959303207,568.210320551891));
#53226=CARTESIAN_POINT('',(268.260474890952,247.282959303207,568.210320551891));
#53227=CARTESIAN_POINT('Origin',(266.076074890951,247.282959303207,559.955320551891));
#53228=CARTESIAN_POINT('Origin',(266.076074890952,247.282959303207,559.828320551891));
#53229=CARTESIAN_POINT('Origin',(266.076074890951,247.282959303207,562.975666301891));
#53230=CARTESIAN_POINT('',(268.920874890951,247.994159303207,558.102555467933));
#53231=CARTESIAN_POINT('',(268.920874890951,246.571759303207,558.102555467933));
#53232=CARTESIAN_POINT('Origin',(268.920874890953,247.282959303207,562.975666301892));
#53233=CARTESIAN_POINT('',(267.523874890951,247.994159303207,557.521862913425));
#53234=CARTESIAN_POINT('Origin',(266.076074890953,247.994159303207,562.975666301888));
#53235=CARTESIAN_POINT('',(266.787274890951,248.730759303207,557.521862913425));
#53236=CARTESIAN_POINT('Origin',(267.15557489095,248.362459303206,562.975666301897));
#53237=CARTESIAN_POINT('',(266.787274890951,250.127759303207,558.102555467933));
#53238=CARTESIAN_POINT('Origin',(266.787274890951,247.282959303209,562.975666301886));
#53239=CARTESIAN_POINT('',(265.364874890951,250.127759303207,558.102555467933));
#53240=CARTESIAN_POINT('Origin',(266.076074890951,250.127759303207,562.975666301891));
#53241=CARTESIAN_POINT('',(265.364874890951,248.730759303207,557.521862913425));
#53242=CARTESIAN_POINT('Origin',(265.364874890952,247.282959303207,562.975666301891));
#53243=CARTESIAN_POINT('',(264.628274890951,247.994159303207,557.521862913425));
#53244=CARTESIAN_POINT('Origin',(264.996574890949,248.362459303209,562.975666301889));
#53245=CARTESIAN_POINT('',(263.231274890951,247.994159303207,558.102555467933));
#53246=CARTESIAN_POINT('Origin',(266.076074890952,247.994159303207,562.975666301893));
#53247=CARTESIAN_POINT('',(263.231274890951,246.571759303207,558.102555467933));
#53248=CARTESIAN_POINT('Origin',(263.231274890951,247.282959303207,562.975666301891));
#53249=CARTESIAN_POINT('',(264.628274890951,246.571759303207,557.521862913425));
#53250=CARTESIAN_POINT('Origin',(266.076074890952,246.571759303207,562.975666301892));
#53251=CARTESIAN_POINT('',(265.364874890951,245.835159303207,557.521862913425));
#53252=CARTESIAN_POINT('Origin',(264.996574890949,246.203459303204,562.975666301889));
#53253=CARTESIAN_POINT('',(265.364874890952,244.438159303207,558.102555467933));
#53254=CARTESIAN_POINT('Origin',(265.364874890952,247.282959303207,562.975666301891));
#53255=CARTESIAN_POINT('',(266.787274890952,244.438159303207,558.102555467933));
#53256=CARTESIAN_POINT('Origin',(266.076074890952,244.438159303207,562.975666301891));
#53257=CARTESIAN_POINT('',(266.787274890951,245.835159303207,557.521862913425));
#53258=CARTESIAN_POINT('Origin',(266.787274890951,247.282959303207,562.975666301893));
#53259=CARTESIAN_POINT('',(267.523874890951,246.571759303207,557.521862913425));
#53260=CARTESIAN_POINT('Origin',(267.155574890951,246.203459303207,562.975666301901));
#53261=CARTESIAN_POINT('Origin',(266.076074890954,246.571759303207,562.975666301885));
#53262=CARTESIAN_POINT('Origin',(263.929774890951,246.571759303207,559.345720551891));
#53263=CARTESIAN_POINT('',(263.231274890951,246.571759303207,559.320320551891));
#53264=CARTESIAN_POINT('',(263.231274890951,246.571759303207,559.320320551891));
#53265=CARTESIAN_POINT('',(264.628274890951,246.571759303207,559.320320551891));
#53266=CARTESIAN_POINT('',(264.628274890951,246.571759303207,559.320320551891));
#53267=CARTESIAN_POINT('',(264.628274890951,246.571759303207,559.320320551891));
#53268=CARTESIAN_POINT('Origin',(263.231274890951,248.019559303207,558.659540417467));
#53269=CARTESIAN_POINT('',(263.231274890951,247.994159303207,559.320320551891));
#53270=CARTESIAN_POINT('',(263.231274890951,247.994159303207,559.320320551891));
#53271=CARTESIAN_POINT('',(263.231274890951,246.571759303207,559.320320551891));
#53272=CARTESIAN_POINT('Origin',(263.929774890951,247.994159303207,559.345720551891));
#53273=CARTESIAN_POINT('',(264.628274890951,247.994159303207,559.320320551891));
#53274=CARTESIAN_POINT('',(264.628274890951,247.994159303207,559.320320551891));
#53275=CARTESIAN_POINT('',(263.231274890951,247.994159303207,559.320320551891));
#53276=CARTESIAN_POINT('Origin',(264.996574890951,248.362459303207,559.345720551891));
#53277=CARTESIAN_POINT('',(265.364874890951,248.730759303207,559.320320551891));
#53278=CARTESIAN_POINT('',(265.364874890951,248.730759303207,559.320320551891));
#53279=CARTESIAN_POINT('',(264.628274890951,247.994159303207,559.320320551891));
#53280=CARTESIAN_POINT('Origin',(265.364874890951,250.153159303207,558.421091732658));
#53281=CARTESIAN_POINT('',(265.364874890951,250.127759303207,559.320320551891));
#53282=CARTESIAN_POINT('',(265.364874890951,250.127759303207,559.320320551891));
#53283=CARTESIAN_POINT('',(265.364874890951,248.730759303207,559.320320551891));
#53284=CARTESIAN_POINT('Origin',(266.076074890951,250.127759303207,559.345720551891));
#53285=CARTESIAN_POINT('',(266.787274890951,250.127759303207,559.320320551891));
#53286=CARTESIAN_POINT('',(266.787274890951,250.127759303207,559.320320551891));
#53287=CARTESIAN_POINT('',(265.364874890951,250.127759303207,559.320320551891));
#53288=CARTESIAN_POINT('Origin',(266.787274890951,250.153159303207,558.421091732658));
#53289=CARTESIAN_POINT('',(266.787274890951,248.730759303207,559.320320551891));
#53290=CARTESIAN_POINT('',(266.787274890951,248.730759303207,559.320320551891));
#53291=CARTESIAN_POINT('',(266.787274890951,250.127759303207,559.320320551891));
#53292=CARTESIAN_POINT('Origin',(267.155574890951,248.362459303207,559.345720551891));
#53293=CARTESIAN_POINT('',(267.523874890951,247.994159303207,559.320320551891));
#53294=CARTESIAN_POINT('',(267.523874890951,247.994159303207,559.320320551891));
#53295=CARTESIAN_POINT('',(266.787274890951,248.730759303207,559.320320551891));
#53296=CARTESIAN_POINT('Origin',(268.222374890951,247.994159303207,559.345720551891));
#53297=CARTESIAN_POINT('',(268.920874890951,247.994159303207,559.320320551891));
#53298=CARTESIAN_POINT('',(268.920874890951,247.994159303207,559.320320551891));
#53299=CARTESIAN_POINT('',(267.523874890951,247.994159303207,559.320320551891));
#53300=CARTESIAN_POINT('Origin',(268.920874890951,248.019559303207,558.685625936038));
#53301=CARTESIAN_POINT('',(268.920874890951,246.571759303207,559.320320551891));
#53302=CARTESIAN_POINT('',(268.920874890951,246.571759303207,559.320320551891));
#53303=CARTESIAN_POINT('',(268.920874890951,247.994159303207,559.320320551891));
#53304=CARTESIAN_POINT('Origin',(268.222374890951,246.571759303207,559.345720551891));
#53305=CARTESIAN_POINT('',(267.523874890951,246.571759303207,559.320320551891));
#53306=CARTESIAN_POINT('',(267.523874890951,246.571759303207,559.320320551891));
#53307=CARTESIAN_POINT('',(268.920874890951,246.571759303207,559.320320551891));
#53308=CARTESIAN_POINT('Origin',(267.155574890951,246.203459303207,559.345720551891));
#53309=CARTESIAN_POINT('',(266.787274890951,245.835159303207,559.320320551891));
#53310=CARTESIAN_POINT('',(266.787274890951,245.835159303207,559.320320551891));
#53311=CARTESIAN_POINT('',(267.523874890951,246.571759303207,559.320320551891));
#53312=CARTESIAN_POINT('Origin',(266.787274890951,245.860559303207,558.421091732658));
#53313=CARTESIAN_POINT('',(266.787274890952,244.438159303207,559.320320551891));
#53314=CARTESIAN_POINT('',(266.787274890952,244.438159303207,559.320320551891));
#53315=CARTESIAN_POINT('',(266.787274890951,245.835159303207,559.320320551891));
#53316=CARTESIAN_POINT('Origin',(266.076074890952,244.438159303207,559.345720551891));
#53317=CARTESIAN_POINT('',(265.364874890952,244.438159303207,559.320320551891));
#53318=CARTESIAN_POINT('',(265.364874890952,244.438159303207,559.320320551891));
#53319=CARTESIAN_POINT('',(266.787274890952,244.438159303207,559.320320551891));
#53320=CARTESIAN_POINT('Origin',(265.364874890951,245.860559303207,558.421091732658));
#53321=CARTESIAN_POINT('',(265.364874890951,245.835159303207,559.320320551891));
#53322=CARTESIAN_POINT('',(265.364874890951,245.835159303207,559.320320551891));
#53323=CARTESIAN_POINT('',(265.364874890952,244.438159303207,559.320320551891));
#53324=CARTESIAN_POINT('Origin',(264.996574890951,246.203459303207,559.345720551891));
#53325=CARTESIAN_POINT('',(265.364874890951,245.835159303207,559.320320551891));
#53326=CARTESIAN_POINT('Origin',(266.076074890951,250.153159303207,559.320320551891));
#53327=CARTESIAN_POINT('Origin',(328.001274890951,247.282959303211,559.345720551891));
#53328=CARTESIAN_POINT('',(328.001274890951,247.994159303211,559.320320551891));
#53329=CARTESIAN_POINT('Origin',(328.699774890951,247.994159303211,559.345720551891));
#53330=CARTESIAN_POINT('',(329.398274890951,247.994159303211,559.320320551891));
#53331=CARTESIAN_POINT('Origin',(329.766574890951,248.362459303211,559.345720551891));
#53332=CARTESIAN_POINT('',(330.134874890951,248.730759303211,559.320320551891));
#53333=CARTESIAN_POINT('Origin',(330.134874890951,250.153159303211,558.421091732658));
#53334=CARTESIAN_POINT('',(330.134874890951,250.127759303211,559.320320551891));
#53335=CARTESIAN_POINT('Origin',(330.846074890951,250.127759303211,559.345720551891));
#53336=CARTESIAN_POINT('',(331.557274890951,250.127759303211,559.320320551891));
#53337=CARTESIAN_POINT('Origin',(331.557274890951,250.153159303211,558.421091732658));
#53338=CARTESIAN_POINT('',(331.557274890951,248.730759303211,559.320320551891));
#53339=CARTESIAN_POINT('Origin',(331.925574890951,248.362459303211,559.345720551891));
#53340=CARTESIAN_POINT('',(332.293874890951,247.994159303211,559.320320551891));
#53341=CARTESIAN_POINT('Origin',(332.992374890951,247.994159303211,559.345720551891));
#53342=CARTESIAN_POINT('',(333.690874890951,247.994159303211,559.320320551891));
#53343=CARTESIAN_POINT('Origin',(333.690874890951,248.019559303211,558.685625936038));
#53344=CARTESIAN_POINT('',(333.690874890951,246.571759303211,559.320320551891));
#53345=CARTESIAN_POINT('Origin',(332.992374890951,246.571759303211,559.345720551891));
#53346=CARTESIAN_POINT('',(332.293874890951,246.571759303211,559.320320551891));
#53347=CARTESIAN_POINT('Origin',(331.925574890952,246.203459303211,559.345720551891));
#53348=CARTESIAN_POINT('',(331.557274890951,245.835159303211,559.320320551891));
#53349=CARTESIAN_POINT('Origin',(331.557274890951,245.860559303211,558.421091732658));
#53350=CARTESIAN_POINT('',(331.557274890952,244.438159303211,559.320320551891));
#53351=CARTESIAN_POINT('Origin',(330.846074890952,244.438159303211,559.345720551891));
#53352=CARTESIAN_POINT('',(330.134874890952,244.438159303211,559.320320551891));
#53353=CARTESIAN_POINT('Origin',(330.134874890951,245.860559303211,558.421091732658));
#53354=CARTESIAN_POINT('',(0.,0.,0.));
#53355=CARTESIAN_POINT('Origin',(144.115917770964,-309.972007268788,340.708039952219));
#53356=CARTESIAN_POINT('',(184.115917770964,-310.472007268788,340.708039952219));
#53357=CARTESIAN_POINT('',(184.115917770964,-309.972007268788,340.208039952218));
#53358=CARTESIAN_POINT('Origin',(184.115917770964,-309.972007268788,340.708039952219));
#53359=CARTESIAN_POINT('',(454.11591777097,-309.972007268788,340.208039952218));
#53360=CARTESIAN_POINT('',(144.115917770964,-309.972007268788,340.208039952219));
#53361=CARTESIAN_POINT('',(454.11591777097,-310.472007268788,340.708039952218));
#53362=CARTESIAN_POINT('Origin',(454.11591777097,-309.972007268788,340.708039952218));
#53363=CARTESIAN_POINT('',(144.115917770964,-310.472007268788,340.708039952219));
#53364=CARTESIAN_POINT('Origin',(144.115917770964,-310.472007268788,340.208039952219));
#53365=CARTESIAN_POINT('',(184.115917770964,-270.472007268788,340.208039952219));
#53366=CARTESIAN_POINT('',(184.115917770964,-290.472007268788,340.208039952219));
#53367=CARTESIAN_POINT('',(144.615917770964,-270.472007268788,340.208039952219));
#53368=CARTESIAN_POINT('',(144.115917770964,-270.472007268788,340.208039952219));
#53369=CARTESIAN_POINT('',(144.615917770964,-10.7242208197787,340.208039952219));
#53370=CARTESIAN_POINT('',(144.615917770964,-150.084339619182,340.208039952219));
#53371=CARTESIAN_POINT('',(184.115917770964,-10.7242208197787,340.208039952219));
#53372=CARTESIAN_POINT('',(164.115917770964,-10.7242208197787,340.208039952219));
#53373=CARTESIAN_POINT('',(184.115917770964,29.1607759831004,340.208039952219));
#53374=CARTESIAN_POINT('',(184.115917770964,-140.598114044284,340.208039952219));
#53375=CARTESIAN_POINT('',(454.11591777097,29.1607759831002,340.208039952218));
#53376=CARTESIAN_POINT('',(144.115917770964,29.1607759831004,340.208039952219));
#53377=CARTESIAN_POINT('',(454.11591777097,-10.7242208197788,340.208039952218));
#53378=CARTESIAN_POINT('',(454.11591777097,-160.598114044284,340.208039952218));
#53379=CARTESIAN_POINT('',(493.61591777097,-10.7242208197789,340.208039952218));
#53380=CARTESIAN_POINT('',(319.115917770967,-10.7242208197788,340.208039952218));
#53381=CARTESIAN_POINT('',(493.61591777097,-270.472007268782,340.208039952218));
#53382=CARTESIAN_POINT('',(493.61591777097,-150.222007268789,340.208039952218));
#53383=CARTESIAN_POINT('',(454.11591777097,-270.472007268782,340.208039952218));
#53384=CARTESIAN_POINT('',(299.115917770967,-270.472007268782,340.208039952218));
#53385=CARTESIAN_POINT('',(454.11591777097,-310.472007268785,340.208039952218));
#53386=CARTESIAN_POINT('',(444.115917770964,-64.2840072687828,340.208039952218));
#53387=CARTESIAN_POINT('Origin',(444.115917770964,-70.4720072687828,340.208039952218));
#53388=CARTESIAN_POINT('',(194.115917770964,-284.284007268782,340.208039952219));
#53389=CARTESIAN_POINT('Origin',(194.115917770964,-290.472007268782,340.208039952219));
#53390=CARTESIAN_POINT('',(444.115917770964,-100.472007268783,340.208039952218));
#53391=CARTESIAN_POINT('',(194.115917770964,-100.472007268783,340.208039952219));
#53392=CARTESIAN_POINT('',(169.115917770964,-100.472007268783,340.208039952219));
#53393=CARTESIAN_POINT('',(194.115917770964,-260.472007268782,340.208039952219));
#53394=CARTESIAN_POINT('',(194.115917770964,-285.472007268785,340.208039952219));
#53395=CARTESIAN_POINT('',(444.115917770964,-260.472007268782,340.208039952218));
#53396=CARTESIAN_POINT('',(294.115917770964,-260.472007268782,340.208039952218));
#53397=CARTESIAN_POINT('',(444.115917770964,-205.472007268785,340.208039952218));
#53398=CARTESIAN_POINT('',(194.115917770964,-64.2840072687827,340.208039952219));
#53399=CARTESIAN_POINT('Origin',(194.115917770964,-70.4720072687827,340.208039952219));
#53400=CARTESIAN_POINT('',(444.115917770964,-284.284007268782,340.208039952218));
#53401=CARTESIAN_POINT('Origin',(444.115917770964,-290.472007268782,340.208039952218));
#53402=CARTESIAN_POINT('Origin',(493.61591777097,-150.222007268789,340.708039952218));
#53403=CARTESIAN_POINT('',(494.11591777097,-10.7242208197795,340.708039952218));
#53404=CARTESIAN_POINT('Origin',(493.61591777097,-10.7242208197795,340.708039952218));
#53405=CARTESIAN_POINT('',(494.11591777097,-270.472007268782,340.708039952217));
#53406=CARTESIAN_POINT('',(494.11591777097,-150.222007268789,340.708039952218));
#53407=CARTESIAN_POINT('Origin',(493.61591777097,-270.472007268782,340.708039952217));
#53408=CARTESIAN_POINT('Origin',(494.11591777097,10.0279927312103,335.389856654884));
#53409=CARTESIAN_POINT('',(494.11591777097,-270.472007268782,320.779712758553));
#53410=CARTESIAN_POINT('',(494.11591777097,-270.472007268782,340.208039952218));
#53411=CARTESIAN_POINT('',(494.11591777097,-10.7242208197793,320.779712758176));
#53412=CARTESIAN_POINT('',(494.11591777097,-10.7242208197789,340.208039952218));
#53413=CARTESIAN_POINT('',(494.11591777097,29.2757791802208,320.779712758118));
#53414=CARTESIAN_POINT('',(494.11591777097,-55.6611674320453,320.779712758241));
#53415=CARTESIAN_POINT('',(494.11591777097,29.2757791802205,340.763897945769));
#53416=CARTESIAN_POINT('',(494.11591777097,29.2757791802212,340.208039952218));
#53417=CARTESIAN_POINT('',(494.11591777097,69.3907823772571,321.27971275806));
#53418=CARTESIAN_POINT('',(494.11591777097,22.6541183795134,343.980092760897));
#53419=CARTESIAN_POINT('',(494.11591777097,330.027992731203,321.279712757682));
#53420=CARTESIAN_POINT('',(494.11591777097,39.6518859556631,321.279712758103));
#53421=CARTESIAN_POINT('',(494.11591777097,330.027992731208,330.071673357551));
#53422=CARTESIAN_POINT('',(494.11591777097,330.027992731207,328.084784706188));
#53423=CARTESIAN_POINT('',(494.11591777097,71.6429959273593,330.071673357978));
#53424=CARTESIAN_POINT('',(494.11591777097,170.277992731204,330.071673357815));
#53425=CARTESIAN_POINT('',(494.11591777097,71.2060964085143,330.172163040955));
#53426=CARTESIAN_POINT('Origin',(494.11591777097,71.6429959273607,331.071673357978));
#53427=CARTESIAN_POINT('',(494.11591777097,31.4129895340987,349.500000551885));
#53428=CARTESIAN_POINT('',(494.11591777097,45.4823770730766,342.666383938589));
#53429=CARTESIAN_POINT('',(494.11591777097,-309.972007268783,349.500000552087));
#53430=CARTESIAN_POINT('',(494.11591777097,20.7779927312187,349.500000551892));
#53431=CARTESIAN_POINT('',(494.11591777097,-309.9720072688,320.77971275861));
#53432=CARTESIAN_POINT('',(494.11591777097,-309.972007268787,342.694928603579));
#53433=CARTESIAN_POINT('',(494.11591777097,-205.535060656547,320.779712758459));
#53434=CARTESIAN_POINT('Origin',(144.115917770964,29.1607759831001,339.708039952219));
#53435=CARTESIAN_POINT('',(454.11591777097,29.2757791802212,340.194634511016));
#53436=CARTESIAN_POINT('Origin',(454.11591777097,29.1607759830999,339.708039952218));
#53437=CARTESIAN_POINT('',(184.115917770964,29.2757791802213,340.194634511017));
#53438=CARTESIAN_POINT('Origin',(184.115917770964,29.1607759831001,339.708039952219));
#53439=CARTESIAN_POINT('',(184.115917770964,29.3792257425212,340.157795110731));
#53440=CARTESIAN_POINT('Origin',(184.115917770964,29.1607759831001,339.708039952219));
#53441=CARTESIAN_POINT('',(454.11591777097,29.3792257425211,340.15779511073));
#53442=CARTESIAN_POINT('',(144.115917770964,29.3792257425212,340.157795110731));
#53443=CARTESIAN_POINT('Origin',(454.11591777097,29.1607759830999,339.708039952218));
#53444=CARTESIAN_POINT('Ctrl Pts',(184.00935480449,29.1751198286203,340.231155563991));
#53445=CARTESIAN_POINT('Ctrl Pts',(184.035423606558,29.2301677887044,340.211275129548));
#53446=CARTESIAN_POINT('Ctrl Pts',(184.073633409372,29.2757791802213,340.194634511017));
#53447=CARTESIAN_POINT('Ctrl Pts',(184.115917770964,29.2757791802213,340.194634511017));
#53448=CARTESIAN_POINT('Ctrl Pts',(183.973228480221,29.2110507307293,340.230753219288));
#53449=CARTESIAN_POINT('Ctrl Pts',(184.008848284769,29.2659644027493,340.206430896902));
#53450=CARTESIAN_POINT('Ctrl Pts',(184.05978698227,29.3114732703414,340.186198464193));
#53451=CARTESIAN_POINT('Ctrl Pts',(184.115917770964,29.3114732703414,340.186198464193));
#53452=CARTESIAN_POINT('Ctrl Pts',(183.935350991415,29.2451273482303,340.222927797744));
#53453=CARTESIAN_POINT('Ctrl Pts',(183.981473610584,29.3004359815563,340.196056293685));
#53454=CARTESIAN_POINT('Ctrl Pts',(184.045598704041,29.3462340025403,340.173819468708));
#53455=CARTESIAN_POINT('Ctrl Pts',(184.115917770964,29.3462340025403,340.173819468708));
#53456=CARTESIAN_POINT('Ctrl Pts',(183.89746801131,29.2757791799883,340.208039952332));
#53457=CARTESIAN_POINT('Ctrl Pts',(183.954098540875,29.3324097096283,340.180534040856));
#53458=CARTESIAN_POINT('Ctrl Pts',(184.031409794092,29.3792257425212,340.157795110731));
#53459=CARTESIAN_POINT('Ctrl Pts',(184.115917770964,29.3792257425212,340.157795110731));
#53460=CARTESIAN_POINT('',(183.897468011221,29.2757791800603,340.208039952297));
#53461=CARTESIAN_POINT('Ctrl Pts',(183.897468011543,29.2757791802213,340.208039952219));
#53462=CARTESIAN_POINT('Ctrl Pts',(183.940017338202,29.2757791802213,340.208039952219));
#53463=CARTESIAN_POINT('Ctrl Pts',(183.980384153199,29.2757791801524,340.204672075941));
#53464=CARTESIAN_POINT('Ctrl Pts',(184.03989064397,29.2757791801524,340.199197864216));
#53465=CARTESIAN_POINT('Ctrl Pts',(184.061235828154,29.2757791802213,340.197088039368));
#53466=CARTESIAN_POINT('Ctrl Pts',(184.08771011489,29.2757791802213,340.195413965406));
#53467=CARTESIAN_POINT('Ctrl Pts',(184.094309573317,29.2757791802213,340.195080500941));
#53468=CARTESIAN_POINT('Ctrl Pts',(184.105942202007,29.2757791802213,340.194717028763));
#53469=CARTESIAN_POINT('Ctrl Pts',(184.110902933059,29.2757791802213,340.194634511017));
#53470=CARTESIAN_POINT('Ctrl Pts',(184.115917770964,29.2757791802213,340.194634511017));
#53471=CARTESIAN_POINT('Origin',(184.115917770914,28.3498010374177,340.657795110545));
#53472=CARTESIAN_POINT('Ctrl Pts',(454.11591777097,29.2757791802212,340.194634511016));
#53473=CARTESIAN_POINT('Ctrl Pts',(454.158236522942,29.2757791802212,340.194634511016));
#53474=CARTESIAN_POINT('Ctrl Pts',(454.196425407472,29.2301393405342,340.211285403533));
#53475=CARTESIAN_POINT('Ctrl Pts',(454.222480737526,29.1751198284492,340.231155564052));
#53476=CARTESIAN_POINT('Ctrl Pts',(454.11591777097,29.3114732703412,340.186198464192));
#53477=CARTESIAN_POINT('Ctrl Pts',(454.17209421151,29.3114732703412,340.186198464192));
#53478=CARTESIAN_POINT('Ctrl Pts',(454.223005665121,29.2659360239782,340.206443466406));
#53479=CARTESIAN_POINT('Ctrl Pts',(454.258607061825,29.2110507305572,340.230753219363));
#53480=CARTESIAN_POINT('Ctrl Pts',(454.11591777097,29.3462340025402,340.173819468707));
#53481=CARTESIAN_POINT('Ctrl Pts',(454.186294029236,29.3462340025402,340.173819468707));
#53482=CARTESIAN_POINT('Ctrl Pts',(454.250385767052,29.3004073986722,340.196070180577));
#53483=CARTESIAN_POINT('Ctrl Pts',(454.296484550663,29.2451273480572,340.222927797827));
#53484=CARTESIAN_POINT('Ctrl Pts',(454.11591777097,29.3792257425211,340.15779511073));
#53485=CARTESIAN_POINT('Ctrl Pts',(454.200494479196,29.3792257425211,340.15779511073));
#53486=CARTESIAN_POINT('Ctrl Pts',(454.27776626714,29.3323804436042,340.180548255603));
#53487=CARTESIAN_POINT('Ctrl Pts',(454.334367530801,29.2757791798112,340.208039952417));
#53488=CARTESIAN_POINT('',(454.334367530957,29.2757791799382,340.208039952355));
#53489=CARTESIAN_POINT('Ctrl Pts',(454.11591777097,29.2757791802212,340.194634511016));
#53490=CARTESIAN_POINT('Ctrl Pts',(454.120938618672,29.2757791802212,340.194634511016));
#53491=CARTESIAN_POINT('Ctrl Pts',(454.125905101463,29.2757791802212,340.194717142149));
#53492=CARTESIAN_POINT('Ctrl Pts',(454.137553824068,29.2757791802212,340.195081275641));
#53493=CARTESIAN_POINT('Ctrl Pts',(454.144163062791,29.2757791802211,340.19541545435));
#53494=CARTESIAN_POINT('Ctrl Pts',(454.171630390795,29.2757791802211,340.197153487144));
#53495=CARTESIAN_POINT('Ctrl Pts',(454.190169235585,29.2757791802179,340.199034540506));
#53496=CARTESIAN_POINT('Ctrl Pts',(454.251614129388,29.2757791802179,340.204685275396));
#53497=CARTESIAN_POINT('Ctrl Pts',(454.291901888822,29.2757791802212,340.208039952218));
#53498=CARTESIAN_POINT('Ctrl Pts',(454.334367530392,29.2757791802212,340.208039952218));
#53499=CARTESIAN_POINT('Origin',(454.115917771007,28.3498010373495,340.657795110577));
#53500=CARTESIAN_POINT('Origin',(454.11591777097,-10.7242208197788,340.208039952218));
#53501=CARTESIAN_POINT('',(454.11591777097,29.2757791802208,320.779712758118));
#53502=CARTESIAN_POINT('',(454.11591777097,29.2757791802212,340.208039952218));
#53503=CARTESIAN_POINT('',(454.11591777097,-10.7242208197793,320.779712758176));
#53504=CARTESIAN_POINT('',(454.11591777097,-75.6611674320453,320.77971275827));
#53505=CARTESIAN_POINT('',(454.11591777097,-10.7242208197788,340.208039952218));
#53506=CARTESIAN_POINT('Origin',(454.11591777097,29.2757791802212,340.208039952218));
#53507=CARTESIAN_POINT('',(493.61591777097,29.2757791802212,340.208039952218));
#53508=CARTESIAN_POINT('',(144.115917770964,29.2757791802213,340.208039952219));
#53509=CARTESIAN_POINT('Origin',(493.61591777097,29.2757791802205,340.763897945769));
#53510=CARTESIAN_POINT('',(386.615917770969,29.2757791802208,320.779712758118));
#53511=CARTESIAN_POINT('Origin',(144.115917770964,29.2757791802213,340.208039952219));
#53512=CARTESIAN_POINT('',(144.615917770964,29.2757791802213,340.208039952219));
#53513=CARTESIAN_POINT('',(144.115917770964,29.2757791802213,340.208039952219));
#53514=CARTESIAN_POINT('',(144.615917770964,69.1723326178359,320.829957599548));
#53515=CARTESIAN_POINT('',(144.615917770964,22.3118351489324,343.590484532268));
#53516=CARTESIAN_POINT('',(493.61591777097,69.1723326178358,320.829957599547));
#53517=CARTESIAN_POINT('',(144.115917770964,69.1723326178359,320.829957599548));
#53518=CARTESIAN_POINT('',(493.61591777097,22.4356686200921,343.530337602384));
#53519=CARTESIAN_POINT('Origin',(144.615917770964,-150.084339619182,340.708039952219));
#53520=CARTESIAN_POINT('',(144.115917770964,-10.7242208197794,340.708039952219));
#53521=CARTESIAN_POINT('Origin',(144.615917770964,-10.7242208197794,340.708039952219));
#53522=CARTESIAN_POINT('',(144.115917770964,-270.472007268788,340.708039952219));
#53523=CARTESIAN_POINT('Origin',(144.615917770964,-270.472007268788,340.708039952219));
#53524=CARTESIAN_POINT('',(144.115917770964,-150.084339619182,340.708039952219));
#53525=CARTESIAN_POINT('Origin',(144.615917770964,69.3907823772572,321.279712758061));
#53526=CARTESIAN_POINT('',(144.115917770964,69.3907823772572,321.279712758061));
#53527=CARTESIAN_POINT('Origin',(144.615917770964,69.3907823772572,321.279712758061));
#53528=CARTESIAN_POINT('',(144.615917770964,69.3907823772569,320.779712758061));
#53529=CARTESIAN_POINT('Origin',(144.615917770964,69.3907823772572,321.279712758061));
#53530=CARTESIAN_POINT('Origin',(144.615917770964,69.3907823772572,321.279712758061));
#53531=CARTESIAN_POINT('Origin',(493.61591777097,69.3907823772571,321.27971275806));
#53532=CARTESIAN_POINT('',(493.61591777097,69.3907823772568,320.77971275806));
#53533=CARTESIAN_POINT('Origin',(493.61591777097,69.3907823772571,321.27971275806));
#53534=CARTESIAN_POINT('Origin',(493.61591777097,69.3907823772571,321.27971275806));
#53535=CARTESIAN_POINT('Origin',(493.61591777097,69.3907823772571,321.27971275806));
#53536=CARTESIAN_POINT('Origin',(144.615917770964,330.027992731203,321.279712757683));
#53537=CARTESIAN_POINT('',(144.115917770964,330.027992731203,321.279712757683));
#53538=CARTESIAN_POINT('',(144.615917770964,330.027992731203,320.779712757683));
#53539=CARTESIAN_POINT('Origin',(144.615917770964,330.027992731203,321.279712757683));
#53540=CARTESIAN_POINT('',(144.615917770964,330.527992731203,321.279712757682));
#53541=CARTESIAN_POINT('Origin',(144.615917770964,330.027992731203,321.279712757683));
#53542=CARTESIAN_POINT('Origin',(144.615917770964,330.027992731203,321.279712757683));
#53543=CARTESIAN_POINT('Origin',(493.61591777097,330.027992731203,321.279712757682));
#53544=CARTESIAN_POINT('',(493.61591777097,330.527992731203,321.279712757681));
#53545=CARTESIAN_POINT('',(493.61591777097,330.027992731203,320.779712757682));
#53546=CARTESIAN_POINT('Origin',(493.61591777097,330.027992731203,321.279712757682));
#53547=CARTESIAN_POINT('Origin',(493.61591777097,330.027992731203,321.279712757682));
#53548=CARTESIAN_POINT('Origin',(493.61591777097,330.027992731203,321.279712757682));
#53549=CARTESIAN_POINT('Origin',(144.615917770964,330.027992731208,330.071673357552));
#53550=CARTESIAN_POINT('',(144.115917770964,330.027992731208,330.071673357552));
#53551=CARTESIAN_POINT('',(144.615917770964,330.527992731208,330.071673357552));
#53552=CARTESIAN_POINT('Origin',(144.615917770964,330.027992731208,330.071673357552));
#53553=CARTESIAN_POINT('',(144.615917770964,330.027992731209,330.571673357552));
#53554=CARTESIAN_POINT('Origin',(144.615917770964,330.027992731208,330.071673357552));
#53555=CARTESIAN_POINT('Origin',(144.615917770964,330.027992731208,330.071673357552));
#53556=CARTESIAN_POINT('Origin',(493.61591777097,330.027992731208,330.071673357551));
#53557=CARTESIAN_POINT('',(493.61591777097,330.027992731208,330.571673357551));
#53558=CARTESIAN_POINT('',(493.61591777097,330.527992731208,330.071673357551));
#53559=CARTESIAN_POINT('Origin',(493.61591777097,330.027992731208,330.071673357551));
#53560=CARTESIAN_POINT('Origin',(493.61591777097,330.027992731208,330.071673357551));
#53561=CARTESIAN_POINT('Origin',(493.61591777097,330.027992731208,330.071673357551));
#53562=CARTESIAN_POINT('Origin',(144.615917770964,71.6429959273609,331.071673357979));
#53563=CARTESIAN_POINT('',(144.115917770964,71.6429959273594,330.071673357979));
#53564=CARTESIAN_POINT('',(144.115917770964,71.2060964085144,330.172163040956));
#53565=CARTESIAN_POINT('Origin',(144.115917770964,71.6429959273609,331.07167335798));
#53566=CARTESIAN_POINT('',(144.615917770964,71.4245461679377,330.621918199468));
#53567=CARTESIAN_POINT('Origin',(144.615917770964,71.2060964085144,330.172163040956));
#53568=CARTESIAN_POINT('',(144.615917770964,71.6429959273606,330.571673357979));
#53569=CARTESIAN_POINT('Origin',(144.615917770964,71.6429959273609,331.071673357979));
#53570=CARTESIAN_POINT('Origin',(144.615917770964,71.6429959273594,330.071673357979));
#53571=CARTESIAN_POINT('Origin',(493.61591777097,71.6429959273607,331.071673357978));
#53572=CARTESIAN_POINT('',(493.61591777097,71.4245461679375,330.621918199467));
#53573=CARTESIAN_POINT('',(493.61591777097,71.6429959273605,330.571673357978));
#53574=CARTESIAN_POINT('Origin',(493.61591777097,71.6429959273607,331.071673357978));
#53575=CARTESIAN_POINT('Origin',(493.61591777097,71.2060964085143,330.172163040955));
#53576=CARTESIAN_POINT('Origin',(493.61591777097,71.6429959273593,330.071673357978));
#53577=CARTESIAN_POINT('Origin',(144.615917770964,31.4129895340988,349.500000551887));
#53578=CARTESIAN_POINT('',(144.115917770964,31.4129895340988,349.500000551887));
#53579=CARTESIAN_POINT('',(144.615917770964,31.6314392935211,349.949755710398));
#53580=CARTESIAN_POINT('Origin',(144.615917770964,31.4129895340988,349.500000551887));
#53581=CARTESIAN_POINT('',(144.615917770964,31.4129895340991,350.000000551887));
#53582=CARTESIAN_POINT('Origin',(144.615917770964,31.4129895340988,349.500000551887));
#53583=CARTESIAN_POINT('Origin',(144.615917770964,31.4129895340988,349.500000551887));
#53584=CARTESIAN_POINT('Origin',(144.615917770964,-309.972007268782,349.500000552088));
#53585=CARTESIAN_POINT('',(144.615917770964,-309.972007268782,350.000000552088));
#53586=CARTESIAN_POINT('',(144.615917770964,-310.472007268782,349.500000552088));
#53587=CARTESIAN_POINT('Origin',(144.615917770964,-309.972007268782,349.500000552088));
#53588=CARTESIAN_POINT('',(144.115917770964,-309.972007268782,349.500000552088));
#53589=CARTESIAN_POINT('Origin',(144.615917770964,-309.972007268782,349.500000552088));
#53590=CARTESIAN_POINT('Origin',(144.615917770964,-309.972007268782,349.500000552088));
#53591=CARTESIAN_POINT('Origin',(144.615917770964,20.9156603808258,349.500000551893));
#53592=CARTESIAN_POINT('',(144.115917770964,20.9156603808258,349.500000551893));
#53593=CARTESIAN_POINT('',(144.615917770964,20.9156603808261,350.000000551893));
#53594=CARTESIAN_POINT('Origin',(144.615917770964,-309.972007268786,343.293466961922));
#53595=CARTESIAN_POINT('',(144.115917770964,-309.972007268799,320.779712758612));
#53596=CARTESIAN_POINT('',(144.615917770964,-310.472007268788,320.779712758612));
#53597=CARTESIAN_POINT('Origin',(144.615917770964,-309.972007268799,320.779712758466));
#53598=CARTESIAN_POINT('',(144.615917770964,-310.472007268786,343.293466961922));
#53599=CARTESIAN_POINT('',(144.115917770964,-309.972007268786,343.293466961922));
#53600=CARTESIAN_POINT('Origin',(493.61591777097,31.4129895340987,349.500000551885));
#53601=CARTESIAN_POINT('',(493.61591777097,31.412989534099,350.000000551885));
#53602=CARTESIAN_POINT('Origin',(493.61591777097,31.4129895340987,349.500000551885));
#53603=CARTESIAN_POINT('',(493.61591777097,31.6314392935209,349.949755710397));
#53604=CARTESIAN_POINT('Origin',(493.61591777097,31.4129895340987,349.500000551885));
#53605=CARTESIAN_POINT('Origin',(493.61591777097,31.4129895340987,349.500000551885));
#53606=CARTESIAN_POINT('Origin',(493.61591777097,45.4823770730766,342.666383938589));
#53607=CARTESIAN_POINT('',(493.61591777097,45.7008268324999,343.116139097101));
#53608=CARTESIAN_POINT('Origin',(144.115917770964,31.4129895340988,349.500000551887));
#53609=CARTESIAN_POINT('',(144.115917770964,31.6314392935211,349.949755710398));
#53610=CARTESIAN_POINT('',(144.115917770964,31.4129895340991,350.000000551887));
#53611=CARTESIAN_POINT('Origin',(493.61591777097,-309.972007268783,349.500000552087));
#53612=CARTESIAN_POINT('',(493.61591777097,-310.472007268783,349.500000552087));
#53613=CARTESIAN_POINT('',(493.61591777097,-309.972007268782,350.000000552087));
#53614=CARTESIAN_POINT('Origin',(493.61591777097,-309.972007268783,349.500000552087));
#53615=CARTESIAN_POINT('Origin',(493.61591777097,-309.972007268783,349.500000552087));
#53616=CARTESIAN_POINT('Origin',(493.61591777097,-309.972007268783,349.500000552087));
#53617=CARTESIAN_POINT('Origin',(493.61591777097,-309.972007268787,342.694928603579));
#53618=CARTESIAN_POINT('',(493.61591777097,-310.472007268788,320.779712758611));
#53619=CARTESIAN_POINT('Origin',(493.61591777097,-309.9720072688,320.779712758464));
#53620=CARTESIAN_POINT('',(493.61591777097,-310.472007268787,342.69492860358));
#53621=CARTESIAN_POINT('Origin',(493.61591777097,20.7779927312187,349.500000551892));
#53622=CARTESIAN_POINT('',(493.61591777097,20.7779927312189,350.000000551892));
#53623=CARTESIAN_POINT('Origin',(144.115917770964,-309.972007268782,349.500000552088));
#53624=CARTESIAN_POINT('',(144.115917770964,-309.972007268782,350.000000552088));
#53625=CARTESIAN_POINT('',(144.115917770964,-310.472007268782,349.500000552088));
#53626=CARTESIAN_POINT('Origin',(144.615917770964,45.3585436019158,342.726530868474));
#53627=CARTESIAN_POINT('',(144.115917770964,45.3585436019158,342.726530868474));
#53628=CARTESIAN_POINT('',(144.615917770964,45.576993361338,343.176286026986));
#53629=CARTESIAN_POINT('Origin',(493.61591777097,170.277992731204,330.071673357815));
#53630=CARTESIAN_POINT('',(493.61591777097,170.277992731206,330.571673357815));
#53631=CARTESIAN_POINT('Origin',(144.115917770964,71.6429959273609,331.071673357979));
#53632=CARTESIAN_POINT('',(144.115917770964,71.6429959273606,330.571673357979));
#53633=CARTESIAN_POINT('',(144.115917770964,71.4245461679377,330.621918199468));
#53634=CARTESIAN_POINT('Origin',(144.615917770964,170.41566038081,330.071673357816));
#53635=CARTESIAN_POINT('',(144.115917770964,170.41566038081,330.071673357816));
#53636=CARTESIAN_POINT('',(144.615917770964,170.415660380812,330.571673357816));
#53637=CARTESIAN_POINT('Origin',(493.61591777097,330.027992731207,328.084784706188));
#53638=CARTESIAN_POINT('',(493.61591777097,330.527992731207,328.084784706188));
#53639=CARTESIAN_POINT('Origin',(144.115917770964,330.027992731208,330.071673357552));
#53640=CARTESIAN_POINT('',(144.115917770964,330.527992731208,330.071673357552));
#53641=CARTESIAN_POINT('',(144.115917770964,330.027992731209,330.571673357552));
#53642=CARTESIAN_POINT('Origin',(144.615917770964,330.027992731207,328.683323064531));
#53643=CARTESIAN_POINT('',(144.115917770964,330.027992731207,328.683323064531));
#53644=CARTESIAN_POINT('',(144.615917770964,330.527992731208,328.68332306453));
#53645=CARTESIAN_POINT('Origin',(493.61591777097,39.6518859556631,321.279712758103));
#53646=CARTESIAN_POINT('',(493.61591777097,39.6518859556628,320.779712758103));
#53647=CARTESIAN_POINT('Origin',(144.115917770964,330.027992731203,321.279712757683));
#53648=CARTESIAN_POINT('',(144.115917770964,330.027992731203,320.779712757683));
#53649=CARTESIAN_POINT('',(144.115917770964,330.527992731203,321.279712757682));
#53650=CARTESIAN_POINT('Origin',(144.615917770964,39.7895536052691,321.279712758104));
#53651=CARTESIAN_POINT('',(144.115917770964,39.7895536052691,321.279712758104));
#53652=CARTESIAN_POINT('',(144.615917770964,39.7895536052689,320.779712758104));
#53653=CARTESIAN_POINT('Origin',(493.61591777097,22.6541183795134,343.980092760897));
#53654=CARTESIAN_POINT('Origin',(144.115917770964,69.3907823772572,321.279712758061));
#53655=CARTESIAN_POINT('',(144.115917770964,69.3907823772569,320.779712758061));
#53656=CARTESIAN_POINT('Origin',(144.615917770964,22.5302849083546,344.04023969078));
#53657=CARTESIAN_POINT('',(144.115917770964,29.2757791802206,340.76389794577));
#53658=CARTESIAN_POINT('Origin',(144.615917770964,29.2757791802206,340.76389794577));
#53659=CARTESIAN_POINT('',(144.115917770964,22.5302849083546,344.04023969078));
#53660=CARTESIAN_POINT('Origin',(144.115917770964,-310.472007268782,350.000000552088));
#53661=CARTESIAN_POINT('',(454.11591777097,-310.472007268782,320.779712758611));
#53662=CARTESIAN_POINT('',(454.11591777097,-310.472007268782,340.208039952218));
#53663=CARTESIAN_POINT('',(406.615917770957,-310.472007268775,320.779712758611));
#53664=CARTESIAN_POINT('',(184.115917770964,-310.472007268788,320.779712758612));
#53665=CARTESIAN_POINT('',(251.615917770966,-310.472007268788,320.779712758612));
#53666=CARTESIAN_POINT('',(184.115917770964,-310.472007268788,340.208039952219));
#53667=CARTESIAN_POINT('Origin',(319.115917770967,-140.598114044283,320.779712758365));
#53668=CARTESIAN_POINT('',(144.115917770964,-270.472007268788,320.779712758554));
#53669=CARTESIAN_POINT('',(144.115917770964,-225.53506065655,320.779712758489));
#53670=CARTESIAN_POINT('',(184.115917770964,-270.472007268788,320.779712758554));
#53671=CARTESIAN_POINT('',(231.615917770965,-270.472007268788,320.779712758554));
#53672=CARTESIAN_POINT('',(184.115917770964,-205.53506065655,320.77971275846));
#53673=CARTESIAN_POINT('Origin',(144.115917770964,10.3033280304242,336.586933371568));
#53674=CARTESIAN_POINT('',(144.115917770964,-270.472007268788,340.208039952219));
#53675=CARTESIAN_POINT('',(144.115917770964,29.2757791802209,320.779712758119));
#53676=CARTESIAN_POINT('',(144.115917770964,29.2757791802213,340.208039952219));
#53677=CARTESIAN_POINT('',(144.115917770964,-10.7242208197791,320.779712758177));
#53678=CARTESIAN_POINT('',(144.115917770964,-75.6611674320451,320.779712758272));
#53679=CARTESIAN_POINT('',(144.115917770964,-10.7242208197787,340.208039952219));
#53680=CARTESIAN_POINT('Origin',(144.115917770964,31.5279927312201,350.000000551886));
#53681=CARTESIAN_POINT('',(444.115917770964,-296.660007268781,350.000000552079));
#53682=CARTESIAN_POINT('Origin',(444.115917770964,-290.472007268782,350.000000552075));
#53683=CARTESIAN_POINT('',(194.115917770964,-76.660007268782,350.00000055195));
#53684=CARTESIAN_POINT('Origin',(194.115917770964,-70.472007268782,350.000000551946));
#53685=CARTESIAN_POINT('',(194.115917770964,-100.472007268782,350.000000551964));
#53686=CARTESIAN_POINT('',(444.115917770964,-100.472007268782,350.000000551963));
#53687=CARTESIAN_POINT('',(169.115917770964,-100.472007268782,350.000000551964));
#53688=CARTESIAN_POINT('',(444.115917770964,-260.472007268782,350.000000552058));
#53689=CARTESIAN_POINT('',(444.115917770964,-34.4720072687781,350.000000551924));
#53690=CARTESIAN_POINT('',(194.115917770964,-260.472007268782,350.000000552058));
#53691=CARTESIAN_POINT('',(294.115917770964,-260.472007268782,350.000000552058));
#53692=CARTESIAN_POINT('',(194.115917770964,-114.472007268778,350.000000551972));
#53693=CARTESIAN_POINT('',(194.115917770964,-296.660007268781,350.00000055208));
#53694=CARTESIAN_POINT('Origin',(194.115917770964,-290.472007268782,350.000000552076));
#53695=CARTESIAN_POINT('',(444.115917770964,-76.6600072687821,350.000000551949));
#53696=CARTESIAN_POINT('Origin',(444.115917770964,-70.4720072687821,350.000000551946));
#53697=CARTESIAN_POINT('Origin',(144.115917770964,71.5279927302396,330.57167335798));
#53698=CARTESIAN_POINT('Origin',(144.115917770964,330.527992731209,330.571673357551));
#53699=CARTESIAN_POINT('Origin',(144.115917770964,330.527992731203,320.779712757682));
#53700=CARTESIAN_POINT('Origin',(144.115917770964,69.2757791801369,320.779712758061));
#53701=CARTESIAN_POINT('Origin',(444.115917770964,-290.472007268782,349.500000551887));
#53702=CARTESIAN_POINT('',(444.115917770964,-295.660007268782,349.000000551699));
#53703=CARTESIAN_POINT('Origin',(444.115917770964,-290.472007268782,349.000000551699));
#53704=CARTESIAN_POINT('',(444.115917770964,-296.160007268782,349.50000055189));
#53705=CARTESIAN_POINT('Origin',(444.115917770964,-290.472007268782,355.858039952218));
#53706=CARTESIAN_POINT('',(444.115917770964,-295.660007268782,341.208039952218));
#53707=CARTESIAN_POINT('',(444.115917770964,-295.660007268782,355.858039952218));
#53708=CARTESIAN_POINT('',(444.115917770964,-285.284007268782,341.208039952218));
#53709=CARTESIAN_POINT('Origin',(444.115917770964,-290.472007268782,341.208039952218));
#53710=CARTESIAN_POINT('Origin',(444.115917770964,-290.472007268782,341.208039952218));
#53711=CARTESIAN_POINT('Origin',(444.115917770964,-70.4720072687823,349.500000551887));
#53712=CARTESIAN_POINT('',(444.115917770964,-75.6600072687826,349.000000551829));
#53713=CARTESIAN_POINT('Origin',(444.115917770964,-70.4720072687826,349.000000551829));
#53714=CARTESIAN_POINT('',(444.115917770964,-76.1600072687821,349.50000055189));
#53715=CARTESIAN_POINT('Origin',(444.115917770964,-70.4720072687826,355.858039952218));
#53716=CARTESIAN_POINT('',(444.115917770964,-75.6600072687826,341.208039952218));
#53717=CARTESIAN_POINT('',(444.115917770964,-75.6600072687826,355.858039952218));
#53718=CARTESIAN_POINT('',(444.115917770964,-65.2840072687832,341.208039952218));
#53719=CARTESIAN_POINT('Origin',(444.115917770964,-70.4720072687833,341.208039952218));
#53720=CARTESIAN_POINT('Origin',(444.115917770964,-70.4720072687833,341.208039952218));
#53721=CARTESIAN_POINT('Origin',(194.115917770964,-70.4720072687822,349.500000551888));
#53722=CARTESIAN_POINT('',(194.115917770964,-75.6600072687825,349.00000055183));
#53723=CARTESIAN_POINT('Origin',(194.115917770964,-70.4720072687825,349.00000055183));
#53724=CARTESIAN_POINT('',(194.115917770964,-76.160007268782,349.500000551891));
#53725=CARTESIAN_POINT('Origin',(194.115917770964,-70.4720072687825,355.858039952219));
#53726=CARTESIAN_POINT('',(194.115917770964,-75.6600072687825,341.208039952219));
#53727=CARTESIAN_POINT('',(194.115917770964,-75.6600072687825,355.858039952219));
#53728=CARTESIAN_POINT('',(194.115917770964,-65.2840072687831,341.208039952219));
#53729=CARTESIAN_POINT('Origin',(194.115917770964,-70.4720072687832,341.208039952219));
#53730=CARTESIAN_POINT('Origin',(194.115917770964,-70.4720072687832,341.208039952219));
#53731=CARTESIAN_POINT('Origin',(194.115917770964,-290.472007268782,349.500000551888));
#53732=CARTESIAN_POINT('',(194.115917770964,-295.660007268782,349.0000005517));
#53733=CARTESIAN_POINT('Origin',(194.115917770964,-290.472007268782,349.0000005517));
#53734=CARTESIAN_POINT('',(194.115917770964,-296.160007268782,349.500000551891));
#53735=CARTESIAN_POINT('Origin',(194.115917770964,-290.472007268782,355.858039952219));
#53736=CARTESIAN_POINT('',(194.115917770964,-295.660007268782,341.208039952219));
#53737=CARTESIAN_POINT('',(194.115917770964,-295.660007268782,355.858039952219));
#53738=CARTESIAN_POINT('',(194.115917770964,-285.284007268782,341.208039952218));
#53739=CARTESIAN_POINT('Origin',(194.115917770964,-290.472007268782,341.208039952219));
#53740=CARTESIAN_POINT('Origin',(194.115917770964,-290.472007268782,341.208039952219));
#53741=CARTESIAN_POINT('Origin',(444.115917770964,-290.472007268782,340.708039952218));
#53742=CARTESIAN_POINT('',(444.115917770964,-284.784007268782,340.708039952218));
#53743=CARTESIAN_POINT('Origin',(444.115917770964,-70.4720072687825,340.708039952218));
#53744=CARTESIAN_POINT('',(444.115917770964,-64.7840072687825,340.708039952218));
#53745=CARTESIAN_POINT('Origin',(194.115917770964,-70.4720072687824,340.708039952219));
#53746=CARTESIAN_POINT('',(194.115917770964,-64.7840072687824,340.708039952219));
#53747=CARTESIAN_POINT('Origin',(194.115917770964,-290.472007268782,340.708039952218));
#53748=CARTESIAN_POINT('',(194.115917770964,-284.784007268782,340.708039952218));
#53749=CARTESIAN_POINT('Origin',(144.115917770964,-270.472007268788,340.208039952219));
#53750=CARTESIAN_POINT('',(184.115917770964,-270.472007268788,340.208039952219));
#53751=CARTESIAN_POINT('Origin',(184.115917770964,-270.472007268788,340.208039952219));
#53752=CARTESIAN_POINT('Origin',(319.115917770967,-140.598114044283,320.779712758365));
#53753=CARTESIAN_POINT('',(184.115917770964,29.2757791802209,320.779712758119));
#53754=CARTESIAN_POINT('',(231.615917770966,29.2757791802208,320.779712758119));
#53755=CARTESIAN_POINT('',(184.115917770964,-10.7242208197792,320.779712758177));
#53756=CARTESIAN_POINT('',(184.115917770964,-55.6611674320452,320.779712758242));
#53757=CARTESIAN_POINT('',(251.615917770966,-10.7242208197792,320.779712758177));
#53758=CARTESIAN_POINT('Origin',(184.115917770964,-10.7242208197787,340.208039952219));
#53759=CARTESIAN_POINT('',(184.115917770964,-10.7242208197787,340.208039952219));
#53760=CARTESIAN_POINT('Origin',(144.115917770964,29.2757791802213,340.208039952219));
#53761=CARTESIAN_POINT('',(184.115917770964,29.2757791802213,340.208039952219));
#53762=CARTESIAN_POINT('Origin',(184.115917770964,29.2757791802213,340.208039952219));
#53763=CARTESIAN_POINT('Origin',(454.11591777097,-310.472007268782,340.208039952218));
#53764=CARTESIAN_POINT('',(454.11591777097,-270.472007268782,320.779712758553));
#53765=CARTESIAN_POINT('',(454.11591777097,-225.535060656547,320.779712758488));
#53766=CARTESIAN_POINT('',(454.11591777097,-270.472007268782,340.208039952218));
#53767=CARTESIAN_POINT('Origin',(454.11591777097,-270.472007268782,340.208039952218));
#53768=CARTESIAN_POINT('',(386.615917770969,-270.472007268782,320.779712758553));
#53769=CARTESIAN_POINT('Origin',(319.115917770967,-140.598114044283,320.779712758365));
#53770=CARTESIAN_POINT('Origin',(319.115917770967,-140.598114044283,320.779712758365));
#53771=CARTESIAN_POINT('',(406.615917770969,-10.7242208197793,320.779712758176));
#53772=CARTESIAN_POINT('Origin',(494.11591777097,-10.7242208197789,340.208039952218));
#53773=CARTESIAN_POINT('Origin',(444.115917770964,-260.472007268782,340.208039952218));
#53774=CARTESIAN_POINT('',(194.115917770964,-260.472007268782,340.208039952219));
#53775=CARTESIAN_POINT('',(444.115917770964,-260.472007268782,340.208039952218));
#53776=CARTESIAN_POINT('Origin',(444.115917770964,-100.472007268783,340.208039952218));
#53777=CARTESIAN_POINT('',(444.115917770964,-100.472007268783,340.208039952218));
#53778=CARTESIAN_POINT('Origin',(194.115917770964,-100.472007268783,340.208039952219));
#53779=CARTESIAN_POINT('',(194.115917770964,-100.472007268783,340.208039952219));
#53780=CARTESIAN_POINT('Origin',(194.115917770964,-260.472007268782,340.208039952219));
#53781=CARTESIAN_POINT('',(0.,0.,0.));
#53782=CARTESIAN_POINT('Origin',(489.615917770968,-307.972007269816,-379.220287241398));
#53783=CARTESIAN_POINT('',(457.61591777097,-307.972007268858,280.779712758602));
#53784=CARTESIAN_POINT('',(489.61591777097,-307.972007268858,280.779712758602));
#53785=CARTESIAN_POINT('',(481.61591777097,-307.972007268858,280.779712758602));
#53786=CARTESIAN_POINT('',(489.615917770968,-307.972007269816,-379.220287241398));
#53787=CARTESIAN_POINT('',(489.615917770968,-307.972007269816,-379.220287241398));
#53788=CARTESIAN_POINT('',(457.615917770968,-307.972007269816,-379.220287241398));
#53789=CARTESIAN_POINT('',(481.615917770968,-307.972007269816,-379.220287241398));
#53790=CARTESIAN_POINT('',(457.615917770968,-307.972007269816,-379.220287241398));
#53791=CARTESIAN_POINT('Origin',(489.615917770968,-305.972007269816,-379.220287241401));
#53792=CARTESIAN_POINT('',(491.61591777097,-305.972007268858,280.779712758599));
#53793=CARTESIAN_POINT('Origin',(489.61591777097,-305.972007268858,280.779712758599));
#53794=CARTESIAN_POINT('',(491.615917770968,-305.972007269816,-379.220287241401));
#53795=CARTESIAN_POINT('',(491.615917770968,-305.972007269816,-379.220287241401));
#53796=CARTESIAN_POINT('Origin',(489.615917770968,-305.972007269816,-379.220287241401));
#53797=CARTESIAN_POINT('Origin',(491.615917770968,-273.972007269816,-379.220287241447));
#53798=CARTESIAN_POINT('',(491.61591777097,-273.972007268858,280.779712758553));
#53799=CARTESIAN_POINT('',(491.61591777097,-281.972007268858,280.779712758564));
#53800=CARTESIAN_POINT('',(491.615917770968,-273.972007269816,-379.220287241447));
#53801=CARTESIAN_POINT('',(491.615917770968,-273.972007269816,-379.220287241447));
#53802=CARTESIAN_POINT('',(491.615917770968,-281.972007269816,-379.220287241436));
#53803=CARTESIAN_POINT('Origin',(489.615917770968,-273.972007269816,-379.220287241447));
#53804=CARTESIAN_POINT('',(489.61591777097,-271.972007268858,280.77971275855));
#53805=CARTESIAN_POINT('Origin',(489.61591777097,-273.972007268858,280.779712758553));
#53806=CARTESIAN_POINT('',(489.615917770968,-271.972007269816,-379.22028724145));
#53807=CARTESIAN_POINT('',(489.615917770968,-271.972007269816,-379.22028724145));
#53808=CARTESIAN_POINT('Origin',(489.615917770968,-273.972007269816,-379.220287241447));
#53809=CARTESIAN_POINT('Origin',(493.615917770968,-273.972007269816,-379.220287241447));
#53810=CARTESIAN_POINT('',(493.61591777097,-273.972007268858,280.779712758553));
#53811=CARTESIAN_POINT('',(493.61591777097,-305.972007268858,280.779712758599));
#53812=CARTESIAN_POINT('',(493.61591777097,-281.972007268858,280.779712758564));
#53813=CARTESIAN_POINT('',(493.615917770968,-305.972007269816,-379.220287241401));
#53814=CARTESIAN_POINT('',(493.615917770968,-305.972007269816,-379.220287241401));
#53815=CARTESIAN_POINT('',(493.615917770968,-273.972007269816,-379.220287241447));
#53816=CARTESIAN_POINT('',(493.615917770968,-281.972007269816,-379.220287241436));
#53817=CARTESIAN_POINT('',(493.615917770968,-273.972007269816,-379.220287241447));
#53818=CARTESIAN_POINT('Origin',(489.615917770968,-305.972007269816,-379.220287241401));
#53819=CARTESIAN_POINT('',(489.61591777097,-309.972007268858,280.779712758605));
#53820=CARTESIAN_POINT('Origin',(489.61591777097,-305.972007268858,280.779712758599));
#53821=CARTESIAN_POINT('',(489.615917770968,-309.972007269816,-379.220287241395));
#53822=CARTESIAN_POINT('',(489.615917770968,-309.972007269816,-379.220287241395));
#53823=CARTESIAN_POINT('Origin',(489.615917770968,-305.972007269816,-379.220287241401));
#53824=CARTESIAN_POINT('Origin',(489.615917770968,-309.972007269816,-379.220287241395));
#53825=CARTESIAN_POINT('',(457.61591777097,-309.972007268858,280.779712758605));
#53826=CARTESIAN_POINT('',(481.61591777097,-309.972007268858,280.779712758605));
#53827=CARTESIAN_POINT('',(457.615917770968,-309.972007269816,-379.220287241395));
#53828=CARTESIAN_POINT('',(457.615917770968,-309.972007269816,-379.220287241395));
#53829=CARTESIAN_POINT('',(481.615917770968,-309.972007269816,-379.220287241395));
#53830=CARTESIAN_POINT('Origin',(457.615917770968,-305.972007269816,-379.220287241401));
#53831=CARTESIAN_POINT('',(453.61591777097,-305.972007268858,280.779712758599));
#53832=CARTESIAN_POINT('Origin',(457.61591777097,-305.972007268858,280.779712758599));
#53833=CARTESIAN_POINT('',(453.615917770968,-305.972007269816,-379.220287241401));
#53834=CARTESIAN_POINT('',(453.615917770968,-305.972007269816,-379.220287241401));
#53835=CARTESIAN_POINT('Origin',(457.615917770968,-305.972007269816,-379.220287241401));
#53836=CARTESIAN_POINT('Origin',(457.615917770968,-271.972007269816,-379.22028724145));
#53837=CARTESIAN_POINT('',(457.61591777097,-271.972007268858,280.77971275855));
#53838=CARTESIAN_POINT('',(465.61591777097,-271.972007268858,280.77971275855));
#53839=CARTESIAN_POINT('',(457.615917770968,-271.972007269816,-379.22028724145));
#53840=CARTESIAN_POINT('',(457.615917770968,-271.972007269816,-379.22028724145));
#53841=CARTESIAN_POINT('',(465.615917770968,-271.972007269816,-379.22028724145));
#53842=CARTESIAN_POINT('Origin',(457.615917770968,-305.972007269816,-379.220287241401));
#53843=CARTESIAN_POINT('',(455.61591777097,-305.972007268858,280.779712758599));
#53844=CARTESIAN_POINT('Origin',(457.61591777097,-305.972007268858,280.779712758599));
#53845=CARTESIAN_POINT('',(455.615917770968,-305.972007269816,-379.220287241401));
#53846=CARTESIAN_POINT('Origin',(457.615917770968,-305.972007269816,-379.220287241401));
#53847=CARTESIAN_POINT('',(455.615917770968,-305.972007269816,-379.220287241401));
#53848=CARTESIAN_POINT('Origin',(455.615917770968,-305.972007269816,-379.220287241401));
#53849=CARTESIAN_POINT('',(455.61591777097,-273.972007268858,280.779712758553));
#53850=CARTESIAN_POINT('',(455.61591777097,-297.972007268858,280.779712758588));
#53851=CARTESIAN_POINT('',(455.615917770968,-273.972007269816,-379.220287241447));
#53852=CARTESIAN_POINT('',(455.615917770968,-297.972007269816,-379.220287241412));
#53853=CARTESIAN_POINT('',(455.615917770968,-273.972007269816,-379.220287241447));
#53854=CARTESIAN_POINT('Origin',(457.615917770968,-273.972007269816,-379.220287241447));
#53855=CARTESIAN_POINT('Origin',(457.61591777097,-273.972007268858,280.779712758553));
#53856=CARTESIAN_POINT('Origin',(457.615917770968,-273.972007269816,-379.220287241447));
#53857=CARTESIAN_POINT('Origin',(453.615917770968,-305.972007269816,-379.220287241401));
#53858=CARTESIAN_POINT('',(453.61591777097,-273.972007268858,280.779712758553));
#53859=CARTESIAN_POINT('',(453.61591777097,-297.972007268858,280.779712758588));
#53860=CARTESIAN_POINT('',(453.615917770968,-273.972007269816,-379.220287241447));
#53861=CARTESIAN_POINT('',(453.615917770968,-273.972007269816,-379.220287241447));
#53862=CARTESIAN_POINT('',(453.615917770968,-297.972007269816,-379.220287241412));
#53863=CARTESIAN_POINT('Origin',(457.615917770968,-273.972007269816,-379.220287241447));
#53864=CARTESIAN_POINT('',(457.61591777097,-269.972007268858,280.779712758547));
#53865=CARTESIAN_POINT('Origin',(457.61591777097,-273.972007268858,280.779712758553));
#53866=CARTESIAN_POINT('',(457.615917770968,-269.972007269816,-379.220287241453));
#53867=CARTESIAN_POINT('',(457.615917770968,-269.972007269816,-379.220287241453));
#53868=CARTESIAN_POINT('Origin',(457.615917770968,-273.972007269816,-379.220287241447));
#53869=CARTESIAN_POINT('Origin',(457.615917770968,-269.972007269816,-379.220287241453));
#53870=CARTESIAN_POINT('',(489.61591777097,-269.972007268858,280.779712758547));
#53871=CARTESIAN_POINT('',(465.61591777097,-269.972007268858,280.779712758547));
#53872=CARTESIAN_POINT('',(489.615917770968,-269.972007269816,-379.220287241453));
#53873=CARTESIAN_POINT('',(489.615917770968,-269.972007269816,-379.220287241453));
#53874=CARTESIAN_POINT('',(465.615917770968,-269.972007269816,-379.220287241453));
#53875=CARTESIAN_POINT('Origin',(489.615917770968,-273.972007269816,-379.220287241447));
#53876=CARTESIAN_POINT('Origin',(489.61591777097,-273.972007268858,280.779712758553));
#53877=CARTESIAN_POINT('Origin',(489.615917770968,-273.972007269816,-379.220287241447));
#53878=CARTESIAN_POINT('Origin',(473.615917770968,-289.972007269816,-379.220287241424));
#53879=CARTESIAN_POINT('Origin',(473.61591777097,-289.972007268858,280.779712758576));
#53880=CARTESIAN_POINT('Origin',(489.615917770968,292.027992730186,-379.220287242269));
#53881=CARTESIAN_POINT('',(457.61591777097,292.027992731145,281.279712757731));
#53882=CARTESIAN_POINT('',(489.61591777097,292.027992731144,281.279712757731));
#53883=CARTESIAN_POINT('',(481.61591777097,292.027992731145,281.279712757731));
#53884=CARTESIAN_POINT('',(489.615917770968,292.027992730186,-379.220287242269));
#53885=CARTESIAN_POINT('',(489.615917770968,292.027992730186,-379.220287242269));
#53886=CARTESIAN_POINT('',(457.615917770968,292.027992730186,-379.220287242269));
#53887=CARTESIAN_POINT('',(481.615917770968,292.027992730186,-379.220287242269));
#53888=CARTESIAN_POINT('',(457.615917770968,292.027992730186,-379.220287242269));
#53889=CARTESIAN_POINT('Origin',(489.615917770968,294.027992730186,-379.220287242272));
#53890=CARTESIAN_POINT('',(491.61591777097,294.027992731144,281.279712757728));
#53891=CARTESIAN_POINT('Origin',(489.61591777097,294.027992731144,281.279712757728));
#53892=CARTESIAN_POINT('',(491.615917770968,294.027992730186,-379.220287242272));
#53893=CARTESIAN_POINT('',(491.615917770968,294.027992730186,-379.220287242272));
#53894=CARTESIAN_POINT('Origin',(489.615917770968,294.027992730186,-379.220287242272));
#53895=CARTESIAN_POINT('Origin',(491.615917770968,326.027992730186,-379.220287242318));
#53896=CARTESIAN_POINT('',(491.61591777097,326.027992731144,281.279712757682));
#53897=CARTESIAN_POINT('',(491.61591777097,318.027992731144,281.279712757693));
#53898=CARTESIAN_POINT('',(491.615917770968,326.027992730186,-379.220287242318));
#53899=CARTESIAN_POINT('',(491.615917770968,326.027992730186,-379.220287242318));
#53900=CARTESIAN_POINT('',(491.615917770968,318.027992730186,-379.220287242307));
#53901=CARTESIAN_POINT('Origin',(489.615917770968,326.027992730186,-379.220287242318));
#53902=CARTESIAN_POINT('',(489.61591777097,328.027992731144,281.279712757679));
#53903=CARTESIAN_POINT('Origin',(489.61591777097,326.027992731144,281.279712757682));
#53904=CARTESIAN_POINT('',(489.615917770968,328.027992730186,-379.220287242321));
#53905=CARTESIAN_POINT('',(489.615917770968,328.027992730186,-379.220287242321));
#53906=CARTESIAN_POINT('Origin',(489.615917770968,326.027992730186,-379.220287242318));
#53907=CARTESIAN_POINT('Origin',(493.615917770968,326.027992730186,-379.220287242318));
#53908=CARTESIAN_POINT('',(493.61591777097,326.027992731144,281.279712757682));
#53909=CARTESIAN_POINT('',(493.61591777097,294.027992731144,281.279712757728));
#53910=CARTESIAN_POINT('',(493.61591777097,318.027992731144,281.279712757693));
#53911=CARTESIAN_POINT('',(493.615917770968,294.027992730186,-379.220287242272));
#53912=CARTESIAN_POINT('',(493.615917770968,294.027992730186,-379.220287242272));
#53913=CARTESIAN_POINT('',(493.615917770968,326.027992730186,-379.220287242318));
#53914=CARTESIAN_POINT('',(493.615917770968,318.027992730186,-379.220287242307));
#53915=CARTESIAN_POINT('',(493.615917770968,326.027992730186,-379.220287242318));
#53916=CARTESIAN_POINT('Origin',(489.615917770968,294.027992730186,-379.220287242272));
#53917=CARTESIAN_POINT('',(489.61591777097,290.027992731144,281.279712757734));
#53918=CARTESIAN_POINT('Origin',(489.61591777097,294.027992731144,281.279712757728));
#53919=CARTESIAN_POINT('',(489.615917770968,290.027992730186,-379.220287242266));
#53920=CARTESIAN_POINT('',(489.615917770968,290.027992730186,-379.220287242266));
#53921=CARTESIAN_POINT('Origin',(489.615917770968,294.027992730186,-379.220287242272));
#53922=CARTESIAN_POINT('Origin',(489.615917770968,290.027992730186,-379.220287242266));
#53923=CARTESIAN_POINT('',(457.61591777097,290.027992731145,281.279712757734));
#53924=CARTESIAN_POINT('',(481.61591777097,290.027992731144,281.279712757734));
#53925=CARTESIAN_POINT('',(457.615917770968,290.027992730186,-379.220287242266));
#53926=CARTESIAN_POINT('',(457.615917770968,290.027992730186,-379.220287242266));
#53927=CARTESIAN_POINT('',(481.615917770968,290.027992730186,-379.220287242266));
#53928=CARTESIAN_POINT('Origin',(457.615917770968,294.027992730186,-379.220287242272));
#53929=CARTESIAN_POINT('',(453.61591777097,294.027992731144,281.279712757728));
#53930=CARTESIAN_POINT('Origin',(457.61591777097,294.027992731144,281.279712757728));
#53931=CARTESIAN_POINT('',(453.615917770968,294.027992730186,-379.220287242272));
#53932=CARTESIAN_POINT('',(453.615917770968,294.027992730186,-379.220287242272));
#53933=CARTESIAN_POINT('Origin',(457.615917770968,294.027992730186,-379.220287242272));
#53934=CARTESIAN_POINT('Origin',(457.615917770968,328.027992730186,-379.220287242321));
#53935=CARTESIAN_POINT('',(457.61591777097,328.027992731145,281.279712757679));
#53936=CARTESIAN_POINT('',(465.61591777097,328.027992731145,281.279712757679));
#53937=CARTESIAN_POINT('',(457.615917770968,328.027992730186,-379.220287242321));
#53938=CARTESIAN_POINT('',(457.615917770968,328.027992730186,-379.220287242321));
#53939=CARTESIAN_POINT('',(465.615917770968,328.027992730186,-379.220287242321));
#53940=CARTESIAN_POINT('Origin',(457.615917770968,294.027992730186,-379.220287242272));
#53941=CARTESIAN_POINT('',(455.61591777097,294.027992731144,281.279712757728));
#53942=CARTESIAN_POINT('Origin',(457.61591777097,294.027992731144,281.279712757728));
#53943=CARTESIAN_POINT('',(455.615917770968,294.027992730186,-379.220287242272));
#53944=CARTESIAN_POINT('Origin',(457.615917770968,294.027992730186,-379.220287242272));
#53945=CARTESIAN_POINT('',(455.615917770968,294.027992730186,-379.220287242272));
#53946=CARTESIAN_POINT('Origin',(455.615917770968,294.027992730186,-379.220287242272));
#53947=CARTESIAN_POINT('',(455.61591777097,326.027992731144,281.279712757682));
#53948=CARTESIAN_POINT('',(455.61591777097,302.027992731145,281.279712757717));
#53949=CARTESIAN_POINT('',(455.615917770968,326.027992730186,-379.220287242318));
#53950=CARTESIAN_POINT('',(455.615917770968,302.027992730186,-379.220287242283));
#53951=CARTESIAN_POINT('',(455.615917770968,326.027992730186,-379.220287242318));
#53952=CARTESIAN_POINT('Origin',(457.615917770968,326.027992730186,-379.220287242318));
#53953=CARTESIAN_POINT('Origin',(457.61591777097,326.027992731144,281.279712757682));
#53954=CARTESIAN_POINT('Origin',(457.615917770968,326.027992730186,-379.220287242318));
#53955=CARTESIAN_POINT('Origin',(453.615917770968,294.027992730186,-379.220287242272));
#53956=CARTESIAN_POINT('',(453.61591777097,326.027992731144,281.279712757682));
#53957=CARTESIAN_POINT('',(453.61591777097,302.027992731145,281.279712757717));
#53958=CARTESIAN_POINT('',(453.615917770968,326.027992730186,-379.220287242318));
#53959=CARTESIAN_POINT('',(453.615917770968,326.027992730186,-379.220287242318));
#53960=CARTESIAN_POINT('',(453.615917770968,302.027992730186,-379.220287242283));
#53961=CARTESIAN_POINT('Origin',(457.615917770968,326.027992730186,-379.220287242318));
#53962=CARTESIAN_POINT('',(457.61591777097,330.027992731144,281.279712757676));
#53963=CARTESIAN_POINT('Origin',(457.61591777097,326.027992731144,281.279712757682));
#53964=CARTESIAN_POINT('',(457.615917770968,330.027992730186,-379.220287242324));
#53965=CARTESIAN_POINT('',(457.615917770968,330.027992730186,-379.220287242324));
#53966=CARTESIAN_POINT('Origin',(457.615917770968,326.027992730186,-379.220287242318));
#53967=CARTESIAN_POINT('Origin',(457.615917770968,330.027992730186,-379.220287242324));
#53968=CARTESIAN_POINT('',(489.61591777097,330.027992731144,281.279712757676));
#53969=CARTESIAN_POINT('',(465.61591777097,330.027992731144,281.279712757676));
#53970=CARTESIAN_POINT('',(489.615917770968,330.027992730186,-379.220287242324));
#53971=CARTESIAN_POINT('',(489.615917770968,330.027992730186,-379.220287242324));
#53972=CARTESIAN_POINT('',(465.615917770968,330.027992730186,-379.220287242324));
#53973=CARTESIAN_POINT('Origin',(489.615917770968,326.027992730186,-379.220287242318));
#53974=CARTESIAN_POINT('Origin',(489.61591777097,326.027992731144,281.279712757682));
#53975=CARTESIAN_POINT('Origin',(489.615917770968,326.027992730186,-379.220287242318));
#53976=CARTESIAN_POINT('Origin',(473.615917770968,310.027992730186,-379.220287242295));
#53977=CARTESIAN_POINT('Origin',(473.61591777097,310.027992731145,281.279712757705));
#53978=CARTESIAN_POINT('Origin',(180.115917770962,292.027992730186,-379.220287242268));
#53979=CARTESIAN_POINT('',(148.115917770964,292.027992731145,281.279712757732));
#53980=CARTESIAN_POINT('',(180.115917770964,292.027992731144,281.279712757732));
#53981=CARTESIAN_POINT('',(172.115917770964,292.027992731145,281.279712757732));
#53982=CARTESIAN_POINT('',(180.115917770962,292.027992730186,-379.220287242268));
#53983=CARTESIAN_POINT('',(180.115917770962,292.027992730186,-379.220287242268));
#53984=CARTESIAN_POINT('',(148.115917770962,292.027992730186,-379.220287242268));
#53985=CARTESIAN_POINT('',(172.115917770962,292.027992730186,-379.220287242268));
#53986=CARTESIAN_POINT('',(148.115917770962,292.027992730186,-379.220287242268));
#53987=CARTESIAN_POINT('Origin',(180.115917770962,294.027992730186,-379.220287242271));
#53988=CARTESIAN_POINT('',(182.115917770964,294.027992731144,281.279712757729));
#53989=CARTESIAN_POINT('Origin',(180.115917770964,294.027992731144,281.279712757729));
#53990=CARTESIAN_POINT('',(182.115917770962,294.027992730186,-379.220287242271));
#53991=CARTESIAN_POINT('',(182.115917770962,294.027992730186,-379.220287242271));
#53992=CARTESIAN_POINT('Origin',(180.115917770962,294.027992730186,-379.220287242271));
#53993=CARTESIAN_POINT('Origin',(182.115917770962,326.027992730186,-379.220287242317));
#53994=CARTESIAN_POINT('',(182.115917770964,326.027992731144,281.279712757683));
#53995=CARTESIAN_POINT('',(182.115917770964,318.027992731144,281.279712757694));
#53996=CARTESIAN_POINT('',(182.115917770962,326.027992730186,-379.220287242317));
#53997=CARTESIAN_POINT('',(182.115917770962,326.027992730186,-379.220287242317));
#53998=CARTESIAN_POINT('',(182.115917770962,318.027992730186,-379.220287242306));
#53999=CARTESIAN_POINT('Origin',(180.115917770962,326.027992730186,-379.220287242317));
#54000=CARTESIAN_POINT('',(180.115917770964,328.027992731144,281.27971275768));
#54001=CARTESIAN_POINT('Origin',(180.115917770964,326.027992731144,281.279712757683));
#54002=CARTESIAN_POINT('',(180.115917770962,328.027992730186,-379.22028724232));
#54003=CARTESIAN_POINT('',(180.115917770962,328.027992730186,-379.22028724232));
#54004=CARTESIAN_POINT('Origin',(180.115917770962,326.027992730186,-379.220287242317));
#54005=CARTESIAN_POINT('Origin',(184.115917770962,326.027992730186,-379.220287242317));
#54006=CARTESIAN_POINT('',(184.115917770964,326.027992731144,281.279712757683));
#54007=CARTESIAN_POINT('',(184.115917770964,294.027992731144,281.279712757729));
#54008=CARTESIAN_POINT('',(184.115917770964,318.027992731144,281.279712757694));
#54009=CARTESIAN_POINT('',(184.115917770962,294.027992730186,-379.220287242271));
#54010=CARTESIAN_POINT('',(184.115917770962,294.027992730186,-379.220287242271));
#54011=CARTESIAN_POINT('',(184.115917770962,326.027992730186,-379.220287242317));
#54012=CARTESIAN_POINT('',(184.115917770962,318.027992730186,-379.220287242306));
#54013=CARTESIAN_POINT('',(184.115917770962,326.027992730186,-379.220287242317));
#54014=CARTESIAN_POINT('Origin',(180.115917770962,294.027992730186,-379.220287242271));
#54015=CARTESIAN_POINT('',(180.115917770964,290.027992731144,281.279712757735));
#54016=CARTESIAN_POINT('Origin',(180.115917770964,294.027992731144,281.279712757729));
#54017=CARTESIAN_POINT('',(180.115917770962,290.027992730186,-379.220287242265));
#54018=CARTESIAN_POINT('',(180.115917770962,290.027992730186,-379.220287242265));
#54019=CARTESIAN_POINT('Origin',(180.115917770962,294.027992730186,-379.220287242271));
#54020=CARTESIAN_POINT('Origin',(180.115917770962,290.027992730186,-379.220287242265));
#54021=CARTESIAN_POINT('',(148.115917770964,290.027992731145,281.279712757735));
#54022=CARTESIAN_POINT('',(172.115917770964,290.027992731144,281.279712757735));
#54023=CARTESIAN_POINT('',(148.115917770962,290.027992730186,-379.220287242265));
#54024=CARTESIAN_POINT('',(148.115917770962,290.027992730186,-379.220287242265));
#54025=CARTESIAN_POINT('',(172.115917770962,290.027992730186,-379.220287242265));
#54026=CARTESIAN_POINT('Origin',(148.115917770962,294.027992730186,-379.220287242271));
#54027=CARTESIAN_POINT('',(144.115917770964,294.027992731144,281.279712757729));
#54028=CARTESIAN_POINT('Origin',(148.115917770964,294.027992731144,281.279712757729));
#54029=CARTESIAN_POINT('',(144.115917770962,294.027992730186,-379.220287242271));
#54030=CARTESIAN_POINT('',(144.115917770962,294.027992730186,-379.220287242271));
#54031=CARTESIAN_POINT('Origin',(148.115917770962,294.027992730186,-379.220287242271));
#54032=CARTESIAN_POINT('Origin',(148.115917770962,328.027992730186,-379.22028724232));
#54033=CARTESIAN_POINT('',(148.115917770964,328.027992731145,281.27971275768));
#54034=CARTESIAN_POINT('',(156.115917770964,328.027992731145,281.27971275768));
#54035=CARTESIAN_POINT('',(148.115917770962,328.027992730186,-379.22028724232));
#54036=CARTESIAN_POINT('',(148.115917770962,328.027992730186,-379.22028724232));
#54037=CARTESIAN_POINT('',(156.115917770962,328.027992730186,-379.22028724232));
#54038=CARTESIAN_POINT('Origin',(148.115917770962,294.027992730186,-379.220287242271));
#54039=CARTESIAN_POINT('',(146.115917770964,294.027992731144,281.279712757729));
#54040=CARTESIAN_POINT('Origin',(148.115917770964,294.027992731144,281.279712757729));
#54041=CARTESIAN_POINT('',(146.115917770962,294.027992730186,-379.220287242271));
#54042=CARTESIAN_POINT('Origin',(148.115917770962,294.027992730186,-379.220287242271));
#54043=CARTESIAN_POINT('',(146.115917770962,294.027992730186,-379.220287242271));
#54044=CARTESIAN_POINT('Origin',(146.115917770962,294.027992730186,-379.220287242271));
#54045=CARTESIAN_POINT('',(146.115917770964,326.027992731144,281.279712757683));
#54046=CARTESIAN_POINT('',(146.115917770964,302.027992731145,281.279712757718));
#54047=CARTESIAN_POINT('',(146.115917770962,326.027992730186,-379.220287242317));
#54048=CARTESIAN_POINT('',(146.115917770962,302.027992730186,-379.220287242282));
#54049=CARTESIAN_POINT('',(146.115917770962,326.027992730186,-379.220287242317));
#54050=CARTESIAN_POINT('Origin',(148.115917770962,326.027992730186,-379.220287242317));
#54051=CARTESIAN_POINT('Origin',(148.115917770964,326.027992731144,281.279712757683));
#54052=CARTESIAN_POINT('Origin',(148.115917770962,326.027992730186,-379.220287242317));
#54053=CARTESIAN_POINT('Origin',(144.115917770962,294.027992730186,-379.220287242271));
#54054=CARTESIAN_POINT('',(144.115917770964,326.027992731144,281.279712757683));
#54055=CARTESIAN_POINT('',(144.115917770964,302.027992731145,281.279712757718));
#54056=CARTESIAN_POINT('',(144.115917770962,326.027992730186,-379.220287242317));
#54057=CARTESIAN_POINT('',(144.115917770962,326.027992730186,-379.220287242317));
#54058=CARTESIAN_POINT('',(144.115917770962,302.027992730186,-379.220287242282));
#54059=CARTESIAN_POINT('Origin',(148.115917770962,326.027992730186,-379.220287242317));
#54060=CARTESIAN_POINT('',(148.115917770964,330.027992731144,281.279712757677));
#54061=CARTESIAN_POINT('Origin',(148.115917770964,326.027992731144,281.279712757683));
#54062=CARTESIAN_POINT('',(148.115917770962,330.027992730186,-379.220287242323));
#54063=CARTESIAN_POINT('',(148.115917770962,330.027992730186,-379.220287242323));
#54064=CARTESIAN_POINT('Origin',(148.115917770962,326.027992730186,-379.220287242317));
#54065=CARTESIAN_POINT('Origin',(148.115917770962,330.027992730186,-379.220287242323));
#54066=CARTESIAN_POINT('',(180.115917770964,330.027992731144,281.279712757677));
#54067=CARTESIAN_POINT('',(156.115917770964,330.027992731144,281.279712757677));
#54068=CARTESIAN_POINT('',(180.115917770962,330.027992730186,-379.220287242323));
#54069=CARTESIAN_POINT('',(180.115917770962,330.027992730186,-379.220287242323));
#54070=CARTESIAN_POINT('',(156.115917770962,330.027992730186,-379.220287242323));
#54071=CARTESIAN_POINT('Origin',(180.115917770962,326.027992730186,-379.220287242317));
#54072=CARTESIAN_POINT('Origin',(180.115917770964,326.027992731144,281.279712757683));
#54073=CARTESIAN_POINT('Origin',(180.115917770962,326.027992730186,-379.220287242317));
#54074=CARTESIAN_POINT('Origin',(164.115917770962,310.027992730186,-379.220287242294));
#54075=CARTESIAN_POINT('Origin',(164.115917770964,310.027992731145,281.279712757706));
#54076=CARTESIAN_POINT('Origin',(180.115917770961,-307.972007269815,-379.220287241397));
#54077=CARTESIAN_POINT('',(148.115917770963,-307.972007268857,280.779712758603));
#54078=CARTESIAN_POINT('',(180.115917770963,-307.972007268857,280.779712758603));
#54079=CARTESIAN_POINT('',(172.115917770963,-307.972007268857,280.779712758603));
#54080=CARTESIAN_POINT('',(180.115917770961,-307.972007269815,-379.220287241397));
#54081=CARTESIAN_POINT('',(180.115917770961,-307.972007269815,-379.220287241397));
#54082=CARTESIAN_POINT('',(148.115917770961,-307.972007269815,-379.220287241397));
#54083=CARTESIAN_POINT('',(172.115917770961,-307.972007269815,-379.220287241397));
#54084=CARTESIAN_POINT('',(148.115917770961,-307.972007269815,-379.220287241397));
#54085=CARTESIAN_POINT('Origin',(180.115917770961,-305.972007269815,-379.2202872414));
#54086=CARTESIAN_POINT('',(182.115917770963,-305.972007268857,280.7797127586));
#54087=CARTESIAN_POINT('Origin',(180.115917770963,-305.972007268857,280.7797127586));
#54088=CARTESIAN_POINT('',(182.115917770961,-305.972007269815,-379.2202872414));
#54089=CARTESIAN_POINT('',(182.115917770961,-305.972007269815,-379.2202872414));
#54090=CARTESIAN_POINT('Origin',(180.115917770961,-305.972007269815,-379.2202872414));
#54091=CARTESIAN_POINT('Origin',(182.115917770961,-273.972007269815,-379.220287241446));
#54092=CARTESIAN_POINT('',(182.115917770963,-273.972007268857,280.779712758554));
#54093=CARTESIAN_POINT('',(182.115917770963,-281.972007268857,280.779712758565));
#54094=CARTESIAN_POINT('',(182.115917770961,-273.972007269815,-379.220287241446));
#54095=CARTESIAN_POINT('',(182.115917770961,-273.972007269815,-379.220287241446));
#54096=CARTESIAN_POINT('',(182.115917770961,-281.972007269815,-379.220287241435));
#54097=CARTESIAN_POINT('Origin',(180.115917770961,-273.972007269815,-379.220287241446));
#54098=CARTESIAN_POINT('',(180.115917770963,-271.972007268857,280.779712758551));
#54099=CARTESIAN_POINT('Origin',(180.115917770963,-273.972007268857,280.779712758554));
#54100=CARTESIAN_POINT('',(180.115917770961,-271.972007269815,-379.220287241449));
#54101=CARTESIAN_POINT('',(180.115917770961,-271.972007269815,-379.220287241449));
#54102=CARTESIAN_POINT('Origin',(180.115917770961,-273.972007269815,-379.220287241446));
#54103=CARTESIAN_POINT('Origin',(184.115917770961,-273.972007269815,-379.220287241446));
#54104=CARTESIAN_POINT('',(184.115917770963,-273.972007268857,280.779712758554));
#54105=CARTESIAN_POINT('',(184.115917770963,-305.972007268857,280.7797127586));
#54106=CARTESIAN_POINT('',(184.115917770963,-281.972007268857,280.779712758565));
#54107=CARTESIAN_POINT('',(184.115917770961,-305.972007269815,-379.2202872414));
#54108=CARTESIAN_POINT('',(184.115917770961,-305.972007269815,-379.2202872414));
#54109=CARTESIAN_POINT('',(184.115917770961,-273.972007269815,-379.220287241446));
#54110=CARTESIAN_POINT('',(184.115917770961,-281.972007269815,-379.220287241435));
#54111=CARTESIAN_POINT('',(184.115917770961,-273.972007269815,-379.220287241446));
#54112=CARTESIAN_POINT('Origin',(180.115917770961,-305.972007269815,-379.2202872414));
#54113=CARTESIAN_POINT('',(180.115917770963,-309.972007268857,280.779712758606));
#54114=CARTESIAN_POINT('Origin',(180.115917770963,-305.972007268857,280.7797127586));
#54115=CARTESIAN_POINT('',(180.115917770961,-309.972007269815,-379.220287241394));
#54116=CARTESIAN_POINT('',(180.115917770961,-309.972007269815,-379.220287241394));
#54117=CARTESIAN_POINT('Origin',(180.115917770961,-305.972007269815,-379.2202872414));
#54118=CARTESIAN_POINT('Origin',(180.115917770961,-309.972007269815,-379.220287241394));
#54119=CARTESIAN_POINT('',(148.115917770963,-309.972007268857,280.779712758606));
#54120=CARTESIAN_POINT('',(172.115917770963,-309.972007268857,280.779712758606));
#54121=CARTESIAN_POINT('',(148.115917770961,-309.972007269815,-379.220287241394));
#54122=CARTESIAN_POINT('',(148.115917770961,-309.972007269815,-379.220287241394));
#54123=CARTESIAN_POINT('',(172.115917770961,-309.972007269815,-379.220287241394));
#54124=CARTESIAN_POINT('Origin',(148.115917770961,-305.972007269815,-379.2202872414));
#54125=CARTESIAN_POINT('',(144.115917770963,-305.972007268857,280.7797127586));
#54126=CARTESIAN_POINT('Origin',(148.115917770963,-305.972007268857,280.7797127586));
#54127=CARTESIAN_POINT('',(144.115917770961,-305.972007269815,-379.2202872414));
#54128=CARTESIAN_POINT('',(144.115917770961,-305.972007269815,-379.2202872414));
#54129=CARTESIAN_POINT('Origin',(148.115917770961,-305.972007269815,-379.2202872414));
#54130=CARTESIAN_POINT('Origin',(148.115917770961,-271.972007269815,-379.220287241449));
#54131=CARTESIAN_POINT('',(148.115917770963,-271.972007268857,280.779712758551));
#54132=CARTESIAN_POINT('',(156.115917770963,-271.972007268857,280.779712758551));
#54133=CARTESIAN_POINT('',(148.115917770961,-271.972007269815,-379.220287241449));
#54134=CARTESIAN_POINT('',(148.115917770961,-271.972007269815,-379.220287241449));
#54135=CARTESIAN_POINT('',(156.115917770961,-271.972007269815,-379.220287241449));
#54136=CARTESIAN_POINT('Origin',(148.115917770961,-305.972007269815,-379.2202872414));
#54137=CARTESIAN_POINT('',(146.115917770963,-305.972007268857,280.7797127586));
#54138=CARTESIAN_POINT('Origin',(148.115917770963,-305.972007268857,280.7797127586));
#54139=CARTESIAN_POINT('',(146.115917770961,-305.972007269815,-379.2202872414));
#54140=CARTESIAN_POINT('Origin',(148.115917770961,-305.972007269815,-379.2202872414));
#54141=CARTESIAN_POINT('',(146.115917770961,-305.972007269815,-379.2202872414));
#54142=CARTESIAN_POINT('Origin',(146.115917770961,-305.972007269815,-379.2202872414));
#54143=CARTESIAN_POINT('',(146.115917770963,-273.972007268857,280.779712758554));
#54144=CARTESIAN_POINT('',(146.115917770963,-297.972007268857,280.779712758589));
#54145=CARTESIAN_POINT('',(146.115917770961,-273.972007269815,-379.220287241446));
#54146=CARTESIAN_POINT('',(146.115917770961,-297.972007269815,-379.220287241411));
#54147=CARTESIAN_POINT('',(146.115917770961,-273.972007269815,-379.220287241446));
#54148=CARTESIAN_POINT('Origin',(148.115917770961,-273.972007269815,-379.220287241446));
#54149=CARTESIAN_POINT('Origin',(148.115917770963,-273.972007268857,280.779712758554));
#54150=CARTESIAN_POINT('Origin',(148.115917770961,-273.972007269815,-379.220287241446));
#54151=CARTESIAN_POINT('Origin',(144.115917770961,-305.972007269815,-379.2202872414));
#54152=CARTESIAN_POINT('',(144.115917770963,-273.972007268857,280.779712758554));
#54153=CARTESIAN_POINT('',(144.115917770963,-297.972007268857,280.779712758589));
#54154=CARTESIAN_POINT('',(144.115917770961,-273.972007269815,-379.220287241446));
#54155=CARTESIAN_POINT('',(144.115917770961,-273.972007269815,-379.220287241446));
#54156=CARTESIAN_POINT('',(144.115917770961,-297.972007269815,-379.220287241411));
#54157=CARTESIAN_POINT('Origin',(148.115917770961,-273.972007269815,-379.220287241446));
#54158=CARTESIAN_POINT('',(148.115917770963,-269.972007268857,280.779712758548));
#54159=CARTESIAN_POINT('Origin',(148.115917770963,-273.972007268857,280.779712758554));
#54160=CARTESIAN_POINT('',(148.115917770961,-269.972007269815,-379.220287241452));
#54161=CARTESIAN_POINT('',(148.115917770961,-269.972007269815,-379.220287241452));
#54162=CARTESIAN_POINT('Origin',(148.115917770961,-273.972007269815,-379.220287241446));
#54163=CARTESIAN_POINT('Origin',(148.115917770961,-269.972007269815,-379.220287241452));
#54164=CARTESIAN_POINT('',(180.115917770963,-269.972007268857,280.779712758548));
#54165=CARTESIAN_POINT('',(156.115917770963,-269.972007268857,280.779712758548));
#54166=CARTESIAN_POINT('',(180.115917770961,-269.972007269815,-379.220287241452));
#54167=CARTESIAN_POINT('',(180.115917770961,-269.972007269815,-379.220287241452));
#54168=CARTESIAN_POINT('',(156.115917770961,-269.972007269815,-379.220287241452));
#54169=CARTESIAN_POINT('Origin',(180.115917770961,-273.972007269815,-379.220287241446));
#54170=CARTESIAN_POINT('Origin',(180.115917770963,-273.972007268857,280.779712758554));
#54171=CARTESIAN_POINT('Origin',(180.115917770961,-273.972007269815,-379.220287241446));
#54172=CARTESIAN_POINT('Origin',(164.115917770961,-289.972007269815,-379.220287241423));
#54173=CARTESIAN_POINT('Origin',(164.115917770963,-289.972007268857,280.779712758577));
#54174=CARTESIAN_POINT('Origin',(154.115917770964,-299.972007268829,300.779712758592));
#54175=CARTESIAN_POINT('',(180.115917770964,-273.9720072688,320.779712758554));
#54176=CARTESIAN_POINT('',(184.115917770964,-269.972007268806,316.779712758548));
#54177=CARTESIAN_POINT('Origin',(180.115917770964,-273.972007268806,316.779712758554));
#54178=CARTESIAN_POINT('',(148.115917770964,-305.9720072688,320.7797127586));
#54179=CARTESIAN_POINT('',(158.115917770964,-295.9720072688,320.779712758586));
#54180=CARTESIAN_POINT('',(144.115917770964,-309.972007268806,316.779712758606));
#54181=CARTESIAN_POINT('Origin',(148.115917770964,-305.972007268806,316.7797127586));
#54182=CARTESIAN_POINT('',(144.115917770964,-309.972007268852,284.779712758606));
#54183=CARTESIAN_POINT('',(144.115917770964,-309.972007268817,308.779712758606));
#54184=CARTESIAN_POINT('',(148.115917770964,-305.972007268858,280.7797127586));
#54185=CARTESIAN_POINT('Origin',(148.115917770964,-305.972007268852,284.7797127586));
#54186=CARTESIAN_POINT('',(180.115917770964,-273.972007268858,280.779712758554));
#54187=CARTESIAN_POINT('',(150.115917770964,-303.972007268858,280.779712758597));
#54188=CARTESIAN_POINT('',(184.115917770964,-269.972007268852,284.779712758548));
#54189=CARTESIAN_POINT('Origin',(180.115917770964,-273.972007268852,284.779712758554));
#54190=CARTESIAN_POINT('',(184.115917770964,-269.972007268841,292.779712758548));
#54191=CARTESIAN_POINT('',(180.115917770964,-273.972007268803,318.779712758554));
#54192=CARTESIAN_POINT('',(148.115917770964,-305.972007268803,318.7797127586));
#54193=CARTESIAN_POINT('',(158.115917770964,-295.972007268803,318.779712758586));
#54194=CARTESIAN_POINT('',(182.115917770964,-271.972007268806,316.779712758551));
#54195=CARTESIAN_POINT('Origin',(180.115917770964,-273.972007268806,316.779712758554));
#54196=CARTESIAN_POINT('',(182.115917770964,-271.972007268852,284.779712758551));
#54197=CARTESIAN_POINT('',(182.115917770964,-271.972007268841,292.779712758551));
#54198=CARTESIAN_POINT('',(180.115917770964,-273.972007268855,282.779712758554));
#54199=CARTESIAN_POINT('Origin',(180.115917770964,-273.972007268852,284.779712758554));
#54200=CARTESIAN_POINT('',(148.115917770964,-305.972007268855,282.7797127586));
#54201=CARTESIAN_POINT('',(150.115917770964,-303.972007268855,282.779712758597));
#54202=CARTESIAN_POINT('',(146.115917770964,-307.972007268852,284.779712758603));
#54203=CARTESIAN_POINT('Origin',(148.115917770964,-305.972007268852,284.7797127586));
#54204=CARTESIAN_POINT('',(146.115917770964,-307.972007268806,316.779712758603));
#54205=CARTESIAN_POINT('',(146.115917770964,-307.972007268817,308.779712758603));
#54206=CARTESIAN_POINT('Origin',(148.115917770964,-305.972007268806,316.7797127586));
#54207=CARTESIAN_POINT('Origin',(148.115917770964,-309.972007268855,282.779712758606));
#54208=CARTESIAN_POINT('',(180.115917770964,294.527992731153,282.779712757729));
#54209=CARTESIAN_POINT('',(180.115917770964,-309.972007268855,282.779712758606));
#54210=CARTESIAN_POINT('',(148.115917770964,326.527992731175,282.779712757682));
#54211=CARTESIAN_POINT('',(470.365917770976,4.27799273094074,282.779712758149));
#54212=CARTESIAN_POINT('',(148.115917770964,-309.972007268855,282.779712758606));
#54213=CARTESIAN_POINT('Origin',(180.115917770964,-309.972007268852,284.779712758606));
#54214=CARTESIAN_POINT('',(182.115917770964,292.527992731154,284.779712757732));
#54215=CARTESIAN_POINT('',(182.115917770964,-309.972007268852,284.779712758606));
#54216=CARTESIAN_POINT('Origin',(180.115917770964,294.527992731156,284.779712757729));
#54217=CARTESIAN_POINT('Origin',(182.115917770964,-309.972007268852,284.779712758606));
#54218=CARTESIAN_POINT('',(182.115917770964,292.5279927312,316.779712757732));
#54219=CARTESIAN_POINT('',(182.115917770964,-309.972007268806,316.779712758606));
#54220=CARTESIAN_POINT('',(182.115917770964,292.527992731166,292.779712757732));
#54221=CARTESIAN_POINT('Origin',(180.115917770964,-309.972007268806,316.779712758606));
#54222=CARTESIAN_POINT('',(180.115917770964,294.527992731205,318.779712757729));
#54223=CARTESIAN_POINT('',(180.115917770964,-309.972007268803,318.779712758606));
#54224=CARTESIAN_POINT('Origin',(180.115917770964,294.527992731202,316.779712757729));
#54225=CARTESIAN_POINT('Origin',(148.115917770964,-309.972007268852,284.779712758606));
#54226=CARTESIAN_POINT('',(144.115917770964,330.527992731148,284.779712757677));
#54227=CARTESIAN_POINT('',(144.115917770964,-309.972007268852,284.779712758606));
#54228=CARTESIAN_POINT('',(148.115917770964,326.527992731172,280.779712757682));
#54229=CARTESIAN_POINT('Origin',(148.115917770964,326.527992731178,284.779712757682));
#54230=CARTESIAN_POINT('',(148.115917770964,-309.972007268858,280.779712758606));
#54231=CARTESIAN_POINT('Origin',(148.115917770964,-309.972007268806,316.779712758606));
#54232=CARTESIAN_POINT('',(148.115917770964,326.52799273123,320.779712757682));
#54233=CARTESIAN_POINT('',(148.115917770964,-309.9720072688,320.779712758606));
#54234=CARTESIAN_POINT('',(144.115917770964,330.527992731194,316.779712757677));
#54235=CARTESIAN_POINT('Origin',(148.115917770964,326.527992731224,316.779712757682));
#54236=CARTESIAN_POINT('',(144.115917770964,-309.972007268806,316.779712758606));
#54237=CARTESIAN_POINT('Origin',(180.115917770964,-309.9720072688,320.779712758606));
#54238=CARTESIAN_POINT('',(180.115917770964,294.527992731208,320.779712757729));
#54239=CARTESIAN_POINT('',(180.115917770964,-309.9720072688,320.779712758606));
#54240=CARTESIAN_POINT('',(478.365917770971,-3.7220072690041,320.77971275816));
#54241=CARTESIAN_POINT('Origin',(474.365917770973,0.277992730966865,300.779712758155));
#54242=CARTESIAN_POINT('',(144.115917770964,330.527992731183,308.779712757677));
#54243=CARTESIAN_POINT('',(184.115917770964,290.527992731199,316.779712757735));
#54244=CARTESIAN_POINT('Origin',(180.115917770964,294.527992731202,316.779712757729));
#54245=CARTESIAN_POINT('',(184.115917770964,290.527992731153,284.779712757735));
#54246=CARTESIAN_POINT('',(184.115917770964,290.527992731164,292.779712757735));
#54247=CARTESIAN_POINT('',(180.115917770964,294.52799273115,280.779712757729));
#54248=CARTESIAN_POINT('Origin',(180.115917770964,294.527992731156,284.779712757729));
#54249=CARTESIAN_POINT('',(470.365917770976,4.27799273093786,280.779712758149));
#54250=CARTESIAN_POINT('',(148.115917770964,326.527992731227,318.779712757682));
#54251=CARTESIAN_POINT('',(478.365917770971,-3.72200726900701,318.779712758161));
#54252=CARTESIAN_POINT('',(146.115917770964,328.527992731225,316.77971275768));
#54253=CARTESIAN_POINT('Origin',(148.115917770964,326.527992731224,316.779712757682));
#54254=CARTESIAN_POINT('',(146.115917770964,328.527992731179,284.77971275768));
#54255=CARTESIAN_POINT('',(146.115917770964,328.527992731214,308.77971275768));
#54256=CARTESIAN_POINT('Origin',(148.115917770964,326.527992731178,284.779712757682));
#54257=CARTESIAN_POINT('Origin',(180.115917770964,-309.972007268803,318.779712758606));
#54258=CARTESIAN_POINT('',(148.115917770964,-309.972007268803,318.779712758606));
#54259=CARTESIAN_POINT('Origin',(180.115917770964,-309.972007268806,316.779712758606));
#54260=CARTESIAN_POINT('',(184.115917770964,-309.972007268806,316.779712758606));
#54261=CARTESIAN_POINT('Origin',(148.115917770964,-309.972007268852,284.779712758606));
#54262=CARTESIAN_POINT('',(146.115917770964,-309.972007268852,284.779712758606));
#54263=CARTESIAN_POINT('Origin',(146.115917770964,-309.972007268806,316.779712758606));
#54264=CARTESIAN_POINT('',(146.115917770964,-309.972007268806,316.779712758606));
#54265=CARTESIAN_POINT('Origin',(148.115917770964,-309.972007268806,316.779712758606));
#54266=CARTESIAN_POINT('Origin',(144.115917770964,-309.972007268806,316.779712758606));
#54267=CARTESIAN_POINT('Origin',(148.115917770964,-309.972007268858,280.779712758606));
#54268=CARTESIAN_POINT('',(180.115917770964,-309.972007268858,280.779712758606));
#54269=CARTESIAN_POINT('Origin',(180.115917770964,-309.972007268852,284.779712758606));
#54270=CARTESIAN_POINT('',(184.115917770964,-309.972007268852,284.779712758606));
#54271=CARTESIAN_POINT('Origin',(184.115917770964,-309.972007268852,284.779712758606));
#54272=CARTESIAN_POINT('Origin',(483.61591777097,-299.972007268829,300.779712758591));
#54273=CARTESIAN_POINT('',(489.61591777097,-305.9720072688,320.779712758599));
#54274=CARTESIAN_POINT('',(493.61591777097,-309.972007268806,316.779712758605));
#54275=CARTESIAN_POINT('Origin',(489.61591777097,-305.972007268806,316.779712758599));
#54276=CARTESIAN_POINT('',(457.61591777097,-273.9720072688,320.779712758553));
#54277=CARTESIAN_POINT('',(487.61591777097,-303.9720072688,320.779712758596));
#54278=CARTESIAN_POINT('',(453.61591777097,-269.972007268806,316.779712758547));
#54279=CARTESIAN_POINT('Origin',(457.61591777097,-273.972007268806,316.779712758553));
#54280=CARTESIAN_POINT('',(453.61591777097,-269.972007268852,284.779712758547));
#54281=CARTESIAN_POINT('',(453.61591777097,-269.972007268817,308.779712758547));
#54282=CARTESIAN_POINT('',(457.61591777097,-273.972007268858,280.779712758553));
#54283=CARTESIAN_POINT('Origin',(457.61591777097,-273.972007268852,284.779712758553));
#54284=CARTESIAN_POINT('',(489.61591777097,-305.972007268858,280.779712758599));
#54285=CARTESIAN_POINT('',(479.61591777097,-295.972007268858,280.779712758585));
#54286=CARTESIAN_POINT('',(493.61591777097,-309.972007268852,284.779712758605));
#54287=CARTESIAN_POINT('Origin',(489.61591777097,-305.972007268852,284.779712758599));
#54288=CARTESIAN_POINT('',(493.61591777097,-309.972007268841,292.779712758605));
#54289=CARTESIAN_POINT('',(489.61591777097,-305.972007268803,318.779712758599));
#54290=CARTESIAN_POINT('',(457.61591777097,-273.972007268803,318.779712758553));
#54291=CARTESIAN_POINT('',(487.61591777097,-303.972007268803,318.779712758596));
#54292=CARTESIAN_POINT('',(491.61591777097,-307.972007268806,316.779712758602));
#54293=CARTESIAN_POINT('Origin',(489.61591777097,-305.972007268806,316.779712758599));
#54294=CARTESIAN_POINT('',(491.61591777097,-307.972007268852,284.779712758602));
#54295=CARTESIAN_POINT('',(491.61591777097,-307.972007268841,292.779712758602));
#54296=CARTESIAN_POINT('',(489.61591777097,-305.972007268855,282.779712758599));
#54297=CARTESIAN_POINT('Origin',(489.61591777097,-305.972007268852,284.779712758599));
#54298=CARTESIAN_POINT('',(457.61591777097,-273.972007268855,282.779712758553));
#54299=CARTESIAN_POINT('',(479.61591777097,-295.972007268855,282.779712758585));
#54300=CARTESIAN_POINT('',(455.61591777097,-271.972007268852,284.77971275855));
#54301=CARTESIAN_POINT('Origin',(457.61591777097,-273.972007268852,284.779712758553));
#54302=CARTESIAN_POINT('',(455.61591777097,-271.972007268806,316.77971275855));
#54303=CARTESIAN_POINT('',(455.61591777097,-271.972007268817,308.77971275855));
#54304=CARTESIAN_POINT('Origin',(457.61591777097,-273.972007268806,316.779712758553));
#54305=CARTESIAN_POINT('Origin',(457.61591777097,-309.972007268855,282.779712758605));
#54306=CARTESIAN_POINT('',(489.61591777097,326.527992731175,282.779712757681));
#54307=CARTESIAN_POINT('',(489.61591777097,-309.972007268855,282.779712758605));
#54308=CARTESIAN_POINT('',(457.61591777097,294.527992731153,282.779712757728));
#54309=CARTESIAN_POINT('',(159.365917770963,-3.72200726905991,282.779712758162));
#54310=CARTESIAN_POINT('',(457.61591777097,-309.972007268855,282.779712758605));
#54311=CARTESIAN_POINT('Origin',(489.61591777097,-309.972007268852,284.779712758605));
#54312=CARTESIAN_POINT('',(491.61591777097,328.527992731179,284.779712757678));
#54313=CARTESIAN_POINT('',(491.61591777097,-309.972007268852,284.779712758605));
#54314=CARTESIAN_POINT('Origin',(489.61591777097,326.527992731178,284.779712757681));
#54315=CARTESIAN_POINT('Origin',(491.61591777097,-309.972007268852,284.779712758605));
#54316=CARTESIAN_POINT('',(491.61591777097,328.527992731225,316.779712757678));
#54317=CARTESIAN_POINT('',(491.61591777097,-309.972007268806,316.779712758605));
#54318=CARTESIAN_POINT('',(491.61591777097,328.52799273119,292.779712757678));
#54319=CARTESIAN_POINT('Origin',(489.61591777097,-309.972007268806,316.779712758605));
#54320=CARTESIAN_POINT('',(489.61591777097,326.527992731227,318.779712757681));
#54321=CARTESIAN_POINT('',(489.61591777097,-309.972007268803,318.779712758605));
#54322=CARTESIAN_POINT('Origin',(489.61591777097,326.527992731224,316.779712757681));
#54323=CARTESIAN_POINT('Origin',(457.61591777097,-309.972007268852,284.779712758605));
#54324=CARTESIAN_POINT('',(453.61591777097,290.527992731153,284.779712757734));
#54325=CARTESIAN_POINT('',(453.61591777097,-309.972007268852,284.779712758605));
#54326=CARTESIAN_POINT('',(457.61591777097,294.52799273115,280.779712757728));
#54327=CARTESIAN_POINT('Origin',(457.61591777097,294.527992731156,284.779712757728));
#54328=CARTESIAN_POINT('',(457.61591777097,-309.972007268858,280.779712758605));
#54329=CARTESIAN_POINT('Origin',(453.61591777097,-309.972007268806,316.779712758605));
#54330=CARTESIAN_POINT('',(453.61591777097,290.527992731199,316.779712757734));
#54331=CARTESIAN_POINT('',(453.61591777097,-309.972007268806,316.779712758605));
#54332=CARTESIAN_POINT('',(453.61591777097,290.527992731188,308.779712757734));
#54333=CARTESIAN_POINT('Origin',(457.61591777097,-309.972007268806,316.779712758605));
#54334=CARTESIAN_POINT('',(457.61591777097,294.527992731208,320.779712757728));
#54335=CARTESIAN_POINT('',(457.61591777097,-309.9720072688,320.779712758605));
#54336=CARTESIAN_POINT('Origin',(457.61591777097,294.527992731202,316.779712757728));
#54337=CARTESIAN_POINT('Origin',(489.61591777097,-309.9720072688,320.779712758605));
#54338=CARTESIAN_POINT('',(489.61591777097,326.52799273123,320.779712757681));
#54339=CARTESIAN_POINT('',(489.61591777097,-309.9720072688,320.779712758605));
#54340=CARTESIAN_POINT('',(167.365917770958,4.27799273099524,320.77971275815));
#54341=CARTESIAN_POINT('Origin',(163.365917770961,0.27799273096619,300.779712758156));
#54342=CARTESIAN_POINT('',(493.61591777097,330.527992731194,316.779712757675));
#54343=CARTESIAN_POINT('Origin',(489.61591777097,326.527992731224,316.779712757681));
#54344=CARTESIAN_POINT('',(493.61591777097,330.527992731148,284.779712757675));
#54345=CARTESIAN_POINT('',(493.61591777097,330.527992731159,292.779712757675));
#54346=CARTESIAN_POINT('',(489.61591777097,326.527992731172,280.779712757681));
#54347=CARTESIAN_POINT('Origin',(489.61591777097,326.527992731178,284.779712757681));
#54348=CARTESIAN_POINT('',(159.365917770963,-3.72200726906282,280.779712758162));
#54349=CARTESIAN_POINT('',(457.61591777097,294.527992731205,318.779712757728));
#54350=CARTESIAN_POINT('',(167.365917770958,4.27799273099236,318.77971275815));
#54351=CARTESIAN_POINT('',(455.61591777097,292.5279927312,316.779712757731));
#54352=CARTESIAN_POINT('Origin',(457.61591777097,294.527992731202,316.779712757728));
#54353=CARTESIAN_POINT('',(455.61591777097,292.527992731154,284.779712757731));
#54354=CARTESIAN_POINT('',(455.61591777097,292.527992731189,308.779712757731));
#54355=CARTESIAN_POINT('Origin',(457.61591777097,294.527992731156,284.779712757728));
#54356=CARTESIAN_POINT('Origin',(489.61591777097,-309.972007268803,318.779712758605));
#54357=CARTESIAN_POINT('',(457.61591777097,-309.972007268803,318.779712758605));
#54358=CARTESIAN_POINT('Origin',(489.61591777097,-309.972007268806,316.779712758605));
#54359=CARTESIAN_POINT('',(493.61591777097,-309.972007268806,316.779712758605));
#54360=CARTESIAN_POINT('Origin',(457.61591777097,-309.972007268852,284.779712758605));
#54361=CARTESIAN_POINT('',(455.61591777097,-309.972007268852,284.779712758605));
#54362=CARTESIAN_POINT('Origin',(455.61591777097,-309.972007268806,316.779712758605));
#54363=CARTESIAN_POINT('',(455.61591777097,-309.972007268806,316.779712758605));
#54364=CARTESIAN_POINT('Origin',(457.61591777097,-309.972007268806,316.779712758605));
#54365=CARTESIAN_POINT('Origin',(457.61591777097,-309.972007268858,280.779712758605));
#54366=CARTESIAN_POINT('',(489.61591777097,-309.972007268858,280.779712758605));
#54367=CARTESIAN_POINT('Origin',(489.61591777097,-309.972007268852,284.779712758605));
#54368=CARTESIAN_POINT('',(493.61591777097,-309.972007268852,284.779712758605));
#54369=CARTESIAN_POINT('Origin',(493.61591777097,-309.972007268852,284.779712758605));
#54370=CARTESIAN_POINT('Origin',(309.115917771081,146.027992731188,301.279712757927));
#54371=CARTESIAN_POINT('',(457.615917770964,294.527992731203,321.279712757697));
#54372=CARTESIAN_POINT('',(489.615917770942,326.527992731203,321.279712757678));
#54373=CARTESIAN_POINT('',(305.115917771072,142.027992731206,321.279712757788));
#54374=CARTESIAN_POINT('',(453.61591777097,290.5279927312,317.2797127577));
#54375=CARTESIAN_POINT('Origin',(457.615917770968,294.5279927312,317.279712757697));
#54376=CARTESIAN_POINT('',(453.615917770998,290.527992731181,285.2797127577));
#54377=CARTESIAN_POINT('',(453.615917770991,290.527992731186,293.279712757966));
#54378=CARTESIAN_POINT('',(457.615917770999,294.527992731179,281.279712757697));
#54379=CARTESIAN_POINT('Origin',(457.615917770995,294.527992731181,285.279712757697));
#54380=CARTESIAN_POINT('',(489.615917770977,326.527992731179,281.279712757678));
#54381=CARTESIAN_POINT('',(313.115917771089,150.02799273117,281.279712757783));
#54382=CARTESIAN_POINT('',(493.615917770964,330.527992731181,285.279712757676));
#54383=CARTESIAN_POINT('Origin',(489.615917770973,326.527992731181,285.279712757678));
#54384=CARTESIAN_POINT('',(493.615917770964,330.5279927312,317.279712757676));
#54385=CARTESIAN_POINT('',(493.615917770964,330.527992731196,309.279712757676));
#54386=CARTESIAN_POINT('Origin',(489.615917770946,326.5279927312,317.279712757678));
#54387=CARTESIAN_POINT('',(491.615917770972,328.527992731181,285.279712757677));
#54388=CARTESIAN_POINT('',(491.615917770944,328.5279927312,317.279712757677));
#54389=CARTESIAN_POINT('',(491.615917770951,328.527992731196,309.279712757976));
#54390=CARTESIAN_POINT('',(489.615917770975,326.52799273118,283.279712757678));
#54391=CARTESIAN_POINT('Origin',(489.615917770973,326.527992731181,285.279712757678));
#54392=CARTESIAN_POINT('',(457.615917770997,294.52799273118,283.279712757697));
#54393=CARTESIAN_POINT('',(313.115917771089,150.027992731172,283.279712757783));
#54394=CARTESIAN_POINT('',(455.615917770997,292.527992731181,285.279712757699));
#54395=CARTESIAN_POINT('Origin',(457.615917770995,294.527992731181,285.279712757697));
#54396=CARTESIAN_POINT('',(455.615917770969,292.5279927312,317.279712757699));
#54397=CARTESIAN_POINT('',(455.61591777099,292.527992731186,293.279712757967));
#54398=CARTESIAN_POINT('',(457.615917770966,294.527992731201,319.279712757697));
#54399=CARTESIAN_POINT('Origin',(457.615917770968,294.5279927312,317.279712757697));
#54400=CARTESIAN_POINT('',(489.615917770944,326.527992731201,319.279712757678));
#54401=CARTESIAN_POINT('',(305.115917771073,142.027992731204,319.279712757788));
#54402=CARTESIAN_POINT('Origin',(489.615917770946,326.5279927312,317.279712757678));
#54403=CARTESIAN_POINT('Origin',(144.615917770964,292.527992731182,285.2797127577));
#54404=CARTESIAN_POINT('',(182.115917770938,292.527992731182,285.279712757699));
#54405=CARTESIAN_POINT('',(144.615917770964,292.527992731182,285.2797127577));
#54406=CARTESIAN_POINT('',(182.115917770965,292.5279927312,317.2797127577));
#54407=CARTESIAN_POINT('',(182.115917770945,292.527992731186,293.279712757667));
#54408=CARTESIAN_POINT('',(144.615917770964,292.5279927312,317.2797127577));
#54409=CARTESIAN_POINT('Origin',(144.615917770964,294.527992731182,285.279712757698));
#54410=CARTESIAN_POINT('',(180.115917770937,294.52799273118,283.279712757698));
#54411=CARTESIAN_POINT('',(144.615917770964,294.52799273118,283.279712757698));
#54412=CARTESIAN_POINT('Origin',(180.115917770939,294.527992731182,285.279712757698));
#54413=CARTESIAN_POINT('Origin',(144.615917770964,326.52799273118,283.27971275768));
#54414=CARTESIAN_POINT('',(148.115917770959,326.52799273118,283.27971275768));
#54415=CARTESIAN_POINT('',(144.615917770964,326.52799273118,283.27971275768));
#54416=CARTESIAN_POINT('',(150.365917770963,324.277992731175,283.279712757681));
#54417=CARTESIAN_POINT('Origin',(144.615917770964,326.527992731182,285.27971275768));
#54418=CARTESIAN_POINT('',(146.115917770963,328.527992731182,285.279712757678));
#54419=CARTESIAN_POINT('',(144.615917770964,328.527992731182,285.279712757678));
#54420=CARTESIAN_POINT('Origin',(148.115917770961,326.527992731182,285.27971275768));
#54421=CARTESIAN_POINT('Origin',(144.615917770964,326.527992731179,281.27971275768));
#54422=CARTESIAN_POINT('',(180.115917770936,294.527992731179,281.279712757698));
#54423=CARTESIAN_POINT('',(144.615917770964,294.527992731179,281.279712757698));
#54424=CARTESIAN_POINT('',(148.115917770958,326.527992731179,281.27971275768));
#54425=CARTESIAN_POINT('',(150.365917770962,324.277992731173,281.279712757681));
#54426=CARTESIAN_POINT('',(144.615917770964,326.527992731179,281.27971275768));
#54427=CARTESIAN_POINT('Origin',(144.615917770964,294.527992731182,285.279712757698));
#54428=CARTESIAN_POINT('',(184.115917770936,290.527992731182,285.279712757701));
#54429=CARTESIAN_POINT('',(144.615917770964,290.527992731182,285.279712757701));
#54430=CARTESIAN_POINT('Origin',(180.115917770939,294.527992731182,285.279712757698));
#54431=CARTESIAN_POINT('Origin',(144.615917770964,290.527992731182,285.279712757701));
#54432=CARTESIAN_POINT('',(184.115917770964,290.5279927312,317.279712757701));
#54433=CARTESIAN_POINT('',(144.615917770964,290.5279927312,317.279712757701));
#54434=CARTESIAN_POINT('',(184.115917770943,290.527992731186,293.279712757667));
#54435=CARTESIAN_POINT('Origin',(144.615917770964,294.5279927312,317.279712757698));
#54436=CARTESIAN_POINT('',(180.11591777097,294.527992731203,321.279712757698));
#54437=CARTESIAN_POINT('',(144.615917770964,294.527992731203,321.279712757698));
#54438=CARTESIAN_POINT('Origin',(180.115917770967,294.5279927312,317.279712757698));
#54439=CARTESIAN_POINT('Origin',(154.365917770971,320.277992731191,301.279712757675));
#54440=CARTESIAN_POINT('',(148.115917770992,326.527992731203,321.27971275768));
#54441=CARTESIAN_POINT('',(158.365917770979,316.277992731209,321.279712757686));
#54442=CARTESIAN_POINT('',(144.115917770964,330.5279927312,317.279712757677));
#54443=CARTESIAN_POINT('Origin',(148.115917770989,326.5279927312,317.27971275768));
#54444=CARTESIAN_POINT('',(144.115917770964,330.527992731182,285.279712757677));
#54445=CARTESIAN_POINT('',(144.115917770964,330.527992731196,309.279712757677));
#54446=CARTESIAN_POINT('Origin',(148.115917770961,326.527992731182,285.27971275768));
#54447=CARTESIAN_POINT('',(146.11591777099,328.5279927312,317.279712757678));
#54448=CARTESIAN_POINT('',(146.115917770983,328.527992731196,309.279712757677));
#54449=CARTESIAN_POINT('',(148.115917770991,326.527992731202,319.27971275768));
#54450=CARTESIAN_POINT('Origin',(148.115917770989,326.5279927312,317.27971275768));
#54451=CARTESIAN_POINT('',(180.115917770969,294.527992731202,319.279712757698));
#54452=CARTESIAN_POINT('',(158.365917770979,316.277992731207,319.279712757686));
#54453=CARTESIAN_POINT('Origin',(180.115917770967,294.5279927312,317.279712757698));
#54454=CARTESIAN_POINT('Origin',(144.615917770964,328.5279927312,317.279712757678));
#54455=CARTESIAN_POINT('',(144.615917770964,328.5279927312,317.279712757678));
#54456=CARTESIAN_POINT('Origin',(144.615917770964,294.527992731203,321.279712757698));
#54457=CARTESIAN_POINT('',(144.615917770964,326.527992731203,321.27971275768));
#54458=CARTESIAN_POINT('Origin',(144.615917770964,294.5279927312,317.279712757698));
#54459=CARTESIAN_POINT('',(144.615917770964,294.527992731202,319.279712757698));
#54460=CARTESIAN_POINT('Origin',(144.615917770964,294.527992731202,319.279712757698));
#54461=CARTESIAN_POINT('',(144.615917770964,326.527992731202,319.27971275768));
#54462=CARTESIAN_POINT('Origin',(144.615917770964,326.5279927312,317.27971275768));
#54463=CARTESIAN_POINT('Origin',(144.615917770964,326.5279927312,317.27971275768));
#54464=CARTESIAN_POINT('',(144.615917770964,330.5279927312,317.279712757677));
#54465=CARTESIAN_POINT('Origin',(144.615917770964,330.5279927312,317.279712757677));
#54466=CARTESIAN_POINT('',(144.615917770964,330.527992731182,285.279712757677));
#54467=CARTESIAN_POINT('Origin',(144.615917770964,326.527992731182,285.27971275768));
#54468=CARTESIAN_POINT('Origin',(483.61591777097,-299.972007268829,300.779712758591));
#54469=CARTESIAN_POINT('',(457.61591777097,-273.972007268858,280.779712758553));
#54470=CARTESIAN_POINT('',(489.61591777097,-305.972007268858,280.779712758599));
#54471=CARTESIAN_POINT('',(487.61591777097,-303.972007268858,280.779712758596));
#54472=CARTESIAN_POINT('',(453.61591777097,-269.972007268852,284.779712758547));
#54473=CARTESIAN_POINT('Origin',(457.61591777097,-273.972007268852,284.779712758553));
#54474=CARTESIAN_POINT('',(453.61591777097,-269.972007268806,316.779712758547));
#54475=CARTESIAN_POINT('',(453.61591777097,-269.972007268841,292.779712758547));
#54476=CARTESIAN_POINT('',(457.61591777097,-273.9720072688,320.779712758553));
#54477=CARTESIAN_POINT('Origin',(457.61591777097,-273.972007268806,316.779712758553));
#54478=CARTESIAN_POINT('',(489.61591777097,-305.9720072688,320.779712758599));
#54479=CARTESIAN_POINT('',(479.61591777097,-295.9720072688,320.779712758585));
#54480=CARTESIAN_POINT('',(493.61591777097,-309.972007268806,316.779712758605));
#54481=CARTESIAN_POINT('Origin',(489.61591777097,-305.972007268806,316.779712758599));
#54482=CARTESIAN_POINT('',(493.61591777097,-309.972007268852,284.779712758605));
#54483=CARTESIAN_POINT('',(493.61591777097,-309.972007268817,308.779712758605));
#54484=CARTESIAN_POINT('Origin',(489.61591777097,-305.972007268852,284.779712758599));
#54485=CARTESIAN_POINT('',(455.61591777097,-271.972007268852,284.77971275855));
#54486=CARTESIAN_POINT('',(455.61591777097,-271.972007268806,316.77971275855));
#54487=CARTESIAN_POINT('',(455.61591777097,-271.972007268841,292.77971275855));
#54488=CARTESIAN_POINT('',(457.61591777097,-273.972007268855,282.779712758553));
#54489=CARTESIAN_POINT('Origin',(457.61591777097,-273.972007268852,284.779712758553));
#54490=CARTESIAN_POINT('',(489.61591777097,-305.972007268855,282.779712758599));
#54491=CARTESIAN_POINT('',(487.61591777097,-303.972007268855,282.779712758596));
#54492=CARTESIAN_POINT('',(491.61591777097,-307.972007268852,284.779712758602));
#54493=CARTESIAN_POINT('Origin',(489.61591777097,-305.972007268852,284.779712758599));
#54494=CARTESIAN_POINT('',(491.61591777097,-307.972007268806,316.779712758602));
#54495=CARTESIAN_POINT('',(491.61591777097,-307.972007268817,308.779712758602));
#54496=CARTESIAN_POINT('',(489.61591777097,-305.972007268803,318.779712758599));
#54497=CARTESIAN_POINT('Origin',(489.61591777097,-305.972007268806,316.779712758599));
#54498=CARTESIAN_POINT('',(457.61591777097,-273.972007268803,318.779712758553));
#54499=CARTESIAN_POINT('',(479.61591777097,-295.972007268803,318.779712758585));
#54500=CARTESIAN_POINT('Origin',(457.61591777097,-273.972007268806,316.779712758553));
#54501=CARTESIAN_POINT('Origin',(493.61591777097,-307.972007268806,316.779712758602));
#54502=CARTESIAN_POINT('',(146.115917770963,-307.972007268852,284.779712758603));
#54503=CARTESIAN_POINT('',(493.61591777097,-307.972007268852,284.779712758602));
#54504=CARTESIAN_POINT('',(146.115917770963,-307.972007268806,316.779712758603));
#54505=CARTESIAN_POINT('',(146.115917770963,-307.972007268817,308.779712758603));
#54506=CARTESIAN_POINT('',(493.61591777097,-307.972007268806,316.779712758602));
#54507=CARTESIAN_POINT('Origin',(493.61591777097,-305.972007268852,284.779712758599));
#54508=CARTESIAN_POINT('',(148.115917770964,-305.972007268855,282.7797127586));
#54509=CARTESIAN_POINT('',(493.61591777097,-305.972007268855,282.779712758599));
#54510=CARTESIAN_POINT('Origin',(148.115917770964,-305.972007268852,284.7797127586));
#54511=CARTESIAN_POINT('Origin',(493.61591777097,-305.972007268855,282.779712758599));
#54512=CARTESIAN_POINT('',(180.115917770963,-273.972007268855,282.779712758554));
#54513=CARTESIAN_POINT('',(493.61591777097,-273.972007268855,282.779712758553));
#54514=CARTESIAN_POINT('',(324.865917770967,-129.222007268852,282.779712758343));
#54515=CARTESIAN_POINT('Origin',(493.61591777097,-273.972007268852,284.779712758553));
#54516=CARTESIAN_POINT('',(182.115917770964,-271.972007268852,284.779712758551));
#54517=CARTESIAN_POINT('',(493.61591777097,-271.972007268852,284.77971275855));
#54518=CARTESIAN_POINT('Origin',(180.115917770963,-273.972007268852,284.779712758554));
#54519=CARTESIAN_POINT('Origin',(493.61591777097,-273.9720072688,320.779712758553));
#54520=CARTESIAN_POINT('',(180.115917770964,-273.9720072688,320.779712758554));
#54521=CARTESIAN_POINT('',(493.61591777097,-273.9720072688,320.779712758553));
#54522=CARTESIAN_POINT('',(148.115917770964,-305.9720072688,320.7797127586));
#54523=CARTESIAN_POINT('',(332.865917770967,-121.222007268797,320.779712758332));
#54524=CARTESIAN_POINT('',(493.61591777097,-305.9720072688,320.779712758599));
#54525=CARTESIAN_POINT('Origin',(493.61591777097,-273.972007268806,316.779712758553));
#54526=CARTESIAN_POINT('',(184.115917770964,-269.972007268806,316.779712758548));
#54527=CARTESIAN_POINT('',(493.61591777097,-269.972007268806,316.779712758547));
#54528=CARTESIAN_POINT('Origin',(180.115917770964,-273.972007268806,316.779712758554));
#54529=CARTESIAN_POINT('Origin',(493.61591777097,-269.972007268852,284.779712758547));
#54530=CARTESIAN_POINT('',(184.115917770964,-269.972007268852,284.779712758548));
#54531=CARTESIAN_POINT('',(493.61591777097,-269.972007268852,284.779712758547));
#54532=CARTESIAN_POINT('',(184.115917770964,-269.97200726884,292.779712758548));
#54533=CARTESIAN_POINT('Origin',(493.61591777097,-273.972007268852,284.779712758553));
#54534=CARTESIAN_POINT('',(180.115917770963,-273.972007268858,280.779712758554));
#54535=CARTESIAN_POINT('',(493.61591777097,-273.972007268858,280.779712758553));
#54536=CARTESIAN_POINT('Origin',(180.115917770963,-273.972007268852,284.779712758554));
#54537=CARTESIAN_POINT('Origin',(328.865917770967,-125.222007268826,300.779712758337));
#54538=CARTESIAN_POINT('',(148.115917770964,-305.972007268858,280.7797127586));
#54539=CARTESIAN_POINT('',(324.865917770967,-129.222007268855,280.779712758343));
#54540=CARTESIAN_POINT('',(144.11591777097,-309.972007268852,284.779712758606));
#54541=CARTESIAN_POINT('Origin',(148.115917770964,-305.972007268852,284.7797127586));
#54542=CARTESIAN_POINT('',(144.11591777097,-309.972007268806,316.779712758606));
#54543=CARTESIAN_POINT('',(144.11591777097,-309.972007268817,308.779712758606));
#54544=CARTESIAN_POINT('Origin',(148.115917770964,-305.972007268806,316.7797127586));
#54545=CARTESIAN_POINT('',(182.115917770964,-271.972007268806,316.779712758551));
#54546=CARTESIAN_POINT('',(182.115917770963,-271.97200726884,292.779712758551));
#54547=CARTESIAN_POINT('',(180.115917770964,-273.972007268803,318.779712758554));
#54548=CARTESIAN_POINT('Origin',(180.115917770964,-273.972007268806,316.779712758554));
#54549=CARTESIAN_POINT('',(148.115917770964,-305.972007268803,318.7797127586));
#54550=CARTESIAN_POINT('',(332.865917770967,-121.2220072688,318.779712758332));
#54551=CARTESIAN_POINT('Origin',(148.115917770964,-305.972007268806,316.7797127586));
#54552=CARTESIAN_POINT('Origin',(493.61591777097,-271.972007268852,284.77971275855));
#54553=CARTESIAN_POINT('',(493.61591777097,-271.972007268806,316.77971275855));
#54554=CARTESIAN_POINT('Origin',(493.61591777097,-305.972007268858,280.779712758599));
#54555=CARTESIAN_POINT('',(493.61591777097,-305.972007268858,280.779712758599));
#54556=CARTESIAN_POINT('Origin',(493.61591777097,-305.972007268806,316.779712758599));
#54557=CARTESIAN_POINT('',(493.61591777097,-305.972007268803,318.779712758599));
#54558=CARTESIAN_POINT('Origin',(493.61591777097,-273.972007268803,318.779712758553));
#54559=CARTESIAN_POINT('',(493.61591777097,-273.972007268803,318.779712758553));
#54560=CARTESIAN_POINT('Origin',(493.61591777097,-273.972007268806,316.779712758553));
#54561=CARTESIAN_POINT('Origin',(493.61591777097,-305.972007268806,316.779712758599));
#54562=CARTESIAN_POINT('',(493.61591777097,-309.972007268806,316.779712758605));
#54563=CARTESIAN_POINT('Origin',(493.61591777097,-309.972007268806,316.779712758605));
#54564=CARTESIAN_POINT('',(493.61591777097,-309.972007268852,284.779712758605));
#54565=CARTESIAN_POINT('Origin',(493.61591777097,-305.972007268852,284.779712758599));
#54566=CARTESIAN_POINT('Origin',(144.115917770962,-307.972007269816,-250.999999448107));
#54567=CARTESIAN_POINT('',(453.615917770962,-307.972007269816,-218.999999448108));
#54568=CARTESIAN_POINT('',(453.615917770962,-307.972007269816,-250.999999448108));
#54569=CARTESIAN_POINT('',(453.615917770962,-307.972007269816,-242.999999448108));
#54570=CARTESIAN_POINT('',(184.115917770962,-307.972007269816,-250.999999448107));
#54571=CARTESIAN_POINT('',(144.115917770962,-307.972007269816,-250.999999448107));
#54572=CARTESIAN_POINT('',(184.115917770962,-307.972007269816,-218.999999448107));
#54573=CARTESIAN_POINT('',(184.115917770962,-307.972007269816,-242.999999448107));
#54574=CARTESIAN_POINT('',(144.115917770962,-307.972007269816,-218.999999448107));
#54575=CARTESIAN_POINT('Origin',(144.115917770962,-305.972007269816,-250.999999448107));
#54576=CARTESIAN_POINT('',(453.615917770962,-305.972007269816,-252.999999448108));
#54577=CARTESIAN_POINT('Origin',(453.615917770962,-305.972007269816,-250.999999448108));
#54578=CARTESIAN_POINT('',(184.115917770962,-305.972007269816,-252.999999448107));
#54579=CARTESIAN_POINT('',(144.115917770962,-305.972007269816,-252.999999448107));
#54580=CARTESIAN_POINT('Origin',(184.115917770962,-305.972007269816,-250.999999448107));
#54581=CARTESIAN_POINT('Origin',(144.115917770962,-273.972007269816,-252.999999448107));
#54582=CARTESIAN_POINT('',(453.615917770962,-273.972007269816,-252.999999448108));
#54583=CARTESIAN_POINT('',(453.615917770962,-281.972007269816,-252.999999448108));
#54584=CARTESIAN_POINT('',(184.115917770962,-273.972007269816,-252.999999448107));
#54585=CARTESIAN_POINT('',(144.115917770962,-273.972007269816,-252.999999448107));
#54586=CARTESIAN_POINT('',(184.115917770962,-281.972007269816,-252.999999448107));
#54587=CARTESIAN_POINT('Origin',(144.115917770962,-273.972007269816,-250.999999448107));
#54588=CARTESIAN_POINT('',(453.615917770962,-271.972007269816,-250.999999448108));
#54589=CARTESIAN_POINT('Origin',(453.615917770962,-273.972007269816,-250.999999448108));
#54590=CARTESIAN_POINT('',(184.115917770962,-271.972007269816,-250.999999448107));
#54591=CARTESIAN_POINT('',(144.115917770962,-271.972007269816,-250.999999448107));
#54592=CARTESIAN_POINT('Origin',(184.115917770962,-273.972007269816,-250.999999448107));
#54593=CARTESIAN_POINT('Origin',(144.115917770962,-273.972007269816,-254.999999448107));
#54594=CARTESIAN_POINT('',(453.615917770962,-273.972007269816,-254.999999448108));
#54595=CARTESIAN_POINT('',(453.615917770962,-305.972007269816,-254.999999448108));
#54596=CARTESIAN_POINT('',(453.615917770962,-281.972007269816,-254.999999448108));
#54597=CARTESIAN_POINT('',(184.115917770962,-305.972007269816,-254.999999448107));
#54598=CARTESIAN_POINT('',(144.115917770962,-305.972007269816,-254.999999448107));
#54599=CARTESIAN_POINT('',(184.115917770962,-273.972007269816,-254.999999448107));
#54600=CARTESIAN_POINT('',(184.115917770962,-281.972007269816,-254.999999448107));
#54601=CARTESIAN_POINT('',(144.115917770962,-273.972007269816,-254.999999448107));
#54602=CARTESIAN_POINT('Origin',(144.115917770962,-305.972007269816,-250.999999448107));
#54603=CARTESIAN_POINT('',(453.615917770962,-309.972007269816,-250.999999448108));
#54604=CARTESIAN_POINT('Origin',(453.615917770962,-305.972007269816,-250.999999448108));
#54605=CARTESIAN_POINT('',(184.115917770962,-309.972007269816,-250.999999448107));
#54606=CARTESIAN_POINT('',(144.115917770962,-309.972007269816,-250.999999448107));
#54607=CARTESIAN_POINT('Origin',(184.115917770962,-305.972007269816,-250.999999448107));
#54608=CARTESIAN_POINT('Origin',(144.115917770962,-309.972007269816,-250.999999448107));
#54609=CARTESIAN_POINT('',(453.615917770962,-309.972007269816,-218.999999448108));
#54610=CARTESIAN_POINT('',(453.615917770962,-309.972007269816,-242.999999448108));
#54611=CARTESIAN_POINT('',(184.115917770962,-309.972007269816,-218.999999448107));
#54612=CARTESIAN_POINT('',(144.115917770962,-309.972007269816,-218.999999448107));
#54613=CARTESIAN_POINT('',(184.115917770962,-309.972007269816,-242.999999448107));
#54614=CARTESIAN_POINT('Origin',(144.115917770962,-305.972007269816,-218.999999448107));
#54615=CARTESIAN_POINT('',(453.615917770962,-305.972007269816,-214.999999448108));
#54616=CARTESIAN_POINT('Origin',(453.615917770962,-305.972007269816,-218.999999448108));
#54617=CARTESIAN_POINT('',(184.115917770962,-305.972007269816,-214.999999448107));
#54618=CARTESIAN_POINT('',(144.115917770962,-305.972007269816,-214.999999448107));
#54619=CARTESIAN_POINT('Origin',(184.115917770962,-305.972007269816,-218.999999448107));
#54620=CARTESIAN_POINT('Origin',(144.115917770962,-271.972007269816,-218.999999448107));
#54621=CARTESIAN_POINT('',(453.615917770962,-271.972007269816,-218.999999448108));
#54622=CARTESIAN_POINT('',(453.615917770962,-271.972007269816,-226.999999448108));
#54623=CARTESIAN_POINT('',(184.115917770962,-271.972007269816,-218.999999448107));
#54624=CARTESIAN_POINT('',(144.115917770962,-271.972007269816,-218.999999448107));
#54625=CARTESIAN_POINT('',(184.115917770962,-271.972007269816,-226.999999448107));
#54626=CARTESIAN_POINT('Origin',(144.115917770962,-305.972007269816,-218.999999448107));
#54627=CARTESIAN_POINT('',(453.615917770962,-305.972007269816,-216.999999448108));
#54628=CARTESIAN_POINT('Origin',(453.615917770962,-305.972007269816,-218.999999448108));
#54629=CARTESIAN_POINT('',(184.115917770962,-305.972007269816,-216.999999448107));
#54630=CARTESIAN_POINT('Origin',(184.115917770962,-305.972007269816,-218.999999448107));
#54631=CARTESIAN_POINT('',(144.115917770962,-305.972007269816,-216.999999448107));
#54632=CARTESIAN_POINT('Origin',(144.115917770962,-305.972007269816,-216.999999448107));
#54633=CARTESIAN_POINT('',(453.615917770962,-273.972007269816,-216.999999448108));
#54634=CARTESIAN_POINT('',(453.615917770962,-297.972007269816,-216.999999448108));
#54635=CARTESIAN_POINT('',(184.115917770962,-273.972007269816,-216.999999448107));
#54636=CARTESIAN_POINT('',(184.115917770962,-297.972007269816,-216.999999448107));
#54637=CARTESIAN_POINT('',(144.115917770962,-273.972007269816,-216.999999448107));
#54638=CARTESIAN_POINT('Origin',(144.115917770962,-273.972007269816,-218.999999448107));
#54639=CARTESIAN_POINT('Origin',(453.615917770962,-273.972007269816,-218.999999448108));
#54640=CARTESIAN_POINT('Origin',(184.115917770962,-273.972007269816,-218.999999448107));
#54641=CARTESIAN_POINT('Origin',(144.115917770962,-305.972007269816,-214.999999448107));
#54642=CARTESIAN_POINT('',(453.615917770962,-273.972007269816,-214.999999448108));
#54643=CARTESIAN_POINT('',(453.615917770962,-297.972007269816,-214.999999448108));
#54644=CARTESIAN_POINT('',(184.115917770962,-273.972007269816,-214.999999448107));
#54645=CARTESIAN_POINT('',(144.115917770962,-273.972007269816,-214.999999448107));
#54646=CARTESIAN_POINT('',(184.115917770962,-297.972007269816,-214.999999448107));
#54647=CARTESIAN_POINT('Origin',(144.115917770962,-273.972007269816,-218.999999448107));
#54648=CARTESIAN_POINT('',(453.615917770962,-269.972007269816,-218.999999448108));
#54649=CARTESIAN_POINT('Origin',(453.615917770962,-273.972007269816,-218.999999448108));
#54650=CARTESIAN_POINT('',(184.115917770962,-269.972007269816,-218.999999448107));
#54651=CARTESIAN_POINT('',(144.115917770962,-269.972007269816,-218.999999448107));
#54652=CARTESIAN_POINT('Origin',(184.115917770962,-273.972007269816,-218.999999448107));
#54653=CARTESIAN_POINT('Origin',(144.115917770962,-269.972007269816,-218.999999448107));
#54654=CARTESIAN_POINT('',(453.615917770962,-269.972007269816,-250.999999448108));
#54655=CARTESIAN_POINT('',(453.615917770962,-269.972007269816,-226.999999448108));
#54656=CARTESIAN_POINT('',(184.115917770962,-269.972007269816,-250.999999448107));
#54657=CARTESIAN_POINT('',(144.115917770962,-269.972007269816,-250.999999448107));
#54658=CARTESIAN_POINT('',(184.115917770962,-269.972007269816,-226.999999448107));
#54659=CARTESIAN_POINT('Origin',(144.115917770962,-273.972007269816,-250.999999448107));
#54660=CARTESIAN_POINT('Origin',(453.615917770962,-273.972007269816,-250.999999448108));
#54661=CARTESIAN_POINT('Origin',(184.115917770962,-273.972007269816,-250.999999448107));
#54662=CARTESIAN_POINT('Origin',(184.115917770962,-289.972007269816,-234.999999448107));
#54663=CARTESIAN_POINT('Origin',(453.615917770962,-289.972007269816,-234.999999448108));
#54664=CARTESIAN_POINT('Origin',(144.115917770962,292.027992730186,-250.999999448106));
#54665=CARTESIAN_POINT('',(453.615917770962,292.027992730186,-218.999999448107));
#54666=CARTESIAN_POINT('',(453.615917770962,292.027992730186,-250.999999448107));
#54667=CARTESIAN_POINT('',(453.615917770962,292.027992730186,-242.999999448107));
#54668=CARTESIAN_POINT('',(184.115917770962,292.027992730186,-250.999999448106));
#54669=CARTESIAN_POINT('',(144.115917770962,292.027992730186,-250.999999448106));
#54670=CARTESIAN_POINT('',(184.115917770962,292.027992730186,-218.999999448106));
#54671=CARTESIAN_POINT('',(184.115917770962,292.027992730186,-242.999999448106));
#54672=CARTESIAN_POINT('',(144.115917770962,292.027992730186,-218.999999448106));
#54673=CARTESIAN_POINT('Origin',(144.115917770962,294.027992730186,-250.999999448106));
#54674=CARTESIAN_POINT('',(453.615917770962,294.027992730186,-252.999999448107));
#54675=CARTESIAN_POINT('Origin',(453.615917770962,294.027992730186,-250.999999448107));
#54676=CARTESIAN_POINT('',(184.115917770962,294.027992730186,-252.999999448106));
#54677=CARTESIAN_POINT('',(144.115917770962,294.027992730186,-252.999999448106));
#54678=CARTESIAN_POINT('Origin',(184.115917770962,294.027992730186,-250.999999448106));
#54679=CARTESIAN_POINT('Origin',(144.115917770962,326.027992730186,-252.999999448106));
#54680=CARTESIAN_POINT('',(453.615917770962,326.027992730186,-252.999999448107));
#54681=CARTESIAN_POINT('',(453.615917770962,318.027992730186,-252.999999448107));
#54682=CARTESIAN_POINT('',(184.115917770962,326.027992730186,-252.999999448106));
#54683=CARTESIAN_POINT('',(144.115917770962,326.027992730186,-252.999999448106));
#54684=CARTESIAN_POINT('',(184.115917770962,318.027992730186,-252.999999448106));
#54685=CARTESIAN_POINT('Origin',(144.115917770962,326.027992730186,-250.999999448106));
#54686=CARTESIAN_POINT('',(453.615917770962,328.027992730186,-250.999999448107));
#54687=CARTESIAN_POINT('Origin',(453.615917770962,326.027992730186,-250.999999448107));
#54688=CARTESIAN_POINT('',(184.115917770962,328.027992730186,-250.999999448106));
#54689=CARTESIAN_POINT('',(144.115917770962,328.027992730186,-250.999999448106));
#54690=CARTESIAN_POINT('Origin',(184.115917770962,326.027992730186,-250.999999448106));
#54691=CARTESIAN_POINT('Origin',(144.115917770962,326.027992730186,-254.999999448106));
#54692=CARTESIAN_POINT('',(453.615917770962,326.027992730186,-254.999999448107));
#54693=CARTESIAN_POINT('',(453.615917770962,294.027992730186,-254.999999448107));
#54694=CARTESIAN_POINT('',(453.615917770962,318.027992730186,-254.999999448107));
#54695=CARTESIAN_POINT('',(184.115917770962,294.027992730186,-254.999999448106));
#54696=CARTESIAN_POINT('',(144.115917770962,294.027992730186,-254.999999448106));
#54697=CARTESIAN_POINT('',(184.115917770962,326.027992730186,-254.999999448106));
#54698=CARTESIAN_POINT('',(184.115917770962,318.027992730186,-254.999999448106));
#54699=CARTESIAN_POINT('',(144.115917770962,326.027992730186,-254.999999448106));
#54700=CARTESIAN_POINT('Origin',(144.115917770962,294.027992730186,-250.999999448106));
#54701=CARTESIAN_POINT('',(453.615917770962,290.027992730186,-250.999999448107));
#54702=CARTESIAN_POINT('Origin',(453.615917770962,294.027992730186,-250.999999448107));
#54703=CARTESIAN_POINT('',(184.115917770962,290.027992730186,-250.999999448106));
#54704=CARTESIAN_POINT('',(144.115917770962,290.027992730186,-250.999999448106));
#54705=CARTESIAN_POINT('Origin',(184.115917770962,294.027992730186,-250.999999448106));
#54706=CARTESIAN_POINT('Origin',(144.115917770962,290.027992730186,-250.999999448106));
#54707=CARTESIAN_POINT('',(453.615917770962,290.027992730186,-218.999999448107));
#54708=CARTESIAN_POINT('',(453.615917770962,290.027992730186,-242.999999448107));
#54709=CARTESIAN_POINT('',(184.115917770962,290.027992730186,-218.999999448106));
#54710=CARTESIAN_POINT('',(144.115917770962,290.027992730186,-218.999999448106));
#54711=CARTESIAN_POINT('',(184.115917770962,290.027992730186,-242.999999448106));
#54712=CARTESIAN_POINT('Origin',(144.115917770962,294.027992730186,-218.999999448106));
#54713=CARTESIAN_POINT('',(453.615917770962,294.027992730186,-214.999999448107));
#54714=CARTESIAN_POINT('Origin',(453.615917770962,294.027992730186,-218.999999448107));
#54715=CARTESIAN_POINT('',(184.115917770962,294.027992730186,-214.999999448106));
#54716=CARTESIAN_POINT('',(144.115917770962,294.027992730186,-214.999999448106));
#54717=CARTESIAN_POINT('Origin',(184.115917770962,294.027992730186,-218.999999448106));
#54718=CARTESIAN_POINT('Origin',(144.115917770962,328.027992730186,-218.999999448106));
#54719=CARTESIAN_POINT('',(453.615917770962,328.027992730186,-218.999999448107));
#54720=CARTESIAN_POINT('',(453.615917770962,328.027992730186,-226.999999448107));
#54721=CARTESIAN_POINT('',(184.115917770962,328.027992730186,-218.999999448106));
#54722=CARTESIAN_POINT('',(144.115917770962,328.027992730186,-218.999999448106));
#54723=CARTESIAN_POINT('',(184.115917770962,328.027992730186,-226.999999448106));
#54724=CARTESIAN_POINT('Origin',(144.115917770962,294.027992730186,-218.999999448106));
#54725=CARTESIAN_POINT('',(453.615917770962,294.027992730186,-216.999999448107));
#54726=CARTESIAN_POINT('Origin',(453.615917770962,294.027992730186,-218.999999448107));
#54727=CARTESIAN_POINT('',(184.115917770962,294.027992730186,-216.999999448106));
#54728=CARTESIAN_POINT('Origin',(184.115917770962,294.027992730186,-218.999999448106));
#54729=CARTESIAN_POINT('',(144.115917770962,294.027992730186,-216.999999448106));
#54730=CARTESIAN_POINT('Origin',(144.115917770962,294.027992730186,-216.999999448106));
#54731=CARTESIAN_POINT('',(453.615917770962,326.027992730186,-216.999999448107));
#54732=CARTESIAN_POINT('',(453.615917770962,302.027992730186,-216.999999448107));
#54733=CARTESIAN_POINT('',(184.115917770962,326.027992730186,-216.999999448106));
#54734=CARTESIAN_POINT('',(184.115917770962,302.027992730186,-216.999999448106));
#54735=CARTESIAN_POINT('',(144.115917770962,326.027992730186,-216.999999448106));
#54736=CARTESIAN_POINT('Origin',(144.115917770962,326.027992730186,-218.999999448106));
#54737=CARTESIAN_POINT('Origin',(453.615917770962,326.027992730186,-218.999999448107));
#54738=CARTESIAN_POINT('Origin',(184.115917770962,326.027992730186,-218.999999448106));
#54739=CARTESIAN_POINT('Origin',(144.115917770962,294.027992730186,-214.999999448106));
#54740=CARTESIAN_POINT('',(453.615917770962,326.027992730186,-214.999999448107));
#54741=CARTESIAN_POINT('',(453.615917770962,302.027992730186,-214.999999448107));
#54742=CARTESIAN_POINT('',(184.115917770962,326.027992730186,-214.999999448106));
#54743=CARTESIAN_POINT('',(144.115917770962,326.027992730186,-214.999999448106));
#54744=CARTESIAN_POINT('',(184.115917770962,302.027992730186,-214.999999448106));
#54745=CARTESIAN_POINT('Origin',(144.115917770962,326.027992730186,-218.999999448106));
#54746=CARTESIAN_POINT('',(453.615917770962,330.027992730186,-218.999999448107));
#54747=CARTESIAN_POINT('Origin',(453.615917770962,326.027992730186,-218.999999448107));
#54748=CARTESIAN_POINT('',(184.115917770962,330.027992730186,-218.999999448106));
#54749=CARTESIAN_POINT('',(144.115917770962,330.027992730186,-218.999999448106));
#54750=CARTESIAN_POINT('Origin',(184.115917770962,326.027992730186,-218.999999448106));
#54751=CARTESIAN_POINT('Origin',(144.115917770962,330.027992730186,-218.999999448106));
#54752=CARTESIAN_POINT('',(453.615917770962,330.027992730186,-250.999999448107));
#54753=CARTESIAN_POINT('',(453.615917770962,330.027992730186,-226.999999448107));
#54754=CARTESIAN_POINT('',(184.115917770962,330.027992730186,-250.999999448106));
#54755=CARTESIAN_POINT('',(144.115917770962,330.027992730186,-250.999999448106));
#54756=CARTESIAN_POINT('',(184.115917770962,330.027992730186,-226.999999448106));
#54757=CARTESIAN_POINT('Origin',(144.115917770962,326.027992730186,-250.999999448106));
#54758=CARTESIAN_POINT('Origin',(453.615917770962,326.027992730186,-250.999999448107));
#54759=CARTESIAN_POINT('Origin',(184.115917770962,326.027992730186,-250.999999448106));
#54760=CARTESIAN_POINT('Origin',(184.115917770962,310.027992730186,-234.999999448106));
#54761=CARTESIAN_POINT('Origin',(453.615917770962,310.027992730186,-234.999999448107));
#54762=CARTESIAN_POINT('Origin',(302.865917770965,330.027992730186,-216.999999448107));
#54763=CARTESIAN_POINT('',(334.865917770965,-269.972007269814,-216.999999448108));
#54764=CARTESIAN_POINT('',(302.865917770965,-269.972007269814,-216.999999448108));
#54765=CARTESIAN_POINT('',(310.865917770965,-269.972007269814,-216.999999448108));
#54766=CARTESIAN_POINT('',(302.865917770965,290.027992730186,-216.999999448107));
#54767=CARTESIAN_POINT('',(302.865917770965,330.027992730186,-216.999999448107));
#54768=CARTESIAN_POINT('',(334.865917770965,290.027992730186,-216.999999448107));
#54769=CARTESIAN_POINT('',(310.865917770965,290.027992730186,-216.999999448107));
#54770=CARTESIAN_POINT('',(334.865917770965,330.027992730186,-216.999999448107));
#54771=CARTESIAN_POINT('Origin',(302.865917770965,330.027992730186,-218.999999448107));
#54772=CARTESIAN_POINT('',(300.865917770965,-269.972007269814,-218.999999448108));
#54773=CARTESIAN_POINT('Origin',(302.865917770965,-269.972007269814,-218.999999448108));
#54774=CARTESIAN_POINT('',(300.865917770965,290.027992730186,-218.999999448107));
#54775=CARTESIAN_POINT('',(300.865917770965,330.027992730186,-218.999999448107));
#54776=CARTESIAN_POINT('Origin',(302.865917770965,290.027992730186,-218.999999448107));
#54777=CARTESIAN_POINT('Origin',(300.865917770965,330.027992730186,-250.999999448107));
#54778=CARTESIAN_POINT('',(300.865917770965,-269.972007269814,-250.999999448108));
#54779=CARTESIAN_POINT('',(300.865917770965,-269.972007269814,-242.999999448108));
#54780=CARTESIAN_POINT('',(300.865917770965,290.027992730186,-250.999999448107));
#54781=CARTESIAN_POINT('',(300.865917770965,330.027992730186,-250.999999448107));
#54782=CARTESIAN_POINT('',(300.865917770965,290.027992730186,-242.999999448107));
#54783=CARTESIAN_POINT('Origin',(302.865917770965,330.027992730186,-250.999999448107));
#54784=CARTESIAN_POINT('',(302.865917770965,-269.972007269814,-252.999999448108));
#54785=CARTESIAN_POINT('Origin',(302.865917770965,-269.972007269814,-250.999999448108));
#54786=CARTESIAN_POINT('',(302.865917770965,290.027992730186,-252.999999448107));
#54787=CARTESIAN_POINT('',(302.865917770965,330.027992730186,-252.999999448107));
#54788=CARTESIAN_POINT('Origin',(302.865917770965,290.027992730186,-250.999999448107));
#54789=CARTESIAN_POINT('Origin',(298.865917770965,330.027992730186,-250.999999448107));
#54790=CARTESIAN_POINT('',(298.865917770965,-269.972007269814,-250.999999448108));
#54791=CARTESIAN_POINT('',(298.865917770965,-269.972007269814,-218.999999448108));
#54792=CARTESIAN_POINT('',(298.865917770965,-269.972007269814,-242.999999448108));
#54793=CARTESIAN_POINT('',(298.865917770965,290.027992730186,-218.999999448107));
#54794=CARTESIAN_POINT('',(298.865917770965,330.027992730186,-218.999999448107));
#54795=CARTESIAN_POINT('',(298.865917770965,290.027992730186,-250.999999448107));
#54796=CARTESIAN_POINT('',(298.865917770965,290.027992730186,-242.999999448107));
#54797=CARTESIAN_POINT('',(298.865917770965,330.027992730186,-250.999999448107));
#54798=CARTESIAN_POINT('Origin',(302.865917770965,330.027992730186,-218.999999448107));
#54799=CARTESIAN_POINT('',(302.865917770965,-269.972007269814,-214.999999448108));
#54800=CARTESIAN_POINT('Origin',(302.865917770965,-269.972007269814,-218.999999448108));
#54801=CARTESIAN_POINT('',(302.865917770965,290.027992730186,-214.999999448107));
#54802=CARTESIAN_POINT('',(302.865917770965,330.027992730186,-214.999999448107));
#54803=CARTESIAN_POINT('Origin',(302.865917770965,290.027992730186,-218.999999448107));
#54804=CARTESIAN_POINT('Origin',(302.865917770965,330.027992730186,-214.999999448107));
#54805=CARTESIAN_POINT('',(334.865917770965,-269.972007269814,-214.999999448108));
#54806=CARTESIAN_POINT('',(310.865917770965,-269.972007269814,-214.999999448108));
#54807=CARTESIAN_POINT('',(334.865917770965,290.027992730186,-214.999999448107));
#54808=CARTESIAN_POINT('',(334.865917770965,330.027992730186,-214.999999448107));
#54809=CARTESIAN_POINT('',(310.865917770965,290.027992730186,-214.999999448107));
#54810=CARTESIAN_POINT('Origin',(334.865917770965,330.027992730186,-218.999999448107));
#54811=CARTESIAN_POINT('',(338.865917770965,-269.972007269814,-218.999999448108));
#54812=CARTESIAN_POINT('Origin',(334.865917770965,-269.972007269814,-218.999999448108));
#54813=CARTESIAN_POINT('',(338.865917770965,290.027992730186,-218.999999448107));
#54814=CARTESIAN_POINT('',(338.865917770965,330.027992730186,-218.999999448107));
#54815=CARTESIAN_POINT('Origin',(334.865917770965,290.027992730186,-218.999999448107));
#54816=CARTESIAN_POINT('Origin',(334.865917770965,330.027992730186,-252.999999448107));
#54817=CARTESIAN_POINT('',(334.865917770965,-269.972007269814,-252.999999448108));
#54818=CARTESIAN_POINT('',(326.865917770965,-269.972007269814,-252.999999448108));
#54819=CARTESIAN_POINT('',(334.865917770965,290.027992730186,-252.999999448107));
#54820=CARTESIAN_POINT('',(334.865917770965,330.027992730186,-252.999999448107));
#54821=CARTESIAN_POINT('',(326.865917770965,290.027992730186,-252.999999448107));
#54822=CARTESIAN_POINT('Origin',(334.865917770965,330.027992730186,-218.999999448107));
#54823=CARTESIAN_POINT('',(336.865917770965,-269.972007269814,-218.999999448108));
#54824=CARTESIAN_POINT('Origin',(334.865917770965,-269.972007269814,-218.999999448108));
#54825=CARTESIAN_POINT('',(336.865917770965,290.027992730186,-218.999999448107));
#54826=CARTESIAN_POINT('Origin',(334.865917770965,290.027992730186,-218.999999448107));
#54827=CARTESIAN_POINT('',(336.865917770965,330.027992730186,-218.999999448107));
#54828=CARTESIAN_POINT('Origin',(336.865917770965,330.027992730186,-218.999999448107));
#54829=CARTESIAN_POINT('',(336.865917770965,-269.972007269814,-250.999999448108));
#54830=CARTESIAN_POINT('',(336.865917770965,-269.972007269814,-226.999999448108));
#54831=CARTESIAN_POINT('',(336.865917770965,290.027992730186,-250.999999448107));
#54832=CARTESIAN_POINT('',(336.865917770965,290.027992730186,-226.999999448107));
#54833=CARTESIAN_POINT('',(336.865917770965,330.027992730186,-250.999999448107));
#54834=CARTESIAN_POINT('Origin',(334.865917770965,330.027992730186,-250.999999448107));
#54835=CARTESIAN_POINT('Origin',(334.865917770965,-269.972007269814,-250.999999448108));
#54836=CARTESIAN_POINT('Origin',(334.865917770965,290.027992730186,-250.999999448107));
#54837=CARTESIAN_POINT('Origin',(338.865917770965,330.027992730186,-218.999999448107));
#54838=CARTESIAN_POINT('',(338.865917770965,-269.972007269814,-250.999999448108));
#54839=CARTESIAN_POINT('',(338.865917770965,-269.972007269814,-226.999999448108));
#54840=CARTESIAN_POINT('',(338.865917770965,290.027992730186,-250.999999448107));
#54841=CARTESIAN_POINT('',(338.865917770965,330.027992730186,-250.999999448107));
#54842=CARTESIAN_POINT('',(338.865917770965,290.027992730186,-226.999999448107));
#54843=CARTESIAN_POINT('Origin',(334.865917770965,330.027992730186,-250.999999448107));
#54844=CARTESIAN_POINT('',(334.865917770965,-269.972007269814,-254.999999448108));
#54845=CARTESIAN_POINT('Origin',(334.865917770965,-269.972007269814,-250.999999448108));
#54846=CARTESIAN_POINT('',(334.865917770965,290.027992730186,-254.999999448107));
#54847=CARTESIAN_POINT('',(334.865917770965,330.027992730186,-254.999999448107));
#54848=CARTESIAN_POINT('Origin',(334.865917770965,290.027992730186,-250.999999448107));
#54849=CARTESIAN_POINT('Origin',(334.865917770965,330.027992730186,-254.999999448107));
#54850=CARTESIAN_POINT('',(302.865917770965,-269.972007269814,-254.999999448108));
#54851=CARTESIAN_POINT('',(326.865917770965,-269.972007269814,-254.999999448108));
#54852=CARTESIAN_POINT('',(302.865917770965,290.027992730186,-254.999999448107));
#54853=CARTESIAN_POINT('',(302.865917770965,330.027992730186,-254.999999448107));
#54854=CARTESIAN_POINT('',(326.865917770965,290.027992730186,-254.999999448107));
#54855=CARTESIAN_POINT('Origin',(302.865917770965,330.027992730186,-250.999999448107));
#54856=CARTESIAN_POINT('Origin',(302.865917770965,-269.972007269814,-250.999999448108));
#54857=CARTESIAN_POINT('Origin',(302.865917770965,290.027992730186,-250.999999448107));
#54858=CARTESIAN_POINT('Origin',(318.865917770965,290.027992730186,-234.999999448107));
#54859=CARTESIAN_POINT('Origin',(318.865917770965,-269.972007269814,-234.999999448108));
#54860=CARTESIAN_POINT('Origin',(148.115917770962,-305.972007269816,-379.2202872414));
#54861=CARTESIAN_POINT('',(148.115917770962,-309.972007269816,-379.220287241394));
#54862=CARTESIAN_POINT('',(144.115917770962,-305.972007269816,-379.2202872414));
#54863=CARTESIAN_POINT('Origin',(148.115917770962,-305.972007269816,-379.2202872414));
#54864=CARTESIAN_POINT('',(148.115917770962,-309.972007269823,-384.220287241394));
#54865=CARTESIAN_POINT('',(148.115917770962,-309.972007269816,-379.220287241394));
#54866=CARTESIAN_POINT('',(144.115917770962,-305.972007269823,-384.2202872414));
#54867=CARTESIAN_POINT('Origin',(148.115917770962,-305.972007269823,-384.2202872414));
#54868=CARTESIAN_POINT('',(144.115917770962,-305.972007269816,-379.2202872414));
#54869=CARTESIAN_POINT('Origin',(180.115917770962,-309.972007269816,-379.220287241394));
#54870=CARTESIAN_POINT('',(180.115917770962,-309.972007269816,-379.220287241394));
#54871=CARTESIAN_POINT('',(172.11591777096,-309.972007269816,-379.220287241394));
#54872=CARTESIAN_POINT('',(180.115917770962,-309.972007269823,-384.220287241394));
#54873=CARTESIAN_POINT('',(180.115917770962,-309.972007269816,-379.220287241394));
#54874=CARTESIAN_POINT('',(172.11591777096,-309.972007269823,-384.220287241394));
#54875=CARTESIAN_POINT('Origin',(180.115917770962,-305.972007269816,-379.2202872414));
#54876=CARTESIAN_POINT('',(184.115917770962,-305.972007269816,-379.2202872414));
#54877=CARTESIAN_POINT('Origin',(180.115917770962,-305.972007269816,-379.2202872414));
#54878=CARTESIAN_POINT('',(184.115917770962,-305.972007269823,-384.2202872414));
#54879=CARTESIAN_POINT('',(184.115917770962,-305.972007269816,-379.2202872414));
#54880=CARTESIAN_POINT('Origin',(180.115917770962,-305.972007269823,-384.2202872414));
#54881=CARTESIAN_POINT('Origin',(184.115917770962,-273.972007269816,-379.220287241446));
#54882=CARTESIAN_POINT('',(184.115917770962,-273.972007269816,-379.220287241446));
#54883=CARTESIAN_POINT('',(184.115917770962,-281.972007269816,-379.220287241435));
#54884=CARTESIAN_POINT('',(184.115917770962,-273.972007269823,-384.220287241446));
#54885=CARTESIAN_POINT('',(184.115917770962,-273.972007269816,-379.220287241446));
#54886=CARTESIAN_POINT('',(184.115917770962,-281.972007269823,-384.220287241435));
#54887=CARTESIAN_POINT('Origin',(180.115917770962,-273.972007269816,-379.220287241446));
#54888=CARTESIAN_POINT('',(180.115917770961,-269.972007269816,-379.220287241452));
#54889=CARTESIAN_POINT('Origin',(180.115917770962,-273.972007269816,-379.220287241446));
#54890=CARTESIAN_POINT('',(180.115917770961,-269.972007269823,-384.220287241452));
#54891=CARTESIAN_POINT('',(180.115917770961,-269.972007269816,-379.220287241452));
#54892=CARTESIAN_POINT('Origin',(180.115917770962,-273.972007269823,-384.220287241446));
#54893=CARTESIAN_POINT('Origin',(148.115917770962,-269.972007269816,-379.220287241452));
#54894=CARTESIAN_POINT('',(148.115917770962,-269.972007269816,-379.220287241452));
#54895=CARTESIAN_POINT('',(156.11591777096,-269.972007269816,-379.220287241452));
#54896=CARTESIAN_POINT('',(148.115917770962,-269.972007269823,-384.220287241452));
#54897=CARTESIAN_POINT('',(148.115917770962,-269.972007269816,-379.220287241452));
#54898=CARTESIAN_POINT('',(156.11591777096,-269.972007269823,-384.220287241452));
#54899=CARTESIAN_POINT('Origin',(148.115917770962,-273.972007269816,-379.220287241446));
#54900=CARTESIAN_POINT('',(144.115917770962,-273.972007269816,-379.220287241446));
#54901=CARTESIAN_POINT('Origin',(148.115917770962,-273.972007269816,-379.220287241446));
#54902=CARTESIAN_POINT('',(144.115917770962,-273.972007269823,-384.220287241446));
#54903=CARTESIAN_POINT('',(144.115917770962,-273.972007269816,-379.220287241446));
#54904=CARTESIAN_POINT('Origin',(148.115917770962,-273.972007269823,-384.220287241446));
#54905=CARTESIAN_POINT('Origin',(144.115917770962,-305.972007269816,-379.2202872414));
#54906=CARTESIAN_POINT('',(144.115917770962,-297.972007269816,-379.220287241412));
#54907=CARTESIAN_POINT('',(144.115917770962,-297.972007269823,-384.220287241412));
#54908=CARTESIAN_POINT('Origin',(148.115917770962,-273.972007269816,-379.220287241446));
#54909=CARTESIAN_POINT('',(148.115917770939,-249.972007269814,-379.220287241481));
#54910=CARTESIAN_POINT('',(124.11591777096,-273.972007269756,-379.220287241446));
#54911=CARTESIAN_POINT('Origin',(148.115917770962,-273.972007269816,-379.220287241446));
#54912=CARTESIAN_POINT('',(148.115917770939,-249.972007269821,-384.220287241481));
#54913=CARTESIAN_POINT('',(148.115917770939,-249.972007269814,-379.220287241481));
#54914=CARTESIAN_POINT('',(124.11591777096,-273.972007269763,-384.220287241446));
#54915=CARTESIAN_POINT('Origin',(148.115917770962,-273.972007269823,-384.220287241446));
#54916=CARTESIAN_POINT('',(124.11591777096,-273.972007269756,-379.220287241446));
#54917=CARTESIAN_POINT('Origin',(124.11591777096,-305.972007269872,-379.2202872414));
#54918=CARTESIAN_POINT('',(124.11591777096,-305.972007269872,-379.2202872414));
#54919=CARTESIAN_POINT('',(124.11591777096,-273.972007269756,-379.220287241446));
#54920=CARTESIAN_POINT('',(124.11591777096,-305.972007269879,-384.2202872414));
#54921=CARTESIAN_POINT('',(124.11591777096,-273.972007269763,-384.220287241446));
#54922=CARTESIAN_POINT('',(124.11591777096,-305.972007269872,-379.2202872414));
#54923=CARTESIAN_POINT('Origin',(148.115917770962,-305.972007269816,-379.2202872414));
#54924=CARTESIAN_POINT('',(148.115917770939,-329.972007269817,-379.220287241365));
#54925=CARTESIAN_POINT('Origin',(148.115917770962,-305.972007269816,-379.2202872414));
#54926=CARTESIAN_POINT('',(148.115917770939,-329.972007269824,-384.220287241365));
#54927=CARTESIAN_POINT('Origin',(148.115917770962,-305.972007269823,-384.2202872414));
#54928=CARTESIAN_POINT('',(148.115917770939,-329.972007269817,-379.220287241365));
#54929=CARTESIAN_POINT('Origin',(180.11591777091,-329.972007269817,-379.220287241365));
#54930=CARTESIAN_POINT('',(180.11591777091,-329.972007269817,-379.220287241365));
#54931=CARTESIAN_POINT('',(148.115917770939,-329.972007269817,-379.220287241365));
#54932=CARTESIAN_POINT('',(180.11591777091,-329.972007269824,-384.220287241365));
#54933=CARTESIAN_POINT('',(148.115917770939,-329.972007269824,-384.220287241365));
#54934=CARTESIAN_POINT('',(180.11591777091,-329.972007269817,-379.220287241365));
#54935=CARTESIAN_POINT('Origin',(180.115917770962,-305.972007269816,-379.2202872414));
#54936=CARTESIAN_POINT('',(204.115917770963,-305.972007269872,-379.2202872414));
#54937=CARTESIAN_POINT('Origin',(180.115917770962,-305.972007269816,-379.2202872414));
#54938=CARTESIAN_POINT('',(204.115917770963,-305.972007269879,-384.2202872414));
#54939=CARTESIAN_POINT('Origin',(180.115917770962,-305.972007269823,-384.2202872414));
#54940=CARTESIAN_POINT('',(204.115917770963,-305.972007269872,-379.2202872414));
#54941=CARTESIAN_POINT('Origin',(204.115917770963,-273.972007269756,-379.220287241447));
#54942=CARTESIAN_POINT('',(204.115917770963,-273.972007269756,-379.220287241447));
#54943=CARTESIAN_POINT('',(204.115917770963,-305.972007269872,-379.2202872414));
#54944=CARTESIAN_POINT('',(204.115917770963,-273.972007269763,-384.220287241447));
#54945=CARTESIAN_POINT('',(204.115917770963,-305.972007269879,-384.2202872414));
#54946=CARTESIAN_POINT('',(204.115917770963,-273.972007269756,-379.220287241447));
#54947=CARTESIAN_POINT('Origin',(180.115917770962,-273.972007269816,-379.220287241446));
#54948=CARTESIAN_POINT('',(180.11591777091,-249.972007269814,-379.220287241481));
#54949=CARTESIAN_POINT('Origin',(180.115917770962,-273.972007269816,-379.220287241446));
#54950=CARTESIAN_POINT('',(180.11591777091,-249.972007269821,-384.220287241481));
#54951=CARTESIAN_POINT('Origin',(180.115917770962,-273.972007269823,-384.220287241446));
#54952=CARTESIAN_POINT('',(180.11591777091,-249.972007269814,-379.220287241481));
#54953=CARTESIAN_POINT('Origin',(148.115917770939,-249.972007269814,-379.220287241481));
#54954=CARTESIAN_POINT('',(180.11591777091,-249.972007269814,-379.220287241481));
#54955=CARTESIAN_POINT('',(180.11591777091,-249.972007269821,-384.220287241481));
#54956=CARTESIAN_POINT('Origin',(164.115917770959,-289.972007269816,-379.220287241423));
#54957=CARTESIAN_POINT('Origin',(164.115917770959,-289.972007269823,-384.220287241423));
#54958=CARTESIAN_POINT('Origin',(457.615917770968,294.027992730186,-379.220287242272));
#54959=CARTESIAN_POINT('',(457.615917770968,290.027992730186,-379.220287242266));
#54960=CARTESIAN_POINT('',(453.615917770968,294.027992730186,-379.220287242272));
#54961=CARTESIAN_POINT('Origin',(457.615917770968,294.027992730186,-379.220287242272));
#54962=CARTESIAN_POINT('',(457.615917770968,290.027992730179,-384.220287242266));
#54963=CARTESIAN_POINT('',(457.615917770968,290.027992730186,-379.220287242266));
#54964=CARTESIAN_POINT('',(453.615917770968,294.027992730179,-384.220287242272));
#54965=CARTESIAN_POINT('Origin',(457.615917770968,294.027992730179,-384.220287242272));
#54966=CARTESIAN_POINT('',(453.615917770968,294.027992730186,-379.220287242272));
#54967=CARTESIAN_POINT('Origin',(489.615917770968,290.027992730186,-379.220287242266));
#54968=CARTESIAN_POINT('',(489.615917770968,290.027992730186,-379.220287242266));
#54969=CARTESIAN_POINT('',(481.615917770966,290.027992730186,-379.220287242266));
#54970=CARTESIAN_POINT('',(489.615917770968,290.027992730179,-384.220287242266));
#54971=CARTESIAN_POINT('',(489.615917770968,290.027992730186,-379.220287242266));
#54972=CARTESIAN_POINT('',(481.615917770966,290.027992730179,-384.220287242266));
#54973=CARTESIAN_POINT('Origin',(489.615917770968,294.027992730186,-379.220287242272));
#54974=CARTESIAN_POINT('',(493.615917770968,294.027992730186,-379.220287242272));
#54975=CARTESIAN_POINT('Origin',(489.615917770968,294.027992730186,-379.220287242272));
#54976=CARTESIAN_POINT('',(493.615917770968,294.027992730179,-384.220287242272));
#54977=CARTESIAN_POINT('',(493.615917770968,294.027992730186,-379.220287242272));
#54978=CARTESIAN_POINT('Origin',(489.615917770968,294.027992730179,-384.220287242272));
#54979=CARTESIAN_POINT('Origin',(493.615917770968,326.027992730186,-379.220287242318));
#54980=CARTESIAN_POINT('',(493.615917770968,326.027992730186,-379.220287242318));
#54981=CARTESIAN_POINT('',(493.615917770968,318.027992730186,-379.220287242307));
#54982=CARTESIAN_POINT('',(493.615917770968,326.027992730179,-384.220287242318));
#54983=CARTESIAN_POINT('',(493.615917770968,326.027992730186,-379.220287242318));
#54984=CARTESIAN_POINT('',(493.615917770968,318.027992730179,-384.220287242307));
#54985=CARTESIAN_POINT('Origin',(489.615917770968,326.027992730186,-379.220287242318));
#54986=CARTESIAN_POINT('',(489.615917770967,330.027992730186,-379.220287242324));
#54987=CARTESIAN_POINT('Origin',(489.615917770968,326.027992730186,-379.220287242318));
#54988=CARTESIAN_POINT('',(489.615917770967,330.027992730179,-384.220287242324));
#54989=CARTESIAN_POINT('',(489.615917770967,330.027992730186,-379.220287242324));
#54990=CARTESIAN_POINT('Origin',(489.615917770968,326.027992730179,-384.220287242318));
#54991=CARTESIAN_POINT('Origin',(457.615917770968,330.027992730186,-379.220287242324));
#54992=CARTESIAN_POINT('',(457.615917770968,330.027992730186,-379.220287242324));
#54993=CARTESIAN_POINT('',(465.615917770966,330.027992730186,-379.220287242324));
#54994=CARTESIAN_POINT('',(457.615917770968,330.027992730179,-384.220287242324));
#54995=CARTESIAN_POINT('',(457.615917770968,330.027992730186,-379.220287242324));
#54996=CARTESIAN_POINT('',(465.615917770966,330.027992730179,-384.220287242324));
#54997=CARTESIAN_POINT('Origin',(457.615917770968,326.027992730186,-379.220287242318));
#54998=CARTESIAN_POINT('',(453.615917770968,326.027992730186,-379.220287242318));
#54999=CARTESIAN_POINT('Origin',(457.615917770968,326.027992730186,-379.220287242318));
#55000=CARTESIAN_POINT('',(453.615917770968,326.027992730179,-384.220287242318));
#55001=CARTESIAN_POINT('',(453.615917770968,326.027992730186,-379.220287242318));
#55002=CARTESIAN_POINT('Origin',(457.615917770968,326.027992730179,-384.220287242318));
#55003=CARTESIAN_POINT('Origin',(453.615917770968,294.027992730186,-379.220287242272));
#55004=CARTESIAN_POINT('',(453.615917770968,302.027992730186,-379.220287242283));
#55005=CARTESIAN_POINT('',(453.615917770968,302.027992730179,-384.220287242283));
#55006=CARTESIAN_POINT('Origin',(457.615917770968,326.027992730186,-379.220287242318));
#55007=CARTESIAN_POINT('',(457.615917770945,350.027992730188,-379.220287242353));
#55008=CARTESIAN_POINT('',(433.615917770966,326.027992730246,-379.220287242318));
#55009=CARTESIAN_POINT('Origin',(457.615917770968,326.027992730186,-379.220287242318));
#55010=CARTESIAN_POINT('',(457.615917770945,350.027992730181,-384.220287242353));
#55011=CARTESIAN_POINT('',(457.615917770945,350.027992730188,-379.220287242353));
#55012=CARTESIAN_POINT('',(433.615917770966,326.027992730239,-384.220287242318));
#55013=CARTESIAN_POINT('Origin',(457.615917770968,326.027992730179,-384.220287242318));
#55014=CARTESIAN_POINT('',(433.615917770966,326.027992730246,-379.220287242318));
#55015=CARTESIAN_POINT('Origin',(433.615917770966,294.02799273013,-379.220287242272));
#55016=CARTESIAN_POINT('',(433.615917770966,294.02799273013,-379.220287242272));
#55017=CARTESIAN_POINT('',(433.615917770966,326.027992730246,-379.220287242318));
#55018=CARTESIAN_POINT('',(433.615917770966,294.027992730123,-384.220287242272));
#55019=CARTESIAN_POINT('',(433.615917770966,326.027992730239,-384.220287242318));
#55020=CARTESIAN_POINT('',(433.615917770966,294.02799273013,-379.220287242272));
#55021=CARTESIAN_POINT('Origin',(457.615917770968,294.027992730186,-379.220287242272));
#55022=CARTESIAN_POINT('',(457.615917770945,270.027992730185,-379.220287242237));
#55023=CARTESIAN_POINT('Origin',(457.615917770968,294.027992730186,-379.220287242272));
#55024=CARTESIAN_POINT('',(457.615917770945,270.027992730178,-384.220287242237));
#55025=CARTESIAN_POINT('Origin',(457.615917770968,294.027992730179,-384.220287242272));
#55026=CARTESIAN_POINT('',(457.615917770945,270.027992730185,-379.220287242237));
#55027=CARTESIAN_POINT('Origin',(489.615917770916,270.027992730185,-379.220287242237));
#55028=CARTESIAN_POINT('',(489.615917770916,270.027992730185,-379.220287242237));
#55029=CARTESIAN_POINT('',(457.615917770945,270.027992730185,-379.220287242237));
#55030=CARTESIAN_POINT('',(489.615917770916,270.027992730178,-384.220287242237));
#55031=CARTESIAN_POINT('',(457.615917770945,270.027992730178,-384.220287242237));
#55032=CARTESIAN_POINT('',(489.615917770916,270.027992730185,-379.220287242237));
#55033=CARTESIAN_POINT('Origin',(489.615917770968,294.027992730186,-379.220287242272));
#55034=CARTESIAN_POINT('',(513.615917770969,294.02799273013,-379.220287242272));
#55035=CARTESIAN_POINT('Origin',(489.615917770968,294.027992730186,-379.220287242272));
#55036=CARTESIAN_POINT('',(513.615917770969,294.027992730123,-384.220287242272));
#55037=CARTESIAN_POINT('Origin',(489.615917770968,294.027992730179,-384.220287242272));
#55038=CARTESIAN_POINT('',(513.615917770969,294.02799273013,-379.220287242272));
#55039=CARTESIAN_POINT('Origin',(513.615917770969,326.027992730246,-379.220287242318));
#55040=CARTESIAN_POINT('',(513.615917770969,326.027992730246,-379.220287242318));
#55041=CARTESIAN_POINT('',(513.615917770969,294.02799273013,-379.220287242272));
#55042=CARTESIAN_POINT('',(513.615917770969,326.027992730239,-384.220287242318));
#55043=CARTESIAN_POINT('',(513.615917770969,294.027992730123,-384.220287242272));
#55044=CARTESIAN_POINT('',(513.615917770969,326.027992730246,-379.220287242318));
#55045=CARTESIAN_POINT('Origin',(489.615917770968,326.027992730186,-379.220287242318));
#55046=CARTESIAN_POINT('',(489.615917770916,350.027992730188,-379.220287242353));
#55047=CARTESIAN_POINT('Origin',(489.615917770968,326.027992730186,-379.220287242318));
#55048=CARTESIAN_POINT('',(489.615917770916,350.027992730181,-384.220287242353));
#55049=CARTESIAN_POINT('Origin',(489.615917770968,326.027992730179,-384.220287242318));
#55050=CARTESIAN_POINT('',(489.615917770916,350.027992730188,-379.220287242353));
#55051=CARTESIAN_POINT('Origin',(457.615917770945,350.027992730188,-379.220287242353));
#55052=CARTESIAN_POINT('',(489.615917770916,350.027992730188,-379.220287242353));
#55053=CARTESIAN_POINT('',(489.615917770916,350.027992730181,-384.220287242353));
#55054=CARTESIAN_POINT('Origin',(473.615917770965,310.027992730186,-379.220287242295));
#55055=CARTESIAN_POINT('Origin',(473.615917770965,310.027992730179,-384.220287242295));
#55056=CARTESIAN_POINT('Origin',(148.115917770962,294.027992730186,-379.220287242271));
#55057=CARTESIAN_POINT('',(148.115917770962,290.027992730186,-379.220287242265));
#55058=CARTESIAN_POINT('',(144.115917770962,294.027992730186,-379.220287242271));
#55059=CARTESIAN_POINT('Origin',(148.115917770962,294.027992730186,-379.220287242271));
#55060=CARTESIAN_POINT('',(148.115917770962,290.027992730179,-384.220287242265));
#55061=CARTESIAN_POINT('',(148.115917770962,290.027992730186,-379.220287242265));
#55062=CARTESIAN_POINT('',(144.115917770962,294.027992730179,-384.220287242271));
#55063=CARTESIAN_POINT('Origin',(148.115917770962,294.027992730179,-384.220287242271));
#55064=CARTESIAN_POINT('',(144.115917770962,294.027992730186,-379.220287242271));
#55065=CARTESIAN_POINT('Origin',(180.115917770962,290.027992730186,-379.220287242265));
#55066=CARTESIAN_POINT('',(180.115917770962,290.027992730186,-379.220287242265));
#55067=CARTESIAN_POINT('',(172.11591777096,290.027992730186,-379.220287242265));
#55068=CARTESIAN_POINT('',(180.115917770962,290.027992730179,-384.220287242265));
#55069=CARTESIAN_POINT('',(180.115917770962,290.027992730186,-379.220287242265));
#55070=CARTESIAN_POINT('',(172.11591777096,290.027992730179,-384.220287242265));
#55071=CARTESIAN_POINT('Origin',(180.115917770962,294.027992730186,-379.220287242271));
#55072=CARTESIAN_POINT('',(184.115917770962,294.027992730186,-379.220287242271));
#55073=CARTESIAN_POINT('Origin',(180.115917770962,294.027992730186,-379.220287242271));
#55074=CARTESIAN_POINT('',(184.115917770962,294.027992730179,-384.220287242271));
#55075=CARTESIAN_POINT('',(184.115917770962,294.027992730186,-379.220287242271));
#55076=CARTESIAN_POINT('Origin',(180.115917770962,294.027992730179,-384.220287242271));
#55077=CARTESIAN_POINT('Origin',(184.115917770962,326.027992730186,-379.220287242317));
#55078=CARTESIAN_POINT('',(184.115917770962,326.027992730186,-379.220287242317));
#55079=CARTESIAN_POINT('',(184.115917770962,318.027992730186,-379.220287242306));
#55080=CARTESIAN_POINT('',(184.115917770962,326.027992730179,-384.220287242317));
#55081=CARTESIAN_POINT('',(184.115917770962,326.027992730186,-379.220287242317));
#55082=CARTESIAN_POINT('',(184.115917770962,318.027992730179,-384.220287242306));
#55083=CARTESIAN_POINT('Origin',(180.115917770962,326.027992730186,-379.220287242317));
#55084=CARTESIAN_POINT('',(180.115917770961,330.027992730186,-379.220287242323));
#55085=CARTESIAN_POINT('Origin',(180.115917770962,326.027992730186,-379.220287242317));
#55086=CARTESIAN_POINT('',(180.115917770961,330.027992730179,-384.220287242323));
#55087=CARTESIAN_POINT('',(180.115917770961,330.027992730186,-379.220287242323));
#55088=CARTESIAN_POINT('Origin',(180.115917770962,326.027992730179,-384.220287242317));
#55089=CARTESIAN_POINT('Origin',(148.115917770962,330.027992730186,-379.220287242323));
#55090=CARTESIAN_POINT('',(148.115917770962,330.027992730186,-379.220287242323));
#55091=CARTESIAN_POINT('',(156.11591777096,330.027992730186,-379.220287242323));
#55092=CARTESIAN_POINT('',(148.115917770962,330.027992730179,-384.220287242323));
#55093=CARTESIAN_POINT('',(148.115917770962,330.027992730186,-379.220287242323));
#55094=CARTESIAN_POINT('',(156.11591777096,330.027992730179,-384.220287242323));
#55095=CARTESIAN_POINT('Origin',(148.115917770962,326.027992730186,-379.220287242317));
#55096=CARTESIAN_POINT('',(144.115917770962,326.027992730186,-379.220287242317));
#55097=CARTESIAN_POINT('Origin',(148.115917770962,326.027992730186,-379.220287242317));
#55098=CARTESIAN_POINT('',(144.115917770962,326.027992730179,-384.220287242317));
#55099=CARTESIAN_POINT('',(144.115917770962,326.027992730186,-379.220287242317));
#55100=CARTESIAN_POINT('Origin',(148.115917770962,326.027992730179,-384.220287242317));
#55101=CARTESIAN_POINT('Origin',(144.115917770962,294.027992730186,-379.220287242271));
#55102=CARTESIAN_POINT('',(144.115917770962,302.027992730186,-379.220287242282));
#55103=CARTESIAN_POINT('',(144.115917770962,302.027992730179,-384.220287242282));
#55104=CARTESIAN_POINT('Origin',(148.115917770962,326.027992730186,-379.220287242317));
#55105=CARTESIAN_POINT('',(148.115917770939,350.027992730188,-379.220287242352));
#55106=CARTESIAN_POINT('',(124.11591777096,326.027992730246,-379.220287242317));
#55107=CARTESIAN_POINT('Origin',(148.115917770962,326.027992730186,-379.220287242317));
#55108=CARTESIAN_POINT('',(148.115917770939,350.027992730181,-384.220287242352));
#55109=CARTESIAN_POINT('',(148.115917770939,350.027992730188,-379.220287242352));
#55110=CARTESIAN_POINT('',(124.11591777096,326.027992730239,-384.220287242317));
#55111=CARTESIAN_POINT('Origin',(148.115917770962,326.027992730179,-384.220287242317));
#55112=CARTESIAN_POINT('',(124.11591777096,326.027992730246,-379.220287242317));
#55113=CARTESIAN_POINT('Origin',(124.11591777096,294.02799273013,-379.220287242271));
#55114=CARTESIAN_POINT('',(124.11591777096,294.02799273013,-379.220287242271));
#55115=CARTESIAN_POINT('',(124.11591777096,326.027992730246,-379.220287242317));
#55116=CARTESIAN_POINT('',(124.11591777096,294.027992730123,-384.220287242271));
#55117=CARTESIAN_POINT('',(124.11591777096,326.027992730239,-384.220287242317));
#55118=CARTESIAN_POINT('',(124.11591777096,294.02799273013,-379.220287242271));
#55119=CARTESIAN_POINT('Origin',(148.115917770962,294.027992730186,-379.220287242271));
#55120=CARTESIAN_POINT('',(148.115917770939,270.027992730185,-379.220287242236));
#55121=CARTESIAN_POINT('Origin',(148.115917770962,294.027992730186,-379.220287242271));
#55122=CARTESIAN_POINT('',(148.115917770939,270.027992730178,-384.220287242236));
#55123=CARTESIAN_POINT('Origin',(148.115917770962,294.027992730179,-384.220287242271));
#55124=CARTESIAN_POINT('',(148.115917770939,270.027992730185,-379.220287242236));
#55125=CARTESIAN_POINT('Origin',(180.11591777091,270.027992730185,-379.220287242236));
#55126=CARTESIAN_POINT('',(180.11591777091,270.027992730185,-379.220287242236));
#55127=CARTESIAN_POINT('',(148.115917770939,270.027992730185,-379.220287242236));
#55128=CARTESIAN_POINT('',(180.11591777091,270.027992730178,-384.220287242236));
#55129=CARTESIAN_POINT('',(148.115917770939,270.027992730178,-384.220287242236));
#55130=CARTESIAN_POINT('',(180.11591777091,270.027992730185,-379.220287242236));
#55131=CARTESIAN_POINT('Origin',(180.115917770962,294.027992730186,-379.220287242271));
#55132=CARTESIAN_POINT('',(204.115917770963,294.02799273013,-379.220287242271));
#55133=CARTESIAN_POINT('Origin',(180.115917770962,294.027992730186,-379.220287242271));
#55134=CARTESIAN_POINT('',(204.115917770963,294.027992730123,-384.220287242271));
#55135=CARTESIAN_POINT('Origin',(180.115917770962,294.027992730179,-384.220287242271));
#55136=CARTESIAN_POINT('',(204.115917770963,294.02799273013,-379.220287242271));
#55137=CARTESIAN_POINT('Origin',(204.115917770963,326.027992730246,-379.220287242317));
#55138=CARTESIAN_POINT('',(204.115917770963,326.027992730246,-379.220287242317));
#55139=CARTESIAN_POINT('',(204.115917770963,294.02799273013,-379.220287242271));
#55140=CARTESIAN_POINT('',(204.115917770963,326.027992730239,-384.220287242317));
#55141=CARTESIAN_POINT('',(204.115917770963,294.027992730123,-384.220287242271));
#55142=CARTESIAN_POINT('',(204.115917770963,326.027992730246,-379.220287242317));
#55143=CARTESIAN_POINT('Origin',(180.115917770962,326.027992730186,-379.220287242317));
#55144=CARTESIAN_POINT('',(180.11591777091,350.027992730188,-379.220287242352));
#55145=CARTESIAN_POINT('Origin',(180.115917770962,326.027992730186,-379.220287242317));
#55146=CARTESIAN_POINT('',(180.11591777091,350.027992730181,-384.220287242352));
#55147=CARTESIAN_POINT('Origin',(180.115917770962,326.027992730179,-384.220287242317));
#55148=CARTESIAN_POINT('',(180.11591777091,350.027992730188,-379.220287242352));
#55149=CARTESIAN_POINT('Origin',(148.115917770939,350.027992730188,-379.220287242352));
#55150=CARTESIAN_POINT('',(180.11591777091,350.027992730188,-379.220287242352));
#55151=CARTESIAN_POINT('',(180.11591777091,350.027992730181,-384.220287242352));
#55152=CARTESIAN_POINT('Origin',(164.115917770959,310.027992730186,-379.220287242294));
#55153=CARTESIAN_POINT('Origin',(164.115917770959,310.027992730179,-384.220287242294));
#55154=CARTESIAN_POINT('Origin',(457.615917770968,-305.972007269816,-379.220287241401));
#55155=CARTESIAN_POINT('',(457.615917770968,-309.972007269816,-379.220287241395));
#55156=CARTESIAN_POINT('',(453.615917770968,-305.972007269816,-379.220287241401));
#55157=CARTESIAN_POINT('Origin',(457.615917770968,-305.972007269816,-379.220287241401));
#55158=CARTESIAN_POINT('',(457.615917770968,-309.972007269823,-384.220287241395));
#55159=CARTESIAN_POINT('',(457.615917770968,-309.972007269816,-379.220287241395));
#55160=CARTESIAN_POINT('',(453.615917770968,-305.972007269823,-384.220287241401));
#55161=CARTESIAN_POINT('Origin',(457.615917770968,-305.972007269823,-384.220287241401));
#55162=CARTESIAN_POINT('',(453.615917770968,-305.972007269816,-379.220287241401));
#55163=CARTESIAN_POINT('Origin',(489.615917770968,-309.972007269816,-379.220287241395));
#55164=CARTESIAN_POINT('',(489.615917770968,-309.972007269816,-379.220287241395));
#55165=CARTESIAN_POINT('',(481.615917770966,-309.972007269816,-379.220287241395));
#55166=CARTESIAN_POINT('',(489.615917770968,-309.972007269823,-384.220287241395));
#55167=CARTESIAN_POINT('',(489.615917770968,-309.972007269816,-379.220287241395));
#55168=CARTESIAN_POINT('',(481.615917770966,-309.972007269823,-384.220287241395));
#55169=CARTESIAN_POINT('Origin',(489.615917770968,-305.972007269816,-379.220287241401));
#55170=CARTESIAN_POINT('',(493.615917770968,-305.972007269816,-379.220287241401));
#55171=CARTESIAN_POINT('Origin',(489.615917770968,-305.972007269816,-379.220287241401));
#55172=CARTESIAN_POINT('',(493.615917770968,-305.972007269823,-384.220287241401));
#55173=CARTESIAN_POINT('',(493.615917770968,-305.972007269816,-379.220287241401));
#55174=CARTESIAN_POINT('Origin',(489.615917770968,-305.972007269823,-384.220287241401));
#55175=CARTESIAN_POINT('Origin',(493.615917770968,-273.972007269816,-379.220287241448));
#55176=CARTESIAN_POINT('',(493.615917770968,-273.972007269816,-379.220287241448));
#55177=CARTESIAN_POINT('',(493.615917770968,-281.972007269816,-379.220287241436));
#55178=CARTESIAN_POINT('',(493.615917770968,-273.972007269823,-384.220287241448));
#55179=CARTESIAN_POINT('',(493.615917770968,-273.972007269816,-379.220287241448));
#55180=CARTESIAN_POINT('',(493.615917770968,-281.972007269823,-384.220287241436));
#55181=CARTESIAN_POINT('Origin',(489.615917770968,-273.972007269816,-379.220287241448));
#55182=CARTESIAN_POINT('',(489.615917770967,-269.972007269816,-379.220287241453));
#55183=CARTESIAN_POINT('Origin',(489.615917770968,-273.972007269816,-379.220287241448));
#55184=CARTESIAN_POINT('',(489.615917770967,-269.972007269823,-384.220287241453));
#55185=CARTESIAN_POINT('',(489.615917770967,-269.972007269816,-379.220287241453));
#55186=CARTESIAN_POINT('Origin',(489.615917770968,-273.972007269823,-384.220287241448));
#55187=CARTESIAN_POINT('Origin',(457.615917770968,-269.972007269816,-379.220287241453));
#55188=CARTESIAN_POINT('',(457.615917770968,-269.972007269816,-379.220287241453));
#55189=CARTESIAN_POINT('',(465.615917770966,-269.972007269816,-379.220287241453));
#55190=CARTESIAN_POINT('',(457.615917770968,-269.972007269823,-384.220287241453));
#55191=CARTESIAN_POINT('',(457.615917770968,-269.972007269816,-379.220287241453));
#55192=CARTESIAN_POINT('',(465.615917770966,-269.972007269823,-384.220287241453));
#55193=CARTESIAN_POINT('Origin',(457.615917770968,-273.972007269816,-379.220287241447));
#55194=CARTESIAN_POINT('',(453.615917770968,-273.972007269816,-379.220287241447));
#55195=CARTESIAN_POINT('Origin',(457.615917770968,-273.972007269816,-379.220287241447));
#55196=CARTESIAN_POINT('',(453.615917770968,-273.972007269823,-384.220287241447));
#55197=CARTESIAN_POINT('',(453.615917770968,-273.972007269816,-379.220287241447));
#55198=CARTESIAN_POINT('Origin',(457.615917770968,-273.972007269823,-384.220287241447));
#55199=CARTESIAN_POINT('Origin',(453.615917770968,-305.972007269816,-379.220287241401));
#55200=CARTESIAN_POINT('',(453.615917770968,-297.972007269816,-379.220287241413));
#55201=CARTESIAN_POINT('',(453.615917770968,-297.972007269823,-384.220287241413));
#55202=CARTESIAN_POINT('Origin',(457.615917770968,-273.972007269816,-379.220287241447));
#55203=CARTESIAN_POINT('',(457.615917770945,-249.972007269814,-379.220287241482));
#55204=CARTESIAN_POINT('',(433.615917770966,-273.972007269756,-379.220287241447));
#55205=CARTESIAN_POINT('Origin',(457.615917770968,-273.972007269816,-379.220287241447));
#55206=CARTESIAN_POINT('',(457.615917770945,-249.972007269821,-384.220287241482));
#55207=CARTESIAN_POINT('',(457.615917770945,-249.972007269814,-379.220287241482));
#55208=CARTESIAN_POINT('',(433.615917770966,-273.972007269763,-384.220287241447));
#55209=CARTESIAN_POINT('Origin',(457.615917770968,-273.972007269823,-384.220287241447));
#55210=CARTESIAN_POINT('',(433.615917770966,-273.972007269756,-379.220287241447));
#55211=CARTESIAN_POINT('Origin',(433.615917770966,-305.972007269872,-379.220287241401));
#55212=CARTESIAN_POINT('',(433.615917770966,-305.972007269872,-379.220287241401));
#55213=CARTESIAN_POINT('',(433.615917770966,-273.972007269756,-379.220287241447));
#55214=CARTESIAN_POINT('',(433.615917770966,-305.972007269879,-384.220287241401));
#55215=CARTESIAN_POINT('',(433.615917770966,-273.972007269763,-384.220287241447));
#55216=CARTESIAN_POINT('',(433.615917770966,-305.972007269872,-379.220287241401));
#55217=CARTESIAN_POINT('Origin',(457.615917770968,-305.972007269816,-379.220287241401));
#55218=CARTESIAN_POINT('',(457.615917770945,-329.972007269817,-379.220287241366));
#55219=CARTESIAN_POINT('Origin',(457.615917770968,-305.972007269816,-379.220287241401));
#55220=CARTESIAN_POINT('',(457.615917770945,-329.972007269824,-384.220287241366));
#55221=CARTESIAN_POINT('Origin',(457.615917770968,-305.972007269823,-384.220287241401));
#55222=CARTESIAN_POINT('',(457.615917770945,-329.972007269817,-379.220287241366));
#55223=CARTESIAN_POINT('Origin',(489.615917770916,-329.972007269817,-379.220287241366));
#55224=CARTESIAN_POINT('',(489.615917770916,-329.972007269817,-379.220287241366));
#55225=CARTESIAN_POINT('',(457.615917770945,-329.972007269817,-379.220287241366));
#55226=CARTESIAN_POINT('',(489.615917770916,-329.972007269824,-384.220287241366));
#55227=CARTESIAN_POINT('',(457.615917770945,-329.972007269824,-384.220287241366));
#55228=CARTESIAN_POINT('',(489.615917770916,-329.972007269817,-379.220287241366));
#55229=CARTESIAN_POINT('Origin',(489.615917770968,-305.972007269816,-379.220287241401));
#55230=CARTESIAN_POINT('',(513.615917770969,-305.972007269872,-379.220287241401));
#55231=CARTESIAN_POINT('Origin',(489.615917770968,-305.972007269816,-379.220287241401));
#55232=CARTESIAN_POINT('',(513.615917770969,-305.972007269879,-384.220287241401));
#55233=CARTESIAN_POINT('Origin',(489.615917770968,-305.972007269823,-384.220287241401));
#55234=CARTESIAN_POINT('',(513.615917770969,-305.972007269872,-379.220287241401));
#55235=CARTESIAN_POINT('Origin',(513.615917770969,-273.972007269756,-379.220287241448));
#55236=CARTESIAN_POINT('',(513.615917770969,-273.972007269756,-379.220287241448));
#55237=CARTESIAN_POINT('',(513.615917770969,-305.972007269872,-379.220287241401));
#55238=CARTESIAN_POINT('',(513.615917770969,-273.972007269763,-384.220287241448));
#55239=CARTESIAN_POINT('',(513.615917770969,-305.972007269879,-384.220287241401));
#55240=CARTESIAN_POINT('',(513.615917770969,-273.972007269756,-379.220287241448));
#55241=CARTESIAN_POINT('Origin',(489.615917770968,-273.972007269816,-379.220287241448));
#55242=CARTESIAN_POINT('',(489.615917770916,-249.972007269814,-379.220287241482));
#55243=CARTESIAN_POINT('Origin',(489.615917770968,-273.972007269816,-379.220287241448));
#55244=CARTESIAN_POINT('',(489.615917770916,-249.972007269821,-384.220287241482));
#55245=CARTESIAN_POINT('Origin',(489.615917770968,-273.972007269823,-384.220287241448));
#55246=CARTESIAN_POINT('',(489.615917770916,-249.972007269814,-379.220287241482));
#55247=CARTESIAN_POINT('Origin',(457.615917770945,-249.972007269814,-379.220287241482));
#55248=CARTESIAN_POINT('',(489.615917770916,-249.972007269814,-379.220287241482));
#55249=CARTESIAN_POINT('',(489.615917770916,-249.972007269821,-384.220287241482));
#55250=CARTESIAN_POINT('Origin',(473.615917770965,-289.972007269816,-379.220287241424));
#55251=CARTESIAN_POINT('Origin',(473.615917770965,-289.972007269823,-384.220287241424));
#55252=CARTESIAN_POINT('',(0.,0.,0.));
#55253=CARTESIAN_POINT('',(0.,0.,0.));
#55254=CARTESIAN_POINT('Origin',(221.615917770968,-486.84465207658,486.500000551893));
#55255=CARTESIAN_POINT('',(221.615917770968,-100.47200726879,491.553000551893));
#55256=CARTESIAN_POINT('Origin',(221.615917770968,-100.47200726879,486.500000551893));
#55257=CARTESIAN_POINT('',(221.615917770968,-85.47200726879,491.553000551893));
#55258=CARTESIAN_POINT('',(221.615917770968,-486.84465207658,491.553000551893));
#55259=CARTESIAN_POINT('Origin',(221.615917770968,-85.47200726879,486.500000551893));
#55260=CARTESIAN_POINT('Origin',(221.615917770968,-486.84465207658,486.500000551893));
#55261=CARTESIAN_POINT('',(221.615917770968,-275.47200726879,491.553000551893));
#55262=CARTESIAN_POINT('Origin',(221.615917770968,-275.47200726879,486.500000551893));
#55263=CARTESIAN_POINT('',(221.615917770968,-260.47200726879,491.553000551893));
#55264=CARTESIAN_POINT('',(221.615917770968,-486.84465207658,491.553000551893));
#55265=CARTESIAN_POINT('Origin',(221.615917770968,-260.47200726879,486.500000551893));
#55266=CARTESIAN_POINT('Origin',(304.615917770968,-486.84465207658,403.500000551892));
#55267=CARTESIAN_POINT('',(304.615917770968,-100.47200726879,408.553000551893));
#55268=CARTESIAN_POINT('Origin',(304.615917770968,-100.47200726879,403.500000551893));
#55269=CARTESIAN_POINT('',(304.615917770968,-85.47200726879,408.553000551893));
#55270=CARTESIAN_POINT('',(304.615917770968,-486.84465207658,408.553000551892));
#55271=CARTESIAN_POINT('Origin',(304.615917770968,-85.47200726879,403.500000551893));
#55272=CARTESIAN_POINT('Origin',(304.615917770968,-486.84465207658,403.500000551892));
#55273=CARTESIAN_POINT('',(304.615917770968,-275.47200726879,408.553000551893));
#55274=CARTESIAN_POINT('Origin',(304.615917770968,-275.47200726879,403.500000551893));
#55275=CARTESIAN_POINT('',(304.615917770968,-260.47200726879,408.553000551893));
#55276=CARTESIAN_POINT('',(304.615917770968,-486.84465207658,408.553000551892));
#55277=CARTESIAN_POINT('Origin',(304.615917770968,-260.47200726879,403.500000551893));
#55278=CARTESIAN_POINT('Origin',(333.615917770968,-486.84465207658,486.500000551892));
#55279=CARTESIAN_POINT('',(333.615917770968,-100.47200726879,491.553000551893));
#55280=CARTESIAN_POINT('Origin',(333.615917770968,-100.47200726879,486.500000551893));
#55281=CARTESIAN_POINT('',(333.615917770969,-85.47200726879,491.553000551893));
#55282=CARTESIAN_POINT('',(333.615917770968,-486.84465207658,491.553000551892));
#55283=CARTESIAN_POINT('Origin',(333.615917770968,-85.4720072687901,486.500000551893));
#55284=CARTESIAN_POINT('Origin',(333.615917770968,-486.84465207658,486.500000551892));
#55285=CARTESIAN_POINT('',(333.615917770968,-275.47200726879,491.553000551893));
#55286=CARTESIAN_POINT('Origin',(333.615917770968,-275.47200726879,486.500000551893));
#55287=CARTESIAN_POINT('',(333.615917770968,-260.47200726879,491.553000551893));
#55288=CARTESIAN_POINT('',(333.615917770968,-486.84465207658,491.553000551892));
#55289=CARTESIAN_POINT('Origin',(333.615917770968,-260.47200726879,486.500000551893));
#55290=CARTESIAN_POINT('Origin',(416.615917770968,-486.84465207658,403.500000551892));
#55291=CARTESIAN_POINT('',(416.615917770968,-100.47200726879,408.553000551892));
#55292=CARTESIAN_POINT('Origin',(416.615917770968,-100.47200726879,403.500000551892));
#55293=CARTESIAN_POINT('',(416.615917770968,-85.4720072687901,408.553000551892));
#55294=CARTESIAN_POINT('',(416.615917770968,-486.84465207658,408.553000551892));
#55295=CARTESIAN_POINT('Origin',(416.615917770968,-85.47200726879,403.500000551892));
#55296=CARTESIAN_POINT('Origin',(416.615917770968,-486.84465207658,403.500000551892));
#55297=CARTESIAN_POINT('',(416.615917770968,-275.47200726879,408.553000551892));
#55298=CARTESIAN_POINT('Origin',(416.615917770968,-275.47200726879,403.500000551892));
#55299=CARTESIAN_POINT('',(416.615917770968,-260.47200726879,408.553000551892));
#55300=CARTESIAN_POINT('',(416.615917770968,-486.84465207658,408.553000551892));
#55301=CARTESIAN_POINT('Origin',(416.615917770968,-260.47200726879,403.500000551892));
#55302=CARTESIAN_POINT('Origin',(333.615917770968,-486.84465207658,403.500000551892));
#55303=CARTESIAN_POINT('',(333.615917770968,-100.47200726879,408.553000551893));
#55304=CARTESIAN_POINT('Origin',(333.615917770968,-100.47200726879,403.500000551893));
#55305=CARTESIAN_POINT('',(333.615917770968,-85.47200726879,408.553000551893));
#55306=CARTESIAN_POINT('',(333.615917770968,-486.84465207658,408.553000551892));
#55307=CARTESIAN_POINT('Origin',(333.615917770968,-85.47200726879,403.500000551893));
#55308=CARTESIAN_POINT('Origin',(333.615917770968,-486.84465207658,403.500000551892));
#55309=CARTESIAN_POINT('',(333.615917770968,-275.47200726879,408.553000551893));
#55310=CARTESIAN_POINT('Origin',(333.615917770968,-275.47200726879,403.500000551893));
#55311=CARTESIAN_POINT('',(333.615917770968,-260.47200726879,408.553000551893));
#55312=CARTESIAN_POINT('',(333.615917770968,-486.84465207658,408.553000551892));
#55313=CARTESIAN_POINT('Origin',(333.615917770968,-260.47200726879,403.500000551893));
#55314=CARTESIAN_POINT('Origin',(416.615917770968,-486.84465207658,486.500000551892));
#55315=CARTESIAN_POINT('',(416.615917770968,-100.47200726879,491.553000551892));
#55316=CARTESIAN_POINT('Origin',(416.615917770968,-100.47200726879,486.500000551892));
#55317=CARTESIAN_POINT('',(416.615917770968,-85.4720072687901,491.553000551892));
#55318=CARTESIAN_POINT('',(416.615917770968,-486.84465207658,491.553000551892));
#55319=CARTESIAN_POINT('Origin',(416.615917770968,-85.4720072687901,486.500000551892));
#55320=CARTESIAN_POINT('Origin',(416.615917770968,-486.84465207658,486.500000551892));
#55321=CARTESIAN_POINT('',(416.615917770968,-275.47200726879,491.553000551892));
#55322=CARTESIAN_POINT('Origin',(416.615917770968,-275.47200726879,486.500000551892));
#55323=CARTESIAN_POINT('',(416.615917770968,-260.47200726879,491.553000551892));
#55324=CARTESIAN_POINT('',(416.615917770968,-486.84465207658,491.553000551892));
#55325=CARTESIAN_POINT('Origin',(416.615917770968,-260.47200726879,486.500000551892));
#55326=CARTESIAN_POINT('Origin',(304.615917770968,-486.84465207658,486.500000551892));
#55327=CARTESIAN_POINT('',(304.615917770968,-100.47200726879,491.553000551893));
#55328=CARTESIAN_POINT('Origin',(304.615917770968,-100.47200726879,486.500000551893));
#55329=CARTESIAN_POINT('',(304.615917770968,-85.47200726879,491.553000551893));
#55330=CARTESIAN_POINT('',(304.615917770968,-486.84465207658,491.553000551892));
#55331=CARTESIAN_POINT('Origin',(304.615917770968,-85.4720072687901,486.500000551893));
#55332=CARTESIAN_POINT('Origin',(304.615917770968,-486.84465207658,486.500000551892));
#55333=CARTESIAN_POINT('',(304.615917770968,-275.47200726879,491.553000551893));
#55334=CARTESIAN_POINT('Origin',(304.615917770968,-275.47200726879,486.500000551893));
#55335=CARTESIAN_POINT('',(304.615917770968,-260.47200726879,491.553000551893));
#55336=CARTESIAN_POINT('',(304.615917770968,-486.84465207658,491.553000551892));
#55337=CARTESIAN_POINT('Origin',(304.615917770968,-260.47200726879,486.500000551893));
#55338=CARTESIAN_POINT('Origin',(221.615917770968,-486.84465207658,403.500000551893));
#55339=CARTESIAN_POINT('',(221.615917770968,-100.47200726879,408.553000551893));
#55340=CARTESIAN_POINT('Origin',(221.615917770968,-100.47200726879,403.500000551893));
#55341=CARTESIAN_POINT('',(221.615917770968,-85.47200726879,408.553000551893));
#55342=CARTESIAN_POINT('',(221.615917770968,-486.84465207658,408.553000551893));
#55343=CARTESIAN_POINT('Origin',(221.615917770968,-85.47200726879,403.500000551893));
#55344=CARTESIAN_POINT('Origin',(221.615917770968,-486.84465207658,403.500000551893));
#55345=CARTESIAN_POINT('',(221.615917770968,-275.47200726879,408.553000551893));
#55346=CARTESIAN_POINT('Origin',(221.615917770968,-275.47200726879,403.500000551893));
#55347=CARTESIAN_POINT('',(221.615917770968,-260.47200726879,408.553000551893));
#55348=CARTESIAN_POINT('',(221.615917770968,-486.84465207658,408.553000551893));
#55349=CARTESIAN_POINT('Origin',(221.615917770968,-260.47200726879,403.500000551893));
#55350=CARTESIAN_POINT('Origin',(459.115917770997,-260.47200726879,445.000000551892));
#55351=CARTESIAN_POINT('',(179.115917770997,-260.47200726879,360.000000551893));
#55352=CARTESIAN_POINT('',(179.115917770997,-260.47200726879,530.000000551893));
#55353=CARTESIAN_POINT('',(179.115917770997,-260.47200726879,445.000000551893));
#55354=CARTESIAN_POINT('',(459.115917770997,-260.47200726879,530.000000551892));
#55355=CARTESIAN_POINT('',(389.115917770983,-260.47200726879,530.000000551892));
#55356=CARTESIAN_POINT('',(459.115917770997,-260.47200726879,360.000000551892));
#55357=CARTESIAN_POINT('',(459.115917770997,-260.47200726879,445.000000551892));
#55358=CARTESIAN_POINT('',(389.115917770982,-260.47200726879,360.000000551892));
#55359=CARTESIAN_POINT('Origin',(459.115917770997,-100.47200726879,445.000000551892));
#55360=CARTESIAN_POINT('',(459.115917770997,-100.47200726879,530.000000551892));
#55361=CARTESIAN_POINT('',(459.115917770997,-140.47200726879,530.000000551892));
#55362=CARTESIAN_POINT('',(459.115917770997,-100.47200726879,360.000000551892));
#55363=CARTESIAN_POINT('',(459.115917770997,-100.47200726879,445.000000551892));
#55364=CARTESIAN_POINT('',(459.115917770997,-140.47200726879,360.000000551892));
#55365=CARTESIAN_POINT('Origin',(179.115917770997,-100.47200726879,445.000000551894));
#55366=CARTESIAN_POINT('',(179.115917770997,-100.47200726879,530.000000551894));
#55367=CARTESIAN_POINT('',(249.115917770983,-100.47200726879,530.000000551893));
#55368=CARTESIAN_POINT('',(179.115917770997,-100.47200726879,360.000000551894));
#55369=CARTESIAN_POINT('',(179.115917770997,-100.47200726879,445.000000551894));
#55370=CARTESIAN_POINT('',(249.115917770982,-100.47200726879,360.000000551893));
#55371=CARTESIAN_POINT('Origin',(179.115917770997,-260.47200726879,445.000000551893));
#55372=CARTESIAN_POINT('',(179.115917770997,-220.47200726879,530.000000551893));
#55373=CARTESIAN_POINT('',(179.115917770997,-220.47200726879,360.000000551893));
#55374=CARTESIAN_POINT('Origin',(319.115917770969,-180.47200726879,530.000000551893));
#55375=CARTESIAN_POINT('',(164.115917770969,-85.4720072687901,530.000000551894));
#55376=CARTESIAN_POINT('',(164.115917770969,-275.47200726879,530.000000551893));
#55377=CARTESIAN_POINT('',(164.115917770969,-275.47200726879,530.000000551893));
#55378=CARTESIAN_POINT('',(474.115917770968,-275.47200726879,530.000000551892));
#55379=CARTESIAN_POINT('',(474.115917770968,-275.47200726879,530.000000551892));
#55380=CARTESIAN_POINT('',(474.115917770969,-85.4720072687902,530.000000551892));
#55381=CARTESIAN_POINT('',(474.115917770969,-85.4720072687902,530.000000551892));
#55382=CARTESIAN_POINT('',(164.115917770969,-85.4720072687901,530.000000551894));
#55383=CARTESIAN_POINT('Origin',(474.115917770968,-275.47200726879,445.000000551892));
#55384=CARTESIAN_POINT('',(164.115917770968,-275.47200726879,360.000000551893));
#55385=CARTESIAN_POINT('',(164.115917770968,-275.47200726879,445.000000551893));
#55386=CARTESIAN_POINT('',(474.115917770968,-275.47200726879,360.000000551892));
#55387=CARTESIAN_POINT('',(474.115917770968,-275.47200726879,360.000000551892));
#55388=CARTESIAN_POINT('',(474.115917770968,-275.47200726879,445.000000551892));
#55389=CARTESIAN_POINT('Origin',(474.115917770968,-85.4720072687901,445.000000551892));
#55390=CARTESIAN_POINT('',(474.115917770968,-85.47200726879,360.000000551892));
#55391=CARTESIAN_POINT('',(474.115917770968,-85.47200726879,360.000000551892));
#55392=CARTESIAN_POINT('',(474.115917770968,-85.4720072687901,445.000000551892));
#55393=CARTESIAN_POINT('Origin',(164.115917770968,-85.47200726879,445.000000551894));
#55394=CARTESIAN_POINT('',(164.115917770968,-85.4720072687899,360.000000551894));
#55395=CARTESIAN_POINT('',(164.115917770968,-85.4720072687899,360.000000551894));
#55396=CARTESIAN_POINT('',(164.115917770968,-85.47200726879,445.000000551894));
#55397=CARTESIAN_POINT('Origin',(164.115917770968,-275.47200726879,445.000000551893));
#55398=CARTESIAN_POINT('',(164.115917770968,-275.47200726879,360.000000551893));
#55399=CARTESIAN_POINT('Origin',(319.115917770968,-180.47200726879,360.000000551893));
#55400=CARTESIAN_POINT('',(0.,0.,0.));
#55401=CARTESIAN_POINT('Origin',(179.115917770968,-85.4720072687897,360.000000551894));
#55402=CARTESIAN_POINT('',(179.115917770968,-100.47200726879,530.000000551894));
#55403=CARTESIAN_POINT('',(179.115917770968,-100.47200726879,360.000000551894));
#55404=CARTESIAN_POINT('',(179.115917770968,-100.47200726879,402.500000551894));
#55405=CARTESIAN_POINT('',(179.115917770968,-85.4720072687903,530.000000551894));
#55406=CARTESIAN_POINT('',(179.115917770968,-89.2220072687903,530.000000551894));
#55407=CARTESIAN_POINT('',(179.115917770968,-85.4720072687897,360.000000551894));
#55408=CARTESIAN_POINT('',(179.115917770968,-85.4720072687898,402.500000551894));
#55409=CARTESIAN_POINT('',(179.115917770968,-89.2220072687897,360.000000551894));
#55410=CARTESIAN_POINT('',(179.115917770968,-88.7840072687902,510.000000551894));
#55411=CARTESIAN_POINT('Origin',(179.115917770968,-92.9720072687902,510.000000551894));
#55412=CARTESIAN_POINT('',(179.115917770968,-88.7840072687899,445.000000551894));
#55413=CARTESIAN_POINT('Origin',(179.115917770968,-92.97200726879,445.000000551894));
#55414=CARTESIAN_POINT('',(179.115917770968,-88.7840072687897,380.000000551894));
#55415=CARTESIAN_POINT('Origin',(179.115917770968,-92.9720072687898,380.000000551894));
#55416=CARTESIAN_POINT('Origin',(459.115917770968,-85.4720072687904,530.000000551893));
#55417=CARTESIAN_POINT('',(459.115917770968,-100.47200726879,360.000000551893));
#55418=CARTESIAN_POINT('',(459.115917770968,-100.47200726879,530.000000551893));
#55419=CARTESIAN_POINT('',(459.115917770968,-100.47200726879,487.500000551893));
#55420=CARTESIAN_POINT('',(459.115917770968,-85.4720072687898,360.000000551893));
#55421=CARTESIAN_POINT('',(459.115917770968,-89.2220072687898,360.000000551893));
#55422=CARTESIAN_POINT('',(459.115917770968,-85.4720072687904,530.000000551893));
#55423=CARTESIAN_POINT('',(459.115917770968,-85.4720072687903,487.500000551893));
#55424=CARTESIAN_POINT('',(459.115917770968,-89.2220072687904,530.000000551893));
#55425=CARTESIAN_POINT('',(459.115917770968,-88.7840072687903,510.000000551893));
#55426=CARTESIAN_POINT('Origin',(459.115917770968,-92.9720072687903,510.000000551893));
#55427=CARTESIAN_POINT('',(459.115917770968,-88.7840072687901,445.000000551893));
#55428=CARTESIAN_POINT('Origin',(459.115917770968,-92.9720072687901,445.000000551893));
#55429=CARTESIAN_POINT('',(459.115917770968,-88.7840072687899,380.000000551893));
#55430=CARTESIAN_POINT('Origin',(459.115917770968,-92.9720072687899,380.000000551893));
#55431=CARTESIAN_POINT('Origin',(164.115917770968,-92.9720072687902,530.000000551894));
#55432=CARTESIAN_POINT('',(474.115917770968,-100.47200726879,530.000000551893));
#55433=CARTESIAN_POINT('',(474.115917770968,-85.4720072687904,530.000000551893));
#55434=CARTESIAN_POINT('Origin',(432.857715634724,-92.9720072687903,510.000000551893));
#55435=CARTESIAN_POINT('',(431.599513498481,-92.9720072687903,510.000000551893));
#55436=CARTESIAN_POINT('',(434.115917770968,-88.7840072687902,510.000000551893));
#55437=CARTESIAN_POINT('',(432.857715634724,-90.8780072687903,510.000000551893));
#55438=CARTESIAN_POINT('Origin',(434.115917770968,-92.9720072687903,510.000000551893));
#55439=CARTESIAN_POINT('Origin',(454.115917770968,-92.9720072687903,510.000000551893));
#55440=CARTESIAN_POINT('',(454.115917770968,-88.7840072687903,510.000000551893));
#55441=CARTESIAN_POINT('Origin',(432.857715634724,-92.9720072687901,445.000000551893));
#55442=CARTESIAN_POINT('',(431.599513498481,-92.9720072687901,445.000000551893));
#55443=CARTESIAN_POINT('',(434.115917770968,-88.78400726879,445.000000551893));
#55444=CARTESIAN_POINT('',(432.857715634724,-90.8780072687901,445.000000551893));
#55445=CARTESIAN_POINT('Origin',(434.115917770968,-92.9720072687901,445.000000551893));
#55446=CARTESIAN_POINT('Origin',(454.115917770968,-92.9720072687901,445.000000551893));
#55447=CARTESIAN_POINT('',(454.115917770968,-88.7840072687901,445.000000551893));
#55448=CARTESIAN_POINT('Origin',(432.857715634724,-92.9720072687899,380.000000551893));
#55449=CARTESIAN_POINT('',(431.59951349848,-92.9720072687899,380.000000551893));
#55450=CARTESIAN_POINT('',(434.115917770968,-88.7840072687898,380.000000551893));
#55451=CARTESIAN_POINT('',(432.857715634724,-90.8780072687899,380.000000551893));
#55452=CARTESIAN_POINT('Origin',(434.115917770968,-92.9720072687899,380.000000551893));
#55453=CARTESIAN_POINT('Origin',(454.115917770968,-92.9720072687899,380.000000551893));
#55454=CARTESIAN_POINT('',(454.115917770968,-88.7840072687899,380.000000551893));
#55455=CARTESIAN_POINT('Origin',(205.374119907212,-92.9720072687902,510.000000551894));
#55456=CARTESIAN_POINT('',(206.632322043456,-92.9720072687902,510.000000551894));
#55457=CARTESIAN_POINT('',(204.115917770968,-88.7840072687901,510.000000551894));
#55458=CARTESIAN_POINT('',(205.374119907212,-90.8780072687902,510.000000551894));
#55459=CARTESIAN_POINT('Origin',(204.115917770968,-92.9720072687902,510.000000551894));
#55460=CARTESIAN_POINT('Origin',(184.115917770968,-92.9720072687902,510.000000551894));
#55461=CARTESIAN_POINT('',(184.115917770968,-88.7840072687902,510.000000551894));
#55462=CARTESIAN_POINT('Origin',(205.374119907212,-92.97200726879,445.000000551894));
#55463=CARTESIAN_POINT('',(206.632322043456,-92.97200726879,445.000000551894));
#55464=CARTESIAN_POINT('',(204.115917770968,-88.7840072687898,445.000000551894));
#55465=CARTESIAN_POINT('',(205.374119907212,-90.87800726879,445.000000551894));
#55466=CARTESIAN_POINT('Origin',(204.115917770968,-92.97200726879,445.000000551894));
#55467=CARTESIAN_POINT('Origin',(184.115917770968,-92.97200726879,445.000000551894));
#55468=CARTESIAN_POINT('',(184.115917770968,-88.78400726879,445.000000551894));
#55469=CARTESIAN_POINT('Origin',(205.374119907212,-92.9720072687898,380.000000551894));
#55470=CARTESIAN_POINT('',(206.632322043455,-92.9720072687898,380.000000551894));
#55471=CARTESIAN_POINT('',(204.115917770968,-88.7840072687896,380.000000551894));
#55472=CARTESIAN_POINT('',(205.374119907212,-90.8780072687897,380.000000551894));
#55473=CARTESIAN_POINT('Origin',(204.115917770968,-92.9720072687898,380.000000551894));
#55474=CARTESIAN_POINT('Origin',(184.115917770968,-92.9720072687898,380.000000551894));
#55475=CARTESIAN_POINT('',(184.115917770968,-88.7840072687898,380.000000551894));
#55476=CARTESIAN_POINT('Origin',(221.615917770968,-84.8220072687901,486.500000551894));
#55477=CARTESIAN_POINT('',(226.803917770968,-85.4720072687901,486.500000551894));
#55478=CARTESIAN_POINT('Origin',(221.615917770968,-85.4720072687901,486.500000551894));
#55479=CARTESIAN_POINT('',(226.803917770968,-100.47200726879,486.500000551894));
#55480=CARTESIAN_POINT('',(226.803917770968,-84.8220072687901,486.500000551894));
#55481=CARTESIAN_POINT('Origin',(221.615917770968,-100.47200726879,486.500000551894));
#55482=CARTESIAN_POINT('Origin',(333.615917770968,-84.8220072687899,403.500000551893));
#55483=CARTESIAN_POINT('',(338.803917770968,-85.4720072687899,403.500000551893));
#55484=CARTESIAN_POINT('Origin',(333.615917770968,-85.4720072687899,403.500000551893));
#55485=CARTESIAN_POINT('',(338.803917770968,-100.47200726879,403.500000551893));
#55486=CARTESIAN_POINT('',(338.803917770968,-84.8220072687899,403.500000551893));
#55487=CARTESIAN_POINT('Origin',(333.615917770968,-100.47200726879,403.500000551893));
#55488=CARTESIAN_POINT('Origin',(333.615917770968,-84.8220072687902,486.500000551893));
#55489=CARTESIAN_POINT('',(338.803917770968,-85.4720072687902,486.500000551893));
#55490=CARTESIAN_POINT('Origin',(333.615917770968,-85.4720072687902,486.500000551893));
#55491=CARTESIAN_POINT('',(338.803917770968,-100.47200726879,486.500000551893));
#55492=CARTESIAN_POINT('',(338.803917770968,-84.8220072687902,486.500000551893));
#55493=CARTESIAN_POINT('Origin',(333.615917770968,-100.47200726879,486.500000551893));
#55494=CARTESIAN_POINT('Origin',(416.615917770968,-84.8220072687902,486.500000551893));
#55495=CARTESIAN_POINT('',(421.803917770968,-85.4720072687902,486.500000551893));
#55496=CARTESIAN_POINT('Origin',(416.615917770968,-85.4720072687902,486.500000551893));
#55497=CARTESIAN_POINT('',(421.803917770968,-100.47200726879,486.500000551893));
#55498=CARTESIAN_POINT('',(421.803917770968,-84.8220072687902,486.500000551893));
#55499=CARTESIAN_POINT('Origin',(416.615917770968,-100.47200726879,486.500000551893));
#55500=CARTESIAN_POINT('Origin',(416.615917770968,-84.8220072687899,403.500000551893));
#55501=CARTESIAN_POINT('',(421.803917770968,-85.47200726879,403.500000551893));
#55502=CARTESIAN_POINT('Origin',(416.615917770968,-85.47200726879,403.500000551893));
#55503=CARTESIAN_POINT('',(421.803917770968,-100.47200726879,403.500000551893));
#55504=CARTESIAN_POINT('',(421.803917770968,-84.8220072687899,403.500000551893));
#55505=CARTESIAN_POINT('Origin',(416.615917770968,-100.47200726879,403.500000551893));
#55506=CARTESIAN_POINT('Origin',(304.615917770968,-84.8220072687902,486.500000551893));
#55507=CARTESIAN_POINT('',(309.803917770968,-85.4720072687902,486.500000551893));
#55508=CARTESIAN_POINT('Origin',(304.615917770968,-85.4720072687902,486.500000551893));
#55509=CARTESIAN_POINT('',(309.803917770968,-100.47200726879,486.500000551893));
#55510=CARTESIAN_POINT('',(309.803917770968,-84.8220072687902,486.500000551893));
#55511=CARTESIAN_POINT('Origin',(304.615917770968,-100.47200726879,486.500000551893));
#55512=CARTESIAN_POINT('Origin',(304.615917770968,-84.8220072687899,403.500000551893));
#55513=CARTESIAN_POINT('',(309.803917770968,-85.4720072687899,403.500000551893));
#55514=CARTESIAN_POINT('Origin',(304.615917770968,-85.4720072687899,403.500000551893));
#55515=CARTESIAN_POINT('',(309.803917770968,-100.47200726879,403.500000551893));
#55516=CARTESIAN_POINT('',(309.803917770968,-84.8220072687899,403.500000551893));
#55517=CARTESIAN_POINT('Origin',(304.615917770968,-100.47200726879,403.500000551893));
#55518=CARTESIAN_POINT('Origin',(221.615917770968,-84.8220072687898,403.500000551894));
#55519=CARTESIAN_POINT('',(226.803917770968,-85.4720072687898,403.500000551894));
#55520=CARTESIAN_POINT('Origin',(221.615917770968,-85.4720072687898,403.500000551894));
#55521=CARTESIAN_POINT('',(226.803917770968,-100.47200726879,403.500000551893));
#55522=CARTESIAN_POINT('',(226.803917770968,-84.8220072687898,403.500000551894));
#55523=CARTESIAN_POINT('Origin',(221.615917770968,-100.47200726879,403.500000551894));
#55524=CARTESIAN_POINT('Origin',(375.115917770968,-100.47200726879,445.000000551893));
#55525=CARTESIAN_POINT('',(355.115917770968,-100.47200726879,445.000000551893));
#55526=CARTESIAN_POINT('Origin',(375.115917770968,-100.47200726879,445.000000551893));
#55527=CARTESIAN_POINT('',(355.115917770968,-85.4720072687901,445.000000551893));
#55528=CARTESIAN_POINT('',(355.115917770968,-100.47200726879,445.000000551893));
#55529=CARTESIAN_POINT('Origin',(375.115917770968,-85.4720072687901,445.000000551893));
#55530=CARTESIAN_POINT('Origin',(263.115917770968,-100.47200726879,445.000000551893));
#55531=CARTESIAN_POINT('',(243.115917770968,-100.47200726879,445.000000551893));
#55532=CARTESIAN_POINT('Origin',(263.115917770968,-100.47200726879,445.000000551893));
#55533=CARTESIAN_POINT('',(243.115917770968,-85.47200726879,445.000000551893));
#55534=CARTESIAN_POINT('',(243.115917770968,-100.47200726879,445.000000551893));
#55535=CARTESIAN_POINT('Origin',(263.115917770968,-85.47200726879,445.000000551893));
#55536=CARTESIAN_POINT('Origin',(319.115917770968,-100.47200726879,445.000000551893));
#55537=CARTESIAN_POINT('',(164.115917770968,-100.47200726879,360.000000551894));
#55538=CARTESIAN_POINT('Origin',(474.115917770968,-92.9720072687898,360.000000551893));
#55539=CARTESIAN_POINT('',(164.115917770968,-85.4720072687897,360.000000551894));
#55540=CARTESIAN_POINT('Origin',(319.115917770968,-85.47200726879,445.000000551893));
#55541=CARTESIAN_POINT('',(0.,0.,0.));
#55542=CARTESIAN_POINT('Origin',(459.115917770968,-260.47200726879,530.000000551893));
#55543=CARTESIAN_POINT('',(459.115917770968,-275.47200726879,360.000000551893));
#55544=CARTESIAN_POINT('',(459.115917770968,-275.47200726879,530.000000551893));
#55545=CARTESIAN_POINT('',(459.115917770968,-275.47200726879,487.500000551892));
#55546=CARTESIAN_POINT('',(459.115917770968,-260.47200726879,360.000000551893));
#55547=CARTESIAN_POINT('',(459.115917770968,-264.22200726879,360.000000551892));
#55548=CARTESIAN_POINT('',(459.115917770968,-260.47200726879,530.000000551893));
#55549=CARTESIAN_POINT('',(459.115917770968,-260.47200726879,487.500000551892));
#55550=CARTESIAN_POINT('',(459.115917770968,-264.22200726879,530.000000551892));
#55551=CARTESIAN_POINT('',(459.115917770968,-263.78400726879,510.000000551892));
#55552=CARTESIAN_POINT('Origin',(459.115917770968,-267.97200726879,510.000000551892));
#55553=CARTESIAN_POINT('',(459.115917770968,-263.78400726879,445.000000551892));
#55554=CARTESIAN_POINT('Origin',(459.115917770968,-267.97200726879,445.000000551892));
#55555=CARTESIAN_POINT('',(459.115917770968,-263.78400726879,380.000000551892));
#55556=CARTESIAN_POINT('Origin',(459.115917770968,-267.97200726879,380.000000551892));
#55557=CARTESIAN_POINT('Origin',(179.115917770968,-260.47200726879,360.000000551894));
#55558=CARTESIAN_POINT('',(179.115917770968,-275.47200726879,530.000000551894));
#55559=CARTESIAN_POINT('',(179.115917770968,-275.47200726879,360.000000551894));
#55560=CARTESIAN_POINT('',(179.115917770968,-275.47200726879,402.500000551894));
#55561=CARTESIAN_POINT('',(179.115917770968,-260.47200726879,530.000000551894));
#55562=CARTESIAN_POINT('',(179.115917770968,-264.22200726879,530.000000551894));
#55563=CARTESIAN_POINT('',(179.115917770968,-260.47200726879,360.000000551894));
#55564=CARTESIAN_POINT('',(179.115917770968,-260.47200726879,402.500000551894));
#55565=CARTESIAN_POINT('',(179.115917770968,-264.22200726879,360.000000551894));
#55566=CARTESIAN_POINT('',(179.115917770968,-263.78400726879,380.000000551894));
#55567=CARTESIAN_POINT('Origin',(179.115917770968,-267.97200726879,380.000000551894));
#55568=CARTESIAN_POINT('',(179.115917770968,-263.78400726879,445.000000551894));
#55569=CARTESIAN_POINT('Origin',(179.115917770968,-267.97200726879,445.000000551894));
#55570=CARTESIAN_POINT('',(179.115917770968,-263.78400726879,510.000000551894));
#55571=CARTESIAN_POINT('Origin',(179.115917770968,-267.97200726879,510.000000551894));
#55572=CARTESIAN_POINT('Origin',(474.115917770967,-267.97200726879,360.000000551892));
#55573=CARTESIAN_POINT('',(164.115917770968,-275.47200726879,360.000000551894));
#55574=CARTESIAN_POINT('',(164.115917770968,-260.47200726879,360.000000551894));
#55575=CARTESIAN_POINT('Origin',(445.557715634724,-267.97200726879,510.000000551892));
#55576=CARTESIAN_POINT('',(444.299513498481,-267.97200726879,510.000000551892));
#55577=CARTESIAN_POINT('',(446.815917770968,-263.78400726879,510.000000551892));
#55578=CARTESIAN_POINT('',(445.557715634724,-265.87800726879,510.000000551892));
#55579=CARTESIAN_POINT('Origin',(446.815917770968,-267.97200726879,510.000000551892));
#55580=CARTESIAN_POINT('Origin',(460.465917770968,-267.97200726879,510.000000551892));
#55581=CARTESIAN_POINT('',(460.465917770968,-263.78400726879,510.000000551892));
#55582=CARTESIAN_POINT('Origin',(445.557715634724,-267.97200726879,445.000000551892));
#55583=CARTESIAN_POINT('',(444.29951349848,-267.97200726879,445.000000551892));
#55584=CARTESIAN_POINT('',(446.815917770968,-263.78400726879,445.000000551892));
#55585=CARTESIAN_POINT('',(445.557715634724,-265.87800726879,445.000000551892));
#55586=CARTESIAN_POINT('Origin',(446.815917770968,-267.97200726879,445.000000551892));
#55587=CARTESIAN_POINT('Origin',(460.465917770968,-267.97200726879,445.000000551892));
#55588=CARTESIAN_POINT('',(460.465917770968,-263.78400726879,445.000000551892));
#55589=CARTESIAN_POINT('Origin',(445.557715634724,-267.97200726879,380.000000551892));
#55590=CARTESIAN_POINT('',(444.29951349848,-267.97200726879,380.000000551892));
#55591=CARTESIAN_POINT('',(446.815917770968,-263.78400726879,380.000000551892));
#55592=CARTESIAN_POINT('',(445.557715634724,-265.87800726879,380.000000551892));
#55593=CARTESIAN_POINT('Origin',(446.815917770968,-267.97200726879,380.000000551892));
#55594=CARTESIAN_POINT('Origin',(460.465917770968,-267.97200726879,380.000000551892));
#55595=CARTESIAN_POINT('',(460.465917770968,-263.78400726879,380.000000551892));
#55596=CARTESIAN_POINT('Origin',(192.674119907212,-267.97200726879,510.000000551894));
#55597=CARTESIAN_POINT('',(193.932322043456,-267.97200726879,510.000000551894));
#55598=CARTESIAN_POINT('',(191.415917770968,-263.78400726879,510.000000551894));
#55599=CARTESIAN_POINT('',(192.674119907212,-265.87800726879,510.000000551894));
#55600=CARTESIAN_POINT('Origin',(191.415917770968,-267.97200726879,510.000000551894));
#55601=CARTESIAN_POINT('Origin',(177.765917770968,-267.97200726879,510.000000551894));
#55602=CARTESIAN_POINT('',(177.765917770968,-263.78400726879,510.000000551894));
#55603=CARTESIAN_POINT('Origin',(192.674119907212,-267.97200726879,445.000000551894));
#55604=CARTESIAN_POINT('',(193.932322043456,-267.97200726879,445.000000551894));
#55605=CARTESIAN_POINT('',(191.415917770968,-263.78400726879,445.000000551894));
#55606=CARTESIAN_POINT('',(192.674119907212,-265.87800726879,445.000000551894));
#55607=CARTESIAN_POINT('Origin',(191.415917770968,-267.97200726879,445.000000551894));
#55608=CARTESIAN_POINT('Origin',(177.765917770968,-267.97200726879,445.000000551894));
#55609=CARTESIAN_POINT('',(177.765917770968,-263.78400726879,445.000000551894));
#55610=CARTESIAN_POINT('Origin',(192.674119907212,-267.97200726879,380.000000551894));
#55611=CARTESIAN_POINT('',(193.932322043455,-267.97200726879,380.000000551894));
#55612=CARTESIAN_POINT('',(191.415917770968,-263.78400726879,380.000000551894));
#55613=CARTESIAN_POINT('',(192.674119907212,-265.87800726879,380.000000551894));
#55614=CARTESIAN_POINT('Origin',(191.415917770968,-267.97200726879,380.000000551894));
#55615=CARTESIAN_POINT('Origin',(177.765917770968,-267.97200726879,380.000000551894));
#55616=CARTESIAN_POINT('',(177.765917770968,-263.78400726879,380.000000551894));
#55617=CARTESIAN_POINT('Origin',(221.615917770968,-259.82200726879,486.500000551893));
#55618=CARTESIAN_POINT('',(226.803917770968,-260.47200726879,486.500000551893));
#55619=CARTESIAN_POINT('Origin',(221.615917770968,-260.47200726879,486.500000551893));
#55620=CARTESIAN_POINT('',(226.803917770968,-275.47200726879,486.500000551893));
#55621=CARTESIAN_POINT('',(226.803917770968,-259.82200726879,486.500000551893));
#55622=CARTESIAN_POINT('Origin',(221.615917770968,-275.47200726879,486.500000551893));
#55623=CARTESIAN_POINT('Origin',(333.615917770968,-259.82200726879,403.500000551893));
#55624=CARTESIAN_POINT('',(338.803917770968,-260.47200726879,403.500000551893));
#55625=CARTESIAN_POINT('Origin',(333.615917770968,-260.47200726879,403.500000551893));
#55626=CARTESIAN_POINT('',(338.803917770968,-275.47200726879,403.500000551893));
#55627=CARTESIAN_POINT('',(338.803917770968,-259.82200726879,403.500000551893));
#55628=CARTESIAN_POINT('Origin',(333.615917770968,-275.47200726879,403.500000551893));
#55629=CARTESIAN_POINT('Origin',(333.615917770968,-259.82200726879,486.500000551893));
#55630=CARTESIAN_POINT('',(338.803917770968,-260.47200726879,486.500000551893));
#55631=CARTESIAN_POINT('Origin',(333.615917770968,-260.47200726879,486.500000551893));
#55632=CARTESIAN_POINT('',(338.803917770968,-275.47200726879,486.500000551893));
#55633=CARTESIAN_POINT('',(338.803917770968,-259.82200726879,486.500000551893));
#55634=CARTESIAN_POINT('Origin',(333.615917770968,-275.47200726879,486.500000551893));
#55635=CARTESIAN_POINT('Origin',(416.615917770968,-259.82200726879,486.500000551892));
#55636=CARTESIAN_POINT('',(421.803917770968,-260.47200726879,486.500000551892));
#55637=CARTESIAN_POINT('Origin',(416.615917770968,-260.47200726879,486.500000551892));
#55638=CARTESIAN_POINT('',(421.803917770968,-275.47200726879,486.500000551892));
#55639=CARTESIAN_POINT('',(421.803917770968,-259.82200726879,486.500000551892));
#55640=CARTESIAN_POINT('Origin',(416.615917770968,-275.47200726879,486.500000551892));
#55641=CARTESIAN_POINT('Origin',(416.615917770968,-259.82200726879,403.500000551892));
#55642=CARTESIAN_POINT('',(421.803917770968,-260.47200726879,403.500000551892));
#55643=CARTESIAN_POINT('Origin',(416.615917770968,-260.47200726879,403.500000551892));
#55644=CARTESIAN_POINT('',(421.803917770968,-275.47200726879,403.500000551892));
#55645=CARTESIAN_POINT('',(421.803917770968,-259.82200726879,403.500000551892));
#55646=CARTESIAN_POINT('Origin',(416.615917770968,-275.47200726879,403.500000551892));
#55647=CARTESIAN_POINT('Origin',(304.615917770968,-259.82200726879,486.500000551893));
#55648=CARTESIAN_POINT('',(309.803917770968,-260.47200726879,486.500000551893));
#55649=CARTESIAN_POINT('Origin',(304.615917770968,-260.47200726879,486.500000551893));
#55650=CARTESIAN_POINT('',(309.803917770968,-275.47200726879,486.500000551893));
#55651=CARTESIAN_POINT('',(309.803917770968,-259.82200726879,486.500000551893));
#55652=CARTESIAN_POINT('Origin',(304.615917770968,-275.47200726879,486.500000551893));
#55653=CARTESIAN_POINT('Origin',(304.615917770968,-259.82200726879,403.500000551893));
#55654=CARTESIAN_POINT('',(309.803917770968,-260.47200726879,403.500000551893));
#55655=CARTESIAN_POINT('Origin',(304.615917770968,-260.47200726879,403.500000551893));
#55656=CARTESIAN_POINT('',(309.803917770968,-275.47200726879,403.500000551893));
#55657=CARTESIAN_POINT('',(309.803917770968,-259.82200726879,403.500000551893));
#55658=CARTESIAN_POINT('Origin',(304.615917770968,-275.47200726879,403.500000551893));
#55659=CARTESIAN_POINT('Origin',(221.615917770968,-259.82200726879,403.500000551893));
#55660=CARTESIAN_POINT('',(226.803917770968,-260.47200726879,403.500000551893));
#55661=CARTESIAN_POINT('Origin',(221.615917770968,-260.47200726879,403.500000551893));
#55662=CARTESIAN_POINT('',(226.803917770968,-275.47200726879,403.500000551893));
#55663=CARTESIAN_POINT('',(226.803917770968,-259.82200726879,403.500000551893));
#55664=CARTESIAN_POINT('Origin',(221.615917770968,-275.47200726879,403.500000551893));
#55665=CARTESIAN_POINT('Origin',(375.115917770968,-275.47200726879,445.000000551892));
#55666=CARTESIAN_POINT('',(355.115917770968,-275.47200726879,445.000000551892));
#55667=CARTESIAN_POINT('Origin',(375.115917770968,-275.47200726879,445.000000551892));
#55668=CARTESIAN_POINT('',(355.115917770968,-260.47200726879,445.000000551892));
#55669=CARTESIAN_POINT('',(355.115917770968,-275.47200726879,445.000000551892));
#55670=CARTESIAN_POINT('Origin',(375.115917770968,-260.47200726879,445.000000551892));
#55671=CARTESIAN_POINT('Origin',(263.115917770968,-275.47200726879,445.000000551893));
#55672=CARTESIAN_POINT('',(243.115917770968,-275.47200726879,445.000000551893));
#55673=CARTESIAN_POINT('Origin',(263.115917770968,-275.47200726879,445.000000551893));
#55674=CARTESIAN_POINT('',(243.115917770968,-260.47200726879,445.000000551893));
#55675=CARTESIAN_POINT('',(243.115917770968,-275.47200726879,445.000000551893));
#55676=CARTESIAN_POINT('Origin',(263.115917770968,-260.47200726879,445.000000551893));
#55677=CARTESIAN_POINT('Origin',(319.115917770968,-275.47200726879,445.000000551893));
#55678=CARTESIAN_POINT('',(474.115917770968,-275.47200726879,530.000000551892));
#55679=CARTESIAN_POINT('Origin',(164.115917770968,-267.97200726879,530.000000551894));
#55680=CARTESIAN_POINT('',(474.115917770968,-260.47200726879,530.000000551892));
#55681=CARTESIAN_POINT('Origin',(319.115917770968,-260.47200726879,445.000000551893));
#55682=CARTESIAN_POINT('',(0.,0.,0.));
#55683=CARTESIAN_POINT('Origin',(195.682801924451,-267.97200726879,445.000000551899));
#55684=CARTESIAN_POINT('',(459.115917770968,-267.97200726879,450.500000551898));
#55685=CARTESIAN_POINT('Origin',(459.115917770968,-267.97200726879,445.000000551898));
#55686=CARTESIAN_POINT('',(474.115917770968,-267.97200726879,450.500000551898));
#55687=CARTESIAN_POINT('',(195.682801924451,-267.97200726879,450.500000551899));
#55688=CARTESIAN_POINT('Origin',(474.115917770968,-267.97200726879,445.000000551898));
#55689=CARTESIAN_POINT('Origin',(195.682801924451,-92.9720072687897,380.0000005519));
#55690=CARTESIAN_POINT('',(459.115917770968,-92.9720072687899,385.500000551899));
#55691=CARTESIAN_POINT('Origin',(459.115917770968,-92.9720072687899,380.000000551899));
#55692=CARTESIAN_POINT('',(474.115917770968,-92.9720072687899,385.500000551898));
#55693=CARTESIAN_POINT('',(195.682801924451,-92.9720072687898,385.5000005519));
#55694=CARTESIAN_POINT('Origin',(474.115917770968,-92.9720072687899,380.000000551898));
#55695=CARTESIAN_POINT('Origin',(195.682801924451,-92.9720072687902,510.0000005519));
#55696=CARTESIAN_POINT('',(459.115917770968,-92.9720072687903,515.500000551898));
#55697=CARTESIAN_POINT('Origin',(459.115917770968,-92.9720072687903,510.000000551898));
#55698=CARTESIAN_POINT('',(474.115917770969,-92.9720072687903,515.500000551898));
#55699=CARTESIAN_POINT('',(195.682801924451,-92.9720072687902,515.500000551899));
#55700=CARTESIAN_POINT('Origin',(474.115917770968,-92.9720072687903,510.000000551898));
#55701=CARTESIAN_POINT('Origin',(195.682801924451,-92.97200726879,445.000000551899));
#55702=CARTESIAN_POINT('',(459.115917770968,-92.9720072687901,450.500000551898));
#55703=CARTESIAN_POINT('Origin',(459.115917770968,-92.9720072687901,445.000000551898));
#55704=CARTESIAN_POINT('',(474.115917770968,-92.9720072687901,450.500000551898));
#55705=CARTESIAN_POINT('',(195.682801924451,-92.97200726879,450.500000551899));
#55706=CARTESIAN_POINT('Origin',(474.115917770968,-92.9720072687901,445.000000551898));
#55707=CARTESIAN_POINT('Origin',(195.682801924451,-267.97200726879,380.000000551899));
#55708=CARTESIAN_POINT('',(459.115917770968,-267.97200726879,385.500000551898));
#55709=CARTESIAN_POINT('Origin',(459.115917770968,-267.97200726879,380.000000551898));
#55710=CARTESIAN_POINT('',(474.115917770968,-267.97200726879,385.500000551898));
#55711=CARTESIAN_POINT('',(195.682801924451,-267.97200726879,385.500000551899));
#55712=CARTESIAN_POINT('Origin',(474.115917770968,-267.97200726879,380.000000551898));
#55713=CARTESIAN_POINT('Origin',(195.682801924451,-267.97200726879,510.000000551899));
#55714=CARTESIAN_POINT('',(459.115917770968,-267.97200726879,515.500000551898));
#55715=CARTESIAN_POINT('Origin',(459.115917770968,-267.97200726879,510.000000551898));
#55716=CARTESIAN_POINT('',(474.115917770969,-267.97200726879,515.500000551898));
#55717=CARTESIAN_POINT('',(195.682801924451,-267.97200726879,515.500000551899));
#55718=CARTESIAN_POINT('Origin',(474.115917770968,-267.97200726879,510.000000551898));
#55719=CARTESIAN_POINT('Origin',(459.115917770968,-290.47200726879,360.000000551898));
#55720=CARTESIAN_POINT('',(459.115917770968,-290.47200726879,360.000000551898));
#55721=CARTESIAN_POINT('',(459.115917770968,-70.4720072687898,360.000000551899));
#55722=CARTESIAN_POINT('',(459.115917770968,-290.47200726879,360.000000551898));
#55723=CARTESIAN_POINT('',(474.115917770968,-70.4720072687898,360.000000551899));
#55724=CARTESIAN_POINT('',(459.115917770968,-70.4720072687898,360.000000551899));
#55725=CARTESIAN_POINT('',(474.115917770968,-290.47200726879,360.000000551898));
#55726=CARTESIAN_POINT('',(474.115917770968,-290.47200726879,360.000000551898));
#55727=CARTESIAN_POINT('',(459.115917770968,-290.47200726879,360.000000551898));
#55728=CARTESIAN_POINT('Origin',(459.115917770968,-290.47200726879,530.000000551898));
#55729=CARTESIAN_POINT('',(459.115917770968,-290.47200726879,530.000000551898));
#55730=CARTESIAN_POINT('',(459.115917770968,-290.47200726879,530.000000551898));
#55731=CARTESIAN_POINT('',(474.115917770968,-290.47200726879,530.000000551898));
#55732=CARTESIAN_POINT('',(474.115917770968,-290.47200726879,530.000000551898));
#55733=CARTESIAN_POINT('',(459.115917770968,-290.47200726879,530.000000551898));
#55734=CARTESIAN_POINT('Origin',(459.115917770969,-70.4720072687904,530.000000551899));
#55735=CARTESIAN_POINT('',(459.115917770969,-70.4720072687904,530.000000551899));
#55736=CARTESIAN_POINT('',(459.115917770969,-70.4720072687904,530.000000551899));
#55737=CARTESIAN_POINT('',(474.115917770969,-70.4720072687904,530.000000551899));
#55738=CARTESIAN_POINT('',(474.115917770969,-70.4720072687904,530.000000551899));
#55739=CARTESIAN_POINT('',(459.115917770969,-70.4720072687904,530.000000551899));
#55740=CARTESIAN_POINT('Origin',(459.115917770968,-70.4720072687898,360.000000551899));
#55741=CARTESIAN_POINT('',(459.115917770968,-70.4720072687898,360.000000551899));
#55742=CARTESIAN_POINT('',(474.115917770968,-70.4720072687898,360.000000551899));
#55743=CARTESIAN_POINT('Origin',(474.115917770968,-180.47200726879,445.000000551899));
#55744=CARTESIAN_POINT('Origin',(459.115917770968,-180.47200726879,445.000000551899));
#55745=CARTESIAN_POINT('',(0.,0.,0.));
#55746=CARTESIAN_POINT('Origin',(459.115917770968,-120.97200726879,530.000000551892));
#55747=CARTESIAN_POINT('',(459.115917770968,-134.97200726879,360.000000551892));
#55748=CARTESIAN_POINT('',(459.115917770968,-134.97200726879,530.000000551892));
#55749=CARTESIAN_POINT('',(459.115917770968,-134.97200726879,530.000000551892));
#55750=CARTESIAN_POINT('',(459.115917770968,-120.97200726879,360.000000551892));
#55751=CARTESIAN_POINT('',(459.115917770968,-124.47200726879,360.000000551892));
#55752=CARTESIAN_POINT('',(459.115917770968,-120.97200726879,530.000000551892));
#55753=CARTESIAN_POINT('',(459.115917770968,-120.97200726879,530.000000551892));
#55754=CARTESIAN_POINT('',(459.115917770968,-124.47200726879,530.000000551892));
#55755=CARTESIAN_POINT('Origin',(439.615917770968,-127.97200726879,530.000000551892));
#55756=CARTESIAN_POINT('',(417.115917770968,-120.97200726879,530.000000551893));
#55757=CARTESIAN_POINT('',(405.115917770968,-120.97200726879,530.000000551893));
#55758=CARTESIAN_POINT('',(417.115917770968,-134.97200726879,530.000000551893));
#55759=CARTESIAN_POINT('',(417.115917770968,-127.97200726879,530.000000551893));
#55760=CARTESIAN_POINT('',(405.115917770968,-134.97200726879,530.000000551893));
#55761=CARTESIAN_POINT('Origin',(405.115917770968,-120.97200726879,530.000000551893));
#55762=CARTESIAN_POINT('',(417.115917770967,-120.97200726879,360.000000551892));
#55763=CARTESIAN_POINT('',(422.365917770967,-120.97200726879,360.000000551892));
#55764=CARTESIAN_POINT('',(377.115917770967,-120.97200726879,400.000000551893));
#55765=CARTESIAN_POINT('',(361.615917770967,-120.97200726879,415.500000551893));
#55766=CARTESIAN_POINT('',(377.115917770967,-120.97200726879,414.064583955377));
#55767=CARTESIAN_POINT('',(377.115917770968,-120.97200726879,530.000000551893));
#55768=CARTESIAN_POINT('',(377.115917770967,-120.97200726879,475.935417148409));
#55769=CARTESIAN_POINT('Origin',(375.115917770968,-120.97200726879,445.000000551893));
#55770=CARTESIAN_POINT('',(377.115917770968,-120.97200726879,490.000000551893));
#55771=CARTESIAN_POINT('',(377.115917770968,-120.97200726879,530.000000551893));
#55772=CARTESIAN_POINT('',(404.115917770968,-120.97200726879,517.000000551893));
#55773=CARTESIAN_POINT('Origin',(375.115917770968,-120.97200726879,445.000000551893));
#55774=CARTESIAN_POINT('',(377.115917770967,-134.97200726879,475.935417148409));
#55775=CARTESIAN_POINT('',(377.115917770967,-120.97200726879,475.935417148409));
#55776=CARTESIAN_POINT('',(377.115917770967,-134.97200726879,414.064583955377));
#55777=CARTESIAN_POINT('',(377.115917770967,-120.97200726879,414.064583955377));
#55778=CARTESIAN_POINT('Origin',(375.115917770968,-134.97200726879,445.000000551893));
#55779=CARTESIAN_POINT('Origin',(474.115917770968,-134.97200726879,530.000000551892));
#55780=CARTESIAN_POINT('',(377.115917770968,-134.97200726879,490.000000551893));
#55781=CARTESIAN_POINT('',(421.365917770968,-134.97200726879,534.250000551893));
#55782=CARTESIAN_POINT('',(377.115917770967,-134.97200726879,360.000000551893));
#55783=CARTESIAN_POINT('',(377.115917770967,-134.97200726879,400.000000551893));
#55784=CARTESIAN_POINT('',(377.115917770967,-134.97200726879,360.000000551893));
#55785=CARTESIAN_POINT('',(417.115917770967,-134.97200726879,360.000000551892));
#55786=CARTESIAN_POINT('',(378.865917770968,-134.97200726879,398.250000551893));
#55787=CARTESIAN_POINT('',(456.865917770968,-134.97200726879,360.000000551892));
#55788=CARTESIAN_POINT('Origin',(377.115917770967,-127.97200726879,445.000000551893));
#55789=CARTESIAN_POINT('',(377.115917770967,-127.97200726879,400.000000551893));
#55790=CARTESIAN_POINT('Origin',(377.115917770967,-127.97200726879,445.000000551893));
#55791=CARTESIAN_POINT('',(377.115917770968,-127.97200726879,490.000000551893));
#55792=CARTESIAN_POINT('Origin',(397.115917770967,-127.97200726879,380.000000551893));
#55793=CARTESIAN_POINT('',(417.115917770967,-127.97200726879,360.000000551892));
#55794=CARTESIAN_POINT('Origin',(397.115917770968,-127.97200726879,510.000000551893));
#55795=CARTESIAN_POINT('Origin',(439.615917770967,-127.97200726879,360.000000551892));
#55796=CARTESIAN_POINT('',(0.,0.,0.));
#55797=CARTESIAN_POINT('Origin',(444.115917770963,-70.4720072687917,-76.1192491952379));
#55798=CARTESIAN_POINT('',(444.115917770964,-63.472007268792,350.000000551892));
#55799=CARTESIAN_POINT('Origin',(444.115917770964,-70.472007268792,350.000000551892));
#55800=CARTESIAN_POINT('',(444.115917770964,-63.472007268792,360.000000551892));
#55801=CARTESIAN_POINT('',(444.115917770963,-63.4720072687917,-76.1192491952379));
#55802=CARTESIAN_POINT('Origin',(444.115917770964,-70.472007268792,360.000000551892));
#55803=CARTESIAN_POINT('Origin',(194.115917770963,-290.472007268791,-76.1192491952372));
#55804=CARTESIAN_POINT('',(194.115917770964,-283.472007268791,350.000000551893));
#55805=CARTESIAN_POINT('Origin',(194.115917770964,-290.472007268791,350.000000551893));
#55806=CARTESIAN_POINT('',(194.115917770964,-283.472007268791,360.000000551893));
#55807=CARTESIAN_POINT('',(194.115917770963,-283.472007268791,-76.1192491952371));
#55808=CARTESIAN_POINT('Origin',(194.115917770964,-290.472007268791,360.000000551893));
#55809=CARTESIAN_POINT('Origin',(194.115917770963,-70.4720072687917,-76.119249195237));
#55810=CARTESIAN_POINT('',(194.115917770964,-63.472007268792,350.000000551893));
#55811=CARTESIAN_POINT('Origin',(194.115917770964,-70.472007268792,350.000000551893));
#55812=CARTESIAN_POINT('',(194.115917770964,-63.472007268792,360.000000551893));
#55813=CARTESIAN_POINT('',(194.115917770963,-63.4720072687916,-76.119249195237));
#55814=CARTESIAN_POINT('Origin',(194.115917770964,-70.472007268792,360.000000551893));
#55815=CARTESIAN_POINT('Origin',(444.115917770963,-290.472007268791,-76.119249195238));
#55816=CARTESIAN_POINT('',(444.115917770964,-283.472007268791,350.000000551892));
#55817=CARTESIAN_POINT('Origin',(444.115917770964,-290.472007268791,350.000000551892));
#55818=CARTESIAN_POINT('',(444.115917770964,-283.472007268791,360.000000551892));
#55819=CARTESIAN_POINT('',(444.115917770963,-283.472007268791,-76.119249195238));
#55820=CARTESIAN_POINT('Origin',(444.115917770964,-290.472007268791,360.000000551892));
#55821=CARTESIAN_POINT('Origin',(444.115917770964,-260.472007268791,360.000000551892));
#55822=CARTESIAN_POINT('',(444.115917770964,-260.472007268791,360.000000551892));
#55823=CARTESIAN_POINT('',(194.115917770964,-260.472007268791,360.000000551893));
#55824=CARTESIAN_POINT('',(381.615917770964,-260.472007268791,360.000000551892));
#55825=CARTESIAN_POINT('',(444.115917770964,-260.472007268791,350.000000551892));
#55826=CARTESIAN_POINT('',(444.115917770964,-260.472007268791,360.000000551892));
#55827=CARTESIAN_POINT('',(194.115917770964,-260.472007268791,350.000000551893));
#55828=CARTESIAN_POINT('',(381.615917770964,-260.472007268791,350.000000551892));
#55829=CARTESIAN_POINT('',(194.115917770964,-260.472007268791,360.000000551893));
#55830=CARTESIAN_POINT('Origin',(444.115917770964,-100.472007268791,360.000000551892));
#55831=CARTESIAN_POINT('',(444.115917770964,-100.472007268791,360.000000551892));
#55832=CARTESIAN_POINT('',(444.115917770964,-140.472007268791,360.000000551892));
#55833=CARTESIAN_POINT('',(444.115917770964,-100.472007268791,350.000000551892));
#55834=CARTESIAN_POINT('',(444.115917770964,-100.472007268791,360.000000551892));
#55835=CARTESIAN_POINT('',(444.115917770964,-140.472007268791,350.000000551892));
#55836=CARTESIAN_POINT('Origin',(194.115917770964,-100.472007268791,360.000000551893));
#55837=CARTESIAN_POINT('',(194.115917770964,-100.472007268791,360.000000551893));
#55838=CARTESIAN_POINT('',(256.615917770964,-100.472007268791,360.000000551893));
#55839=CARTESIAN_POINT('',(194.115917770964,-100.472007268791,350.000000551893));
#55840=CARTESIAN_POINT('',(194.115917770964,-100.472007268791,360.000000551893));
#55841=CARTESIAN_POINT('',(256.615917770964,-100.472007268791,350.000000551893));
#55842=CARTESIAN_POINT('Origin',(194.115917770964,-260.472007268791,360.000000551893));
#55843=CARTESIAN_POINT('',(194.115917770964,-220.472007268791,360.000000551893));
#55844=CARTESIAN_POINT('',(194.115917770964,-220.472007268791,350.000000551893));
#55845=CARTESIAN_POINT('Origin',(494.115917770964,-310.472007268791,360.000000551892));
#55846=CARTESIAN_POINT('',(494.115917770964,-310.472007268791,360.000000551892));
#55847=CARTESIAN_POINT('',(144.115917770964,-310.472007268791,360.000000551893));
#55848=CARTESIAN_POINT('',(494.115917770964,-310.472007268791,360.000000551892));
#55849=CARTESIAN_POINT('',(144.115917770964,-310.472007268791,350.000000551893));
#55850=CARTESIAN_POINT('',(144.115917770964,-310.472007268791,360.000000551893));
#55851=CARTESIAN_POINT('',(494.115917770964,-310.472007268791,350.000000551892));
#55852=CARTESIAN_POINT('',(494.115917770964,-310.472007268791,350.000000551892));
#55853=CARTESIAN_POINT('',(494.115917770964,-310.472007268791,360.000000551892));
#55854=CARTESIAN_POINT('Origin',(494.115917770964,-50.4720072687911,360.000000551892));
#55855=CARTESIAN_POINT('',(494.115917770964,-50.4720072687911,360.000000551892));
#55856=CARTESIAN_POINT('',(494.115917770964,-50.4720072687911,360.000000551892));
#55857=CARTESIAN_POINT('',(494.115917770964,-50.4720072687911,350.000000551892));
#55858=CARTESIAN_POINT('',(494.115917770964,-50.4720072687911,350.000000551892));
#55859=CARTESIAN_POINT('',(494.115917770964,-50.4720072687911,360.000000551892));
#55860=CARTESIAN_POINT('Origin',(144.115917770964,-50.472007268791,360.000000551893));
#55861=CARTESIAN_POINT('',(144.115917770964,-50.472007268791,360.000000551893));
#55862=CARTESIAN_POINT('',(144.115917770964,-50.472007268791,360.000000551893));
#55863=CARTESIAN_POINT('',(144.115917770964,-50.472007268791,350.000000551893));
#55864=CARTESIAN_POINT('',(144.115917770964,-50.472007268791,350.000000551893));
#55865=CARTESIAN_POINT('',(144.115917770964,-50.472007268791,360.000000551893));
#55866=CARTESIAN_POINT('Origin',(144.115917770964,-310.472007268791,360.000000551893));
#55867=CARTESIAN_POINT('',(144.115917770964,-310.472007268791,360.000000551893));
#55868=CARTESIAN_POINT('',(144.115917770964,-310.472007268791,350.000000551893));
#55869=CARTESIAN_POINT('Origin',(319.115917770964,-180.472007268791,350.000000551893));
#55870=CARTESIAN_POINT('Origin',(319.115917770964,-180.472007268791,360.000000551893));
#55871=CARTESIAN_POINT('',(0.,0.,0.));
#55872=CARTESIAN_POINT('',(0.,0.,0.));
#55873=CARTESIAN_POINT('',(0.,0.,0.));
#55874=CARTESIAN_POINT('',(0.,0.,0.));
#55875=CARTESIAN_POINT('',(-295.000000000001,-5.15143483426073E-13,-4.47641923528863E-12));
#55876=CARTESIAN_POINT('',(0.,0.,0.));
#55877=CARTESIAN_POINT('',(0.,-30.,-1.4210854715202E-13));
#55878=CARTESIAN_POINT('',(0.,-60.0000000000002,-1.4210854715202E-13));
#55879=CARTESIAN_POINT('',(0.,-90.0000000000002,-2.8421709430404E-13));
#55880=CARTESIAN_POINT('',(0.,-120.,-3.5527136788005E-13));
#55881=CARTESIAN_POINT('',(638.231835541936,-105.000000000002,890.000001103787));
#55882=CARTESIAN_POINT('',(638.231835541936,-75.0000000000021,890.000001103787));
#55883=CARTESIAN_POINT('',(638.231835541936,-45.0000000000026,890.000001103787));
#55884=CARTESIAN_POINT('',(638.231835541936,-15.0000000000026,890.000001103787));
#55885=CARTESIAN_POINT('',(638.231835541936,14.9999999999974,890.000001103787));
#55886=CARTESIAN_POINT('',(0.,0.,0.));
#55887=CARTESIAN_POINT('',(0.,0.,0.));
#55888=CARTESIAN_POINT('',(0.,0.,0.));
#55889=CARTESIAN_POINT('Origin',(263.115917770968,-180.47200726879,445.000000551893));
#55890=CARTESIAN_POINT('',(243.115917770968,-105.97200726879,445.000000551893));
#55891=CARTESIAN_POINT('',(243.115917770968,-254.97200726879,445.000000551893));
#55892=CARTESIAN_POINT('',(243.115917770968,-180.47200726879,445.000000551893));
#55893=CARTESIAN_POINT('',(283.115917770968,-105.97200726879,445.000000551893));
#55894=CARTESIAN_POINT('Origin',(263.115917770968,-105.97200726879,445.000000551893));
#55895=CARTESIAN_POINT('',(282.194701799307,-111.97200726879,439.000000551893));
#55896=CARTESIAN_POINT('Ctrl Pts',(283.115917770968,-105.97200726879,445.000000551893));
#55897=CARTESIAN_POINT('Ctrl Pts',(283.115917770968,-105.97200726879,444.241672021309));
#55898=CARTESIAN_POINT('Ctrl Pts',(283.068520438725,-106.124510775769,443.435925116929));
#55899=CARTESIAN_POINT('Ctrl Pts',(282.89734167077,-106.738309454724,441.958955713881));
#55900=CARTESIAN_POINT('Ctrl Pts',(282.775789023268,-107.199354583986,441.287371862459));
#55901=CARTESIAN_POINT('Ctrl Pts',(282.545652805548,-108.259536519781,440.227189926664));
#55902=CARTESIAN_POINT('Ctrl Pts',(282.421616893032,-108.931056193358,439.766267099578));
#55903=CARTESIAN_POINT('Ctrl Pts',(282.244676552118,-110.407792297934,439.152558719695));
#55904=CARTESIAN_POINT('Ctrl Pts',(282.194701799307,-111.213452760811,439.000000551893));
#55905=CARTESIAN_POINT('Ctrl Pts',(282.194701799307,-111.97200726879,439.000000551893));
#55906=CARTESIAN_POINT('',(282.194701799307,-248.97200726879,439.000000551893));
#55907=CARTESIAN_POINT('',(282.194701799307,-180.47200726879,439.000000551893));
#55908=CARTESIAN_POINT('',(283.115917770968,-254.97200726879,445.000000551893));
#55909=CARTESIAN_POINT('Ctrl Pts',(282.194701799307,-248.97200726879,439.000000551893));
#55910=CARTESIAN_POINT('Ctrl Pts',(282.194701799307,-249.730561776769,439.000000551893));
#55911=CARTESIAN_POINT('Ctrl Pts',(282.244676552118,-250.536222239646,439.152558719695));
#55912=CARTESIAN_POINT('Ctrl Pts',(282.421616893032,-252.012958344222,439.766267099578));
#55913=CARTESIAN_POINT('Ctrl Pts',(282.545652805548,-252.684478017799,440.227189926664));
#55914=CARTESIAN_POINT('Ctrl Pts',(282.775789023268,-253.744659953594,441.287371862459));
#55915=CARTESIAN_POINT('Ctrl Pts',(282.89734167077,-254.205705082856,441.958955713881));
#55916=CARTESIAN_POINT('Ctrl Pts',(283.068520438725,-254.819503761811,443.435925116929));
#55917=CARTESIAN_POINT('Ctrl Pts',(283.115917770968,-254.97200726879,444.241672021309));
#55918=CARTESIAN_POINT('Ctrl Pts',(283.115917770968,-254.97200726879,445.000000551893));
#55919=CARTESIAN_POINT('Origin',(263.115917770968,-254.97200726879,445.000000551893));
#55920=CARTESIAN_POINT('Origin',(278.115917770968,9.52799273120991,445.000000551893));
#55921=CARTESIAN_POINT('',(276.863644855836,9.52799273120991,451.000000551893));
#55922=CARTESIAN_POINT('',(276.863644855836,9.52799273120991,439.000000551893));
#55923=CARTESIAN_POINT('Ctrl Pts',(276.863644855836,9.52799273120992,451.000000551893));
#55924=CARTESIAN_POINT('Ctrl Pts',(276.863644855836,10.2911080617152,451.000000551893));
#55925=CARTESIAN_POINT('Ctrl Pts',(276.933905272325,11.0983145255455,450.845735154055));
#55926=CARTESIAN_POINT('Ctrl Pts',(277.178138317006,12.5735133048384,450.230998285314));
#55927=CARTESIAN_POINT('Ctrl Pts',(277.347642076354,13.2423907504513,449.77088390689));
#55928=CARTESIAN_POINT('Ctrl Pts',(277.659025023679,14.2983417003919,448.714932956949));
#55929=CARTESIAN_POINT('Ctrl Pts',(277.822400067743,14.7588613493959,448.045853243948));
#55930=CARTESIAN_POINT('Ctrl Pts',(278.05222803659,15.3739084341755,446.569865474975));
#55931=CARTESIAN_POINT('Ctrl Pts',(278.115917770968,15.5279927312099,445.762343892491));
#55932=CARTESIAN_POINT('Ctrl Pts',(278.115917770968,15.5279927312099,444.237657211294));
#55933=CARTESIAN_POINT('Ctrl Pts',(278.05222803659,15.3739084341755,443.430135628811));
#55934=CARTESIAN_POINT('Ctrl Pts',(277.822400067743,14.7588613493959,441.954147859838));
#55935=CARTESIAN_POINT('Ctrl Pts',(277.659025023679,14.2983417003919,441.285068146836));
#55936=CARTESIAN_POINT('Ctrl Pts',(277.347642076353,13.2423907504513,440.229117196896));
#55937=CARTESIAN_POINT('Ctrl Pts',(277.178138317006,12.5735133048384,439.769002818472));
#55938=CARTESIAN_POINT('Ctrl Pts',(276.933905272324,11.0983145255455,439.154265949731));
#55939=CARTESIAN_POINT('Ctrl Pts',(276.863644855836,10.2911080617152,439.000000551893));
#55940=CARTESIAN_POINT('Ctrl Pts',(276.863644855836,9.52799273120991,439.000000551893));
#55941=CARTESIAN_POINT('',(270.115917770968,9.52799273120991,451.000000551893));
#55942=CARTESIAN_POINT('',(278.115917770968,9.52799273120991,451.000000551893));
#55943=CARTESIAN_POINT('',(270.115917770968,9.52799273120991,439.000000551893));
#55944=CARTESIAN_POINT('Origin',(270.115917770968,9.52799273120991,445.000000551893));
#55945=CARTESIAN_POINT('',(278.115917770968,9.52799273120991,439.000000551893));
#55946=CARTESIAN_POINT('Origin',(278.115917770968,9.52799273120991,439.000000551893));
#55947=CARTESIAN_POINT('',(276.863644855836,-20.4720072687901,439.000000551893));
#55948=CARTESIAN_POINT('',(276.863644855836,-39.9720072687901,439.000000551893));
#55949=CARTESIAN_POINT('',(270.115917770968,-20.4720072687901,439.000000551893));
#55950=CARTESIAN_POINT('',(270.115917770968,-20.4720072687901,439.000000551893));
#55951=CARTESIAN_POINT('',(278.115917770968,-20.4720072687901,439.000000551893));
#55952=CARTESIAN_POINT('Origin',(278.115917770968,-20.4720072687901,451.000000551893));
#55953=CARTESIAN_POINT('',(276.863644855836,-20.4720072687901,451.000000551893));
#55954=CARTESIAN_POINT('',(276.863644855836,-39.9720072687901,451.000000551893));
#55955=CARTESIAN_POINT('',(270.115917770968,-20.4720072687901,451.000000551893));
#55956=CARTESIAN_POINT('',(278.115917770968,-20.4720072687901,451.000000551893));
#55957=CARTESIAN_POINT('',(270.115917770968,9.52799273120991,451.000000551893));
#55958=CARTESIAN_POINT('Origin',(278.115917770968,-20.4720072687901,445.000000551893));
#55959=CARTESIAN_POINT('Ctrl Pts',(276.863644855836,-20.4720072687901,451.000000551893));
#55960=CARTESIAN_POINT('Ctrl Pts',(276.863644855836,-21.2351225992954,451.000000551893));
#55961=CARTESIAN_POINT('Ctrl Pts',(276.933905272325,-22.0423290631257,450.845735154055));
#55962=CARTESIAN_POINT('Ctrl Pts',(277.178138317006,-23.5175278424185,450.230998285314));
#55963=CARTESIAN_POINT('Ctrl Pts',(277.347642076354,-24.1864052880315,449.77088390689));
#55964=CARTESIAN_POINT('Ctrl Pts',(277.659025023679,-25.2423562379721,448.71493295695));
#55965=CARTESIAN_POINT('Ctrl Pts',(277.822400067743,-25.702875886976,448.045853243948));
#55966=CARTESIAN_POINT('Ctrl Pts',(278.05222803659,-26.3179229717557,446.569865474975));
#55967=CARTESIAN_POINT('Ctrl Pts',(278.115917770968,-26.4720072687901,445.762343892492));
#55968=CARTESIAN_POINT('Ctrl Pts',(278.115917770968,-26.4720072687901,444.237657211294));
#55969=CARTESIAN_POINT('Ctrl Pts',(278.05222803659,-26.3179229717557,443.430135628811));
#55970=CARTESIAN_POINT('Ctrl Pts',(277.822400067743,-25.702875886976,441.954147859838));
#55971=CARTESIAN_POINT('Ctrl Pts',(277.659025023679,-25.2423562379721,441.285068146836));
#55972=CARTESIAN_POINT('Ctrl Pts',(277.347642076353,-24.1864052880315,440.229117196896));
#55973=CARTESIAN_POINT('Ctrl Pts',(277.178138317006,-23.5175278424185,439.769002818472));
#55974=CARTESIAN_POINT('Ctrl Pts',(276.933905272324,-22.0423290631256,439.154265949731));
#55975=CARTESIAN_POINT('Ctrl Pts',(276.863644855836,-21.2351225992954,439.000000551893));
#55976=CARTESIAN_POINT('Ctrl Pts',(276.863644855836,-20.4720072687901,439.000000551893));
#55977=CARTESIAN_POINT('Origin',(270.115917770968,-20.4720072687901,445.000000551893));
#55978=CARTESIAN_POINT('Origin',(270.115917770968,-5.47200726879009,445.000000551893));
#55979=CARTESIAN_POINT('Origin',(263.115917770968,-98.97200726879,445.000000551893));
#55980=CARTESIAN_POINT('',(263.115917770968,-98.97200726879,430.000000551893));
#55981=CARTESIAN_POINT('',(248.115917770968,-98.97200726879,445.000000551893));
#55982=CARTESIAN_POINT('Origin',(263.115917770968,-98.97200726879,445.000000551893));
#55983=CARTESIAN_POINT('Origin',(263.115917770968,-98.97200726879,445.000000551893));
#55984=CARTESIAN_POINT('',(263.115917770968,-99.47200726879,429.500000551893));
#55985=CARTESIAN_POINT('Origin',(263.115917770968,-98.97200726879,429.500000551893));
#55986=CARTESIAN_POINT('Origin',(263.115917770968,-99.47200726879,445.000000551893));
#55987=CARTESIAN_POINT('Origin',(278.115917770968,-99.47200726879,445.000000551893));
#55988=CARTESIAN_POINT('',(281.115917770968,-99.47200726879,445.000000551893));
#55989=CARTESIAN_POINT('Origin',(263.115917770968,-99.47200726879,445.000000551893));
#55990=CARTESIAN_POINT('Origin',(263.115917770968,-39.9720072687901,445.000000551893));
#55991=CARTESIAN_POINT('',(248.115917770968,19.52799273121,445.000000551893));
#55992=CARTESIAN_POINT('Origin',(263.115917770968,19.5279927312099,445.000000551893));
#55993=CARTESIAN_POINT('',(248.115917770968,-39.9720072687901,445.000000551893));
#55994=CARTESIAN_POINT('Origin',(263.115917770968,-261.47200726879,445.000000551893));
#55995=CARTESIAN_POINT('',(263.115917770968,-260.97200726879,429.500000551893));
#55996=CARTESIAN_POINT('Origin',(263.115917770968,-260.97200726879,445.000000551893));
#55997=CARTESIAN_POINT('',(263.115917770968,-261.47200726879,430.000000551893));
#55998=CARTESIAN_POINT('Origin',(263.115917770968,-261.47200726879,429.500000551893));
#55999=CARTESIAN_POINT('',(248.115917770968,-261.47200726879,445.000000551893));
#56000=CARTESIAN_POINT('Origin',(263.115917770968,-261.47200726879,445.000000551893));
#56001=CARTESIAN_POINT('Origin',(263.115917770968,-261.47200726879,445.000000551893));
#56002=CARTESIAN_POINT('Origin',(281.615917770968,-260.97200726879,445.000000551893));
#56003=CARTESIAN_POINT('',(281.115917770968,-260.97200726879,445.000000551893));
#56004=CARTESIAN_POINT('Origin',(263.115917770968,-260.97200726879,445.000000551893));
#56005=CARTESIAN_POINT('Origin',(263.115917770968,-295.97200726879,445.000000551893));
#56006=CARTESIAN_POINT('',(248.115917770968,-329.97200726879,445.000000551893));
#56007=CARTESIAN_POINT('',(248.115917770968,-295.97200726879,445.000000551893));
#56008=CARTESIAN_POINT('',(278.115917770968,-329.97200726879,445.000000551893));
#56009=CARTESIAN_POINT('Origin',(263.115917770968,-329.97200726879,445.000000551893));
#56010=CARTESIAN_POINT('Origin',(263.115917770968,-329.97200726879,445.000000551893));
#56011=CARTESIAN_POINT('Origin',(263.115917770968,-260.72200726879,445.000000551893));
#56012=CARTESIAN_POINT('',(281.615917770968,-260.47200726879,445.000000551893));
#56013=CARTESIAN_POINT('',(244.615917770968,-260.47200726879,445.000000551893));
#56014=CARTESIAN_POINT('Origin',(263.115917770968,-260.47200726879,445.000000551893));
#56015=CARTESIAN_POINT('Origin',(263.115917770968,-260.47200726879,445.000000551893));
#56016=CARTESIAN_POINT('',(281.365917770968,-260.72200726879,445.000000551893));
#56017=CARTESIAN_POINT('Origin',(263.115917770968,-258.47200726879,445.000000551893));
#56018=CARTESIAN_POINT('',(244.615917770968,-255.97200726879,445.000000551893));
#56019=CARTESIAN_POINT('',(263.115917770968,-255.97200726879,426.500000551893));
#56020=CARTESIAN_POINT('Origin',(263.115917770968,-255.97200726879,445.000000551893));
#56021=CARTESIAN_POINT('',(244.615917770968,-258.47200726879,445.000000551893));
#56022=CARTESIAN_POINT('Origin',(263.115917770968,-255.97200726879,445.000000551893));
#56023=CARTESIAN_POINT('Origin',(263.115917770968,-99.72200726879,445.000000551893));
#56024=CARTESIAN_POINT('',(281.615917770968,-99.97200726879,445.000000551893));
#56025=CARTESIAN_POINT('',(244.615917770968,-99.97200726879,445.000000551893));
#56026=CARTESIAN_POINT('Origin',(263.115917770968,-99.97200726879,445.000000551893));
#56027=CARTESIAN_POINT('Origin',(263.115917770968,-99.97200726879,445.000000551893));
#56028=CARTESIAN_POINT('',(281.365917770968,-99.72200726879,445.000000551893));
#56029=CARTESIAN_POINT('Origin',(263.115917770968,-102.22200726879,445.000000551893));
#56030=CARTESIAN_POINT('',(244.615917770968,-104.97200726879,445.000000551893));
#56031=CARTESIAN_POINT('',(244.615917770968,-102.22200726879,445.000000551893));
#56032=CARTESIAN_POINT('',(263.115917770968,-104.97200726879,426.500000551893));
#56033=CARTESIAN_POINT('Origin',(263.115917770968,-104.97200726879,445.000000551893));
#56034=CARTESIAN_POINT('Origin',(263.115917770968,-104.97200726879,445.000000551893));
#56035=CARTESIAN_POINT('Origin',(263.115917770968,-330.47200726879,445.000000551893));
#56036=CARTESIAN_POINT('',(277.115917770968,-330.97200726879,445.000000551893));
#56037=CARTESIAN_POINT('',(277.615917770968,-330.47200726879,445.000000551893));
#56038=CARTESIAN_POINT('Origin',(263.115917770968,-330.97200726879,445.000000551893));
#56039=CARTESIAN_POINT('Origin',(278.115917770968,-330.97200726879,445.000000551893));
#56040=CARTESIAN_POINT('Origin',(283.115917770968,-248.97200726879,445.000000551893));
#56041=CARTESIAN_POINT('',(275.115917770968,-248.97200726879,439.000000551893));
#56042=CARTESIAN_POINT('',(283.115917770968,-248.97200726879,439.000000551893));
#56043=CARTESIAN_POINT('',(275.115917770968,-248.97200726879,451.000000551893));
#56044=CARTESIAN_POINT('Origin',(275.115917770968,-248.97200726879,445.000000551893));
#56045=CARTESIAN_POINT('',(282.194701799307,-248.97200726879,451.000000551893));
#56046=CARTESIAN_POINT('',(283.115917770968,-248.97200726879,451.000000551893));
#56047=CARTESIAN_POINT('Ctrl Pts',(283.115917770968,-254.97200726879,445.000000551893));
#56048=CARTESIAN_POINT('Ctrl Pts',(283.115917770968,-254.97200726879,445.758329082477));
#56049=CARTESIAN_POINT('Ctrl Pts',(283.068520438725,-254.819503761811,446.564075986857));
#56050=CARTESIAN_POINT('Ctrl Pts',(282.89734167077,-254.205705082856,448.041045389906));
#56051=CARTESIAN_POINT('Ctrl Pts',(282.775789023268,-253.744659953594,448.712629241327));
#56052=CARTESIAN_POINT('Ctrl Pts',(282.545652805548,-252.684478017799,449.772811177122));
#56053=CARTESIAN_POINT('Ctrl Pts',(282.421616893032,-252.012958344222,450.233734004208));
#56054=CARTESIAN_POINT('Ctrl Pts',(282.244676552118,-250.536222239646,450.847442384092));
#56055=CARTESIAN_POINT('Ctrl Pts',(282.194701799307,-249.730561776768,451.000000551893));
#56056=CARTESIAN_POINT('Ctrl Pts',(282.194701799307,-248.97200726879,451.000000551893));
#56057=CARTESIAN_POINT('Origin',(283.115917770968,-248.97200726879,451.000000551893));
#56058=CARTESIAN_POINT('',(282.194701799307,-111.97200726879,451.000000551893));
#56059=CARTESIAN_POINT('',(282.194701799307,-180.47200726879,451.000000551893));
#56060=CARTESIAN_POINT('',(275.115917770968,-111.97200726879,451.000000551893));
#56061=CARTESIAN_POINT('',(275.115917770968,-111.97200726879,451.000000551893));
#56062=CARTESIAN_POINT('',(283.115917770968,-111.97200726879,451.000000551893));
#56063=CARTESIAN_POINT('Origin',(283.115917770968,-111.97200726879,439.000000551893));
#56064=CARTESIAN_POINT('',(275.115917770968,-111.97200726879,439.000000551893));
#56065=CARTESIAN_POINT('',(283.115917770968,-111.97200726879,439.000000551893));
#56066=CARTESIAN_POINT('',(275.115917770968,-248.97200726879,439.000000551893));
#56067=CARTESIAN_POINT('Origin',(283.115917770968,-111.97200726879,445.000000551893));
#56068=CARTESIAN_POINT('Ctrl Pts',(282.194701799307,-111.97200726879,451.000000551893));
#56069=CARTESIAN_POINT('Ctrl Pts',(282.194701799307,-111.213452760811,451.000000551893));
#56070=CARTESIAN_POINT('Ctrl Pts',(282.244676552118,-110.407792297934,450.847442384091));
#56071=CARTESIAN_POINT('Ctrl Pts',(282.421616893032,-108.931056193358,450.233734004208));
#56072=CARTESIAN_POINT('Ctrl Pts',(282.545652805548,-108.259536519781,449.772811177122));
#56073=CARTESIAN_POINT('Ctrl Pts',(282.775789023268,-107.199354583986,448.712629241327));
#56074=CARTESIAN_POINT('Ctrl Pts',(282.89734167077,-106.738309454724,448.041045389905));
#56075=CARTESIAN_POINT('Ctrl Pts',(283.068520438725,-106.124510775769,446.564075986857));
#56076=CARTESIAN_POINT('Ctrl Pts',(283.115917770968,-105.97200726879,445.758329082477));
#56077=CARTESIAN_POINT('Ctrl Pts',(283.115917770968,-105.97200726879,445.000000551893));
#56078=CARTESIAN_POINT('Origin',(275.115917770968,-111.97200726879,445.000000551893));
#56079=CARTESIAN_POINT('Origin',(275.115917770968,-180.47200726879,445.000000551893));
#56080=CARTESIAN_POINT('Origin',(263.115917770968,-180.47200726879,445.000000551893));
#56081=CARTESIAN_POINT('Origin',(263.115917770968,-254.97200726879,445.000000551893));
#56082=CARTESIAN_POINT('Origin',(263.115917770968,-105.97200726879,445.000000551893));
#56083=CARTESIAN_POINT('Origin',(263.115917770968,20.0279927312099,445.000000551893));
#56084=CARTESIAN_POINT('',(249.115917770968,20.52799273121,445.000000551893));
#56085=CARTESIAN_POINT('',(248.615917770968,20.0279927312099,445.000000551893));
#56086=CARTESIAN_POINT('Origin',(263.115917770968,20.5279927312099,445.000000551893));
#56087=CARTESIAN_POINT('Origin',(263.115917770968,20.5279927312099,445.000000551893));
#56088=CARTESIAN_POINT('Origin',(263.115917770968,-255.97200726879,445.000000551893));
#56089=CARTESIAN_POINT('',(263.115917770968,-255.47200726879,426.000000551893));
#56090=CARTESIAN_POINT('Origin',(263.115917770968,-255.47200726879,445.000000551893));
#56091=CARTESIAN_POINT('Origin',(263.115917770968,-255.97200726879,426.000000551893));
#56092=CARTESIAN_POINT('Origin',(282.615917770968,-255.47200726879,445.000000551893));
#56093=CARTESIAN_POINT('',(243.615917770968,-255.47200726879,445.000000551893));
#56094=CARTESIAN_POINT('Origin',(263.115917770968,-255.47200726879,445.000000551893));
#56095=CARTESIAN_POINT('Origin',(263.115917770968,-255.22200726879,445.000000551893));
#56096=CARTESIAN_POINT('',(243.365917770968,-255.22200726879,445.000000551893));
#56097=CARTESIAN_POINT('Origin',(263.115917770968,-105.72200726879,445.000000551893));
#56098=CARTESIAN_POINT('',(243.615917770968,-105.47200726879,445.000000551893));
#56099=CARTESIAN_POINT('',(243.365917770968,-105.72200726879,445.000000551893));
#56100=CARTESIAN_POINT('Origin',(263.115917770968,-105.47200726879,445.000000551893));
#56101=CARTESIAN_POINT('Origin',(282.115917770968,-105.47200726879,445.000000551893));
#56102=CARTESIAN_POINT('',(263.115917770968,-105.47200726879,426.000000551893));
#56103=CARTESIAN_POINT('Origin',(263.115917770968,-105.47200726879,445.000000551893));
#56104=CARTESIAN_POINT('Origin',(263.115917770968,-104.97200726879,445.000000551893));
#56105=CARTESIAN_POINT('Origin',(263.115917770968,-104.97200726879,426.000000551893));
#56106=CARTESIAN_POINT('',(0.,0.,0.));
#56107=CARTESIAN_POINT('Origin',(375.115917770968,-180.47200726879,445.000000551892));
#56108=CARTESIAN_POINT('',(373.557025589832,-105.97200726879,464.93915437465));
#56109=CARTESIAN_POINT('',(373.557025589832,-254.972007268791,464.93915437465));
#56110=CARTESIAN_POINT('',(373.557025589832,-180.47200726879,464.93915437465));
#56111=CARTESIAN_POINT('',(376.674809952104,-105.97200726879,425.060846729135));
#56112=CARTESIAN_POINT('Origin',(375.115917770968,-105.97200726879,445.000000551892));
#56113=CARTESIAN_POINT('',(370.621259986509,-111.97200726879,425.511592422941));
#56114=CARTESIAN_POINT('Ctrl Pts',(376.674809952104,-105.97200726879,425.060846729135));
#56115=CARTESIAN_POINT('Ctrl Pts',(375.918788491129,-105.97200726879,425.001739108282));
#56116=CARTESIAN_POINT('Ctrl Pts',(375.111798551165,-106.124510775769,424.986188615741));
#56117=CARTESIAN_POINT('Ctrl Pts',(373.625980083073,-106.738309454724,425.041724802303));
#56118=CARTESIAN_POINT('Ctrl Pts',(372.946965023565,-107.199354583986,425.110561308361));
#56119=CARTESIAN_POINT('Ctrl Pts',(371.872070611148,-108.259536519781,425.257361914111));
#56120=CARTESIAN_POINT('Ctrl Pts',(371.402882122954,-108.931056193358,425.345094021509));
#56121=CARTESIAN_POINT('Ctrl Pts',(370.777249287815,-110.407792297934,425.473660795511));
#56122=CARTESIAN_POINT('Ctrl Pts',(370.621259986509,-111.213452760812,425.511592422941));
#56123=CARTESIAN_POINT('Ctrl Pts',(370.621259986509,-111.97200726879,425.511592422941));
#56124=CARTESIAN_POINT('',(370.621259986508,-248.97200726879,425.51159242294));
#56125=CARTESIAN_POINT('',(370.621259986508,-180.47200726879,425.511592422941));
#56126=CARTESIAN_POINT('',(376.674809952104,-254.97200726879,425.060846729135));
#56127=CARTESIAN_POINT('Ctrl Pts',(370.621259986508,-248.97200726879,425.51159242294));
#56128=CARTESIAN_POINT('Ctrl Pts',(370.621259986508,-249.730561776769,425.51159242294));
#56129=CARTESIAN_POINT('Ctrl Pts',(370.777249287815,-250.536222239647,425.473660795511));
#56130=CARTESIAN_POINT('Ctrl Pts',(371.402882122954,-252.012958344223,425.345094021508));
#56131=CARTESIAN_POINT('Ctrl Pts',(371.872070611148,-252.6844780178,425.257361914111));
#56132=CARTESIAN_POINT('Ctrl Pts',(372.946965023565,-253.744659953595,425.110561308361));
#56133=CARTESIAN_POINT('Ctrl Pts',(373.625980083073,-254.205705082856,425.041724802303));
#56134=CARTESIAN_POINT('Ctrl Pts',(375.111798551165,-254.819503761812,424.98618861574));
#56135=CARTESIAN_POINT('Ctrl Pts',(375.918788491129,-254.97200726879,425.001739108282));
#56136=CARTESIAN_POINT('Ctrl Pts',(376.674809952104,-254.97200726879,425.060846729135));
#56137=CARTESIAN_POINT('Origin',(375.115917770968,-254.97200726879,445.000000551892));
#56138=CARTESIAN_POINT('Origin',(375.115917770968,70.2779927312095,445.000000551893));
#56139=CARTESIAN_POINT('',(376.090225384178,70.0279927312094,432.538029412669));
#56140=CARTESIAN_POINT('',(374.141610157758,70.0279927312094,457.461971691116));
#56141=CARTESIAN_POINT('Origin',(375.115917770968,70.0279927312094,445.000000551893));
#56142=CARTESIAN_POINT('Origin',(375.115917770968,70.0279927312094,445.000000551893));
#56143=CARTESIAN_POINT('',(376.05125307965,70.5279927312094,433.036508258238));
#56144=CARTESIAN_POINT('',(376.070739231914,70.2779927312095,432.787268835454));
#56145=CARTESIAN_POINT('Origin',(375.115917770968,70.5279927312094,445.000000551893));
#56146=CARTESIAN_POINT('Origin',(375.115917770968,20.5279927312094,445.000000551893));
#56147=CARTESIAN_POINT('',(374.141610157758,-29.4720072687906,457.461971691116));
#56148=CARTESIAN_POINT('',(374.141610157758,20.5279927312094,457.461971691116));
#56149=CARTESIAN_POINT('Origin',(375.115917770968,-29.4720072687906,445.000000551893));
#56150=CARTESIAN_POINT('',(369.988900990807,56.9410394849244,433.599838319014));
#56151=CARTESIAN_POINT('',(369.988900990807,-15.0589605150756,433.599838319014));
#56152=CARTESIAN_POINT('',(369.988900990807,20.5279927312094,433.599838319014));
#56153=CARTESIAN_POINT('',(381.952393284462,-15.0589605150756,434.535173627696));
#56154=CARTESIAN_POINT('Ctrl Pts',(369.988900990807,-15.0589605150755,433.599838319014));
#56155=CARTESIAN_POINT('Ctrl Pts',(369.988900990807,-15.8272357942547,433.599838319014));
#56156=CARTESIAN_POINT('Ctrl Pts',(370.151524843035,-16.635872857665,433.522949429245));
#56157=CARTESIAN_POINT('Ctrl Pts',(370.78905122987,-18.1091493532521,433.267732479884));
#56158=CARTESIAN_POINT('Ctrl Pts',(371.263063224569,-18.7752122333175,433.095435318238));
#56159=CARTESIAN_POINT('Ctrl Pts',(372.341025514289,-19.8267981076742,432.799110512512));
#56160=CARTESIAN_POINT('Ctrl Pts',(373.020881601515,-20.2868198879197,432.653987167789));
#56161=CARTESIAN_POINT('Ctrl Pts',(374.513080057484,-20.9032184113205,432.492010706903));
#56162=CARTESIAN_POINT('Ctrl Pts',(375.326021983044,-21.0589605150756,432.478282107572));
#56163=CARTESIAN_POINT('Ctrl Pts',(376.854428785312,-21.0589605150756,432.597776717766));
#56164=CARTESIAN_POINT('Ctrl Pts',(377.655359248128,-20.9032184113205,432.737681837422));
#56165=CARTESIAN_POINT('Ctrl Pts',(379.104252847889,-20.2868198879197,433.129600122843));
#56166=CARTESIAN_POINT('Ctrl Pts',(379.753293853246,-19.8267981076742,433.378619917013));
#56167=CARTESIAN_POINT('Ctrl Pts',(380.77210481419,-18.7752122333175,433.838875622472));
#56168=CARTESIAN_POINT('Ctrl Pts',(381.213579664274,-18.1091493532521,434.082747801641));
#56169=CARTESIAN_POINT('Ctrl Pts',(381.803695113145,-16.635872857665,434.433944814947));
#56170=CARTESIAN_POINT('Ctrl Pts',(381.952393284462,-15.8272357942547,434.535173627696));
#56171=CARTESIAN_POINT('Ctrl Pts',(381.952393284462,-15.0589605150756,434.535173627696));
#56172=CARTESIAN_POINT('',(381.952393284462,56.9410394849244,434.535173627696));
#56173=CARTESIAN_POINT('',(381.952393284462,20.5279927312094,434.535173627696));
#56174=CARTESIAN_POINT('Ctrl Pts',(381.952393284462,56.9410394849244,434.535173627696));
#56175=CARTESIAN_POINT('Ctrl Pts',(381.952393284462,57.7093147641036,434.535173627696));
#56176=CARTESIAN_POINT('Ctrl Pts',(381.803695113145,58.5179518275139,434.433944814947));
#56177=CARTESIAN_POINT('Ctrl Pts',(381.213579664274,59.991228323101,434.082747801641));
#56178=CARTESIAN_POINT('Ctrl Pts',(380.77210481419,60.6572912031664,433.838875622472));
#56179=CARTESIAN_POINT('Ctrl Pts',(379.753293853246,61.7088770775231,433.378619917013));
#56180=CARTESIAN_POINT('Ctrl Pts',(379.104252847889,62.1688988577686,433.129600122844));
#56181=CARTESIAN_POINT('Ctrl Pts',(377.655359248128,62.7852973811694,432.737681837422));
#56182=CARTESIAN_POINT('Ctrl Pts',(376.854428785312,62.9410394849244,432.597776717766));
#56183=CARTESIAN_POINT('Ctrl Pts',(375.326021983044,62.9410394849244,432.478282107572));
#56184=CARTESIAN_POINT('Ctrl Pts',(374.513080057484,62.7852973811694,432.492010706903));
#56185=CARTESIAN_POINT('Ctrl Pts',(373.020881601515,62.1688988577686,432.65398716779));
#56186=CARTESIAN_POINT('Ctrl Pts',(372.341025514289,61.7088770775231,432.799110512512));
#56187=CARTESIAN_POINT('Ctrl Pts',(371.263063224569,60.6572912031664,433.095435318238));
#56188=CARTESIAN_POINT('Ctrl Pts',(370.78905122987,59.991228323101,433.267732479884));
#56189=CARTESIAN_POINT('Ctrl Pts',(370.151524843035,58.5179518275139,433.522949429245));
#56190=CARTESIAN_POINT('Ctrl Pts',(369.988900990807,57.7093147641036,433.599838319014));
#56191=CARTESIAN_POINT('Ctrl Pts',(369.988900990807,56.9410394849244,433.599838319014));
#56192=CARTESIAN_POINT('Origin',(375.115917770968,70.5279927312094,445.000000551893));
#56193=CARTESIAN_POINT('Origin',(375.115917770968,-29.7220072687906,445.000000551893));
#56194=CARTESIAN_POINT('',(376.28508690682,-29.9720072687906,430.045635184824));
#56195=CARTESIAN_POINT('',(373.946748635116,-29.9720072687906,459.954365918961));
#56196=CARTESIAN_POINT('Origin',(375.115917770968,-29.9720072687906,445.000000551893));
#56197=CARTESIAN_POINT('Origin',(375.115917770968,-29.9720072687906,445.000000551893));
#56198=CARTESIAN_POINT('',(376.246114602291,-29.4720072687906,430.544114030393));
#56199=CARTESIAN_POINT('',(376.265600754556,-29.7220072687906,430.294874607609));
#56200=CARTESIAN_POINT('Origin',(375.115917770968,-29.4720072687906,445.000000551893));
#56201=CARTESIAN_POINT('Origin',(375.115917770968,-62.3557281990226,445.000000551893));
#56202=CARTESIAN_POINT('',(373.946748635116,-98.9720072687905,459.954365918961));
#56203=CARTESIAN_POINT('',(373.946748635116,-62.3557281990226,459.954365918961));
#56204=CARTESIAN_POINT('',(360.1615524039,-98.9720072687905,443.830831416041));
#56205=CARTESIAN_POINT('Origin',(375.115917770968,-98.9720072687905,445.000000551892));
#56206=CARTESIAN_POINT('Origin',(375.115917770968,-98.9720072687905,445.000000551892));
#56207=CARTESIAN_POINT('Origin',(376.090225384178,-29.4720072687906,432.538029412669));
#56208=CARTESIAN_POINT('Origin',(382.266833053647,-15.0589605150756,430.513302839165));
#56209=CARTESIAN_POINT('',(381.643276181193,-15.0589605150756,438.488964368268));
#56210=CARTESIAN_POINT('',(382.266833053647,-15.0589605150756,430.513302839165));
#56211=CARTESIAN_POINT('',(381.643276181193,56.9410394849244,438.488964368268));
#56212=CARTESIAN_POINT('',(381.643276181193,56.9410394849244,438.488964368268));
#56213=CARTESIAN_POINT('',(382.266833053647,56.9410394849244,430.513302839165));
#56214=CARTESIAN_POINT('Origin',(376.28508690682,56.9410394849244,430.045635184824));
#56215=CARTESIAN_POINT('',(369.679783887538,56.9410394849244,437.553629059587));
#56216=CARTESIAN_POINT('Origin',(375.661530034366,56.9410394849244,438.021296713927));
#56217=CARTESIAN_POINT('',(370.303340759993,56.9410394849244,429.577967530484));
#56218=CARTESIAN_POINT('Origin',(370.303340759993,-10.8264023755406,429.577967530484));
#56219=CARTESIAN_POINT('',(369.679783887538,-15.0589605150756,437.553629059587));
#56220=CARTESIAN_POINT('',(369.679783887538,-10.8264023755406,437.553629059587));
#56221=CARTESIAN_POINT('',(370.303340759993,-15.0589605150756,429.577967530484));
#56222=CARTESIAN_POINT('Origin',(376.28508690682,-15.0589605150756,430.045635184824));
#56223=CARTESIAN_POINT('Origin',(375.661530034366,-15.0589605150756,438.021296713927));
#56224=CARTESIAN_POINT('Origin',(375.661530034366,-15.0589605150756,438.021296713927));
#56225=CARTESIAN_POINT('Origin',(375.115917770968,-260.72200726879,445.000000551892));
#56226=CARTESIAN_POINT('',(376.557893038519,-260.47200726879,426.556283265841));
#56227=CARTESIAN_POINT('',(373.673942503417,-260.47200726879,463.443717837943));
#56228=CARTESIAN_POINT('Origin',(375.115917770968,-260.47200726879,445.000000551892));
#56229=CARTESIAN_POINT('Origin',(375.115917770968,-260.47200726879,445.000000551892));
#56230=CARTESIAN_POINT('',(376.51892073399,-260.97200726879,427.05476211141));
#56231=CARTESIAN_POINT('',(376.538406886254,-260.72200726879,426.805522688626));
#56232=CARTESIAN_POINT('Origin',(375.115917770968,-260.97200726879,445.000000551892));
#56233=CARTESIAN_POINT('Origin',(376.557893038519,-260.97200726879,426.556283265841));
#56234=CARTESIAN_POINT('',(359.663073558331,-260.97200726879,443.791859111512));
#56235=CARTESIAN_POINT('Origin',(375.115917770968,-260.97200726879,445.000000551892));
#56236=CARTESIAN_POINT('Origin',(375.115917770968,-258.47200726879,445.000000551892));
#56237=CARTESIAN_POINT('',(373.673942503417,-255.972007268791,463.443717837943));
#56238=CARTESIAN_POINT('',(356.672200484917,-255.97200726879,443.558025284342));
#56239=CARTESIAN_POINT('Origin',(375.115917770968,-255.97200726879,445.000000551892));
#56240=CARTESIAN_POINT('',(373.673942503417,-258.472007268791,463.443717837943));
#56241=CARTESIAN_POINT('Origin',(375.115917770968,-255.97200726879,445.000000551892));
#56242=CARTESIAN_POINT('Origin',(375.115917770968,-261.47200726879,445.000000551892));
#56243=CARTESIAN_POINT('',(360.1615524039,-261.47200726879,443.83083141604));
#56244=CARTESIAN_POINT('Origin',(359.663073558331,-261.47200726879,443.791859111512));
#56245=CARTESIAN_POINT('',(373.946748635116,-261.47200726879,459.954365918961));
#56246=CARTESIAN_POINT('Origin',(375.115917770968,-261.47200726879,445.000000551892));
#56247=CARTESIAN_POINT('Origin',(375.115917770968,-261.47200726879,445.000000551892));
#56248=CARTESIAN_POINT('Origin',(375.115917770968,-295.972007268791,445.000000551892));
#56249=CARTESIAN_POINT('',(373.946748635116,-329.972007268791,459.95436591896));
#56250=CARTESIAN_POINT('',(373.946748635116,-295.972007268791,459.954365918961));
#56251=CARTESIAN_POINT('',(376.28508690682,-329.972007268791,430.045635184824));
#56252=CARTESIAN_POINT('Origin',(375.115917770968,-329.972007268791,445.000000551892));
#56253=CARTESIAN_POINT('Origin',(375.115917770968,-329.972007268791,445.000000551892));
#56254=CARTESIAN_POINT('Origin',(375.115917770968,-98.9720072687905,445.000000551892));
#56255=CARTESIAN_POINT('',(359.663073558331,-99.4720072687904,443.791859111512));
#56256=CARTESIAN_POINT('Origin',(359.663073558331,-98.9720072687905,443.791859111512));
#56257=CARTESIAN_POINT('Origin',(375.115917770968,-99.4720072687905,445.000000551892));
#56258=CARTESIAN_POINT('Origin',(376.28508690682,-99.4720072687905,430.045635184824));
#56259=CARTESIAN_POINT('',(376.51892073399,-99.4720072687905,427.054762111411));
#56260=CARTESIAN_POINT('Origin',(375.115917770968,-99.4720072687905,445.000000551892));
#56261=CARTESIAN_POINT('Origin',(375.115917770968,-99.7220072687905,445.000000551892));
#56262=CARTESIAN_POINT('',(376.557893038519,-99.9720072687904,426.556283265842));
#56263=CARTESIAN_POINT('',(373.673942503417,-99.9720072687905,463.443717837943));
#56264=CARTESIAN_POINT('Origin',(375.115917770968,-99.9720072687905,445.000000551892));
#56265=CARTESIAN_POINT('Origin',(375.115917770968,-99.9720072687905,445.000000551892));
#56266=CARTESIAN_POINT('',(376.538406886254,-99.7220072687905,426.805522688626));
#56267=CARTESIAN_POINT('Origin',(375.115917770968,-102.22200726879,445.000000551892));
#56268=CARTESIAN_POINT('',(373.673942503417,-104.97200726879,463.443717837943));
#56269=CARTESIAN_POINT('',(373.673942503417,-102.222007268791,463.443717837943));
#56270=CARTESIAN_POINT('',(356.672200484917,-104.97200726879,443.558025284342));
#56271=CARTESIAN_POINT('Origin',(375.115917770968,-104.97200726879,445.000000551892));
#56272=CARTESIAN_POINT('Origin',(375.115917770968,-104.97200726879,445.000000551892));
#56273=CARTESIAN_POINT('Origin',(375.115917770968,-330.472007268791,445.000000551892));
#56274=CARTESIAN_POINT('',(376.207142297763,-330.972007268791,431.042592875962));
#56275=CARTESIAN_POINT('',(376.246114602291,-330.472007268791,430.544114030393));
#56276=CARTESIAN_POINT('Origin',(375.115917770968,-330.972007268791,445.000000551892));
#56277=CARTESIAN_POINT('Origin',(376.28508690682,-330.972007268791,430.045635184824));
#56278=CARTESIAN_POINT('Origin',(376.674809952104,-248.97200726879,425.060846729135));
#56279=CARTESIAN_POINT('',(370.069506932822,-248.97200726879,432.568840603897));
#56280=CARTESIAN_POINT('',(370.693063805276,-248.97200726879,424.593179074794));
#56281=CARTESIAN_POINT('',(382.032999226477,-248.97200726879,433.504175912578));
#56282=CARTESIAN_POINT('Origin',(376.051253079649,-248.97200726879,433.036508258238));
#56283=CARTESIAN_POINT('',(382.584752280163,-248.97200726879,426.446927731622));
#56284=CARTESIAN_POINT('',(382.656556098931,-248.97200726879,425.528514383475));
#56285=CARTESIAN_POINT('Ctrl Pts',(376.674809952104,-254.97200726879,425.060846729135));
#56286=CARTESIAN_POINT('Ctrl Pts',(377.430831413079,-254.97200726879,425.119954349988));
#56287=CARTESIAN_POINT('Ctrl Pts',(378.230432619979,-254.819503761812,425.230011112368));
#56288=CARTESIAN_POINT('Ctrl Pts',(379.689566163776,-254.205705082856,425.515790904349));
#56289=CARTESIAN_POINT('Ctrl Pts',(380.349632476106,-253.744659953595,425.689320091902));
#56290=CARTESIAN_POINT('Ctrl Pts',(381.388651133482,-252.6844780178,426.001391630682));
#56291=CARTESIAN_POINT('Ctrl Pts',(381.838503760257,-252.012958344223,426.160976637205));
#56292=CARTESIAN_POINT('Ctrl Pts',(382.436553503998,-250.536222239647,426.385213930697));
#56293=CARTESIAN_POINT('Ctrl Pts',(382.584752280163,-249.730561776769,426.446927731622));
#56294=CARTESIAN_POINT('Ctrl Pts',(382.584752280163,-248.97200726879,426.446927731622));
#56295=CARTESIAN_POINT('Origin',(382.656556098931,-248.97200726879,425.528514383475));
#56296=CARTESIAN_POINT('',(382.584752280163,-111.97200726879,426.446927731622));
#56297=CARTESIAN_POINT('',(382.584752280163,-180.47200726879,426.446927731622));
#56298=CARTESIAN_POINT('',(382.032999226477,-111.97200726879,433.504175912579));
#56299=CARTESIAN_POINT('',(382.032999226477,-111.97200726879,433.504175912579));
#56300=CARTESIAN_POINT('',(382.656556098931,-111.97200726879,425.528514383475));
#56301=CARTESIAN_POINT('Origin',(370.693063805276,-111.97200726879,424.593179074794));
#56302=CARTESIAN_POINT('',(370.069506932822,-111.97200726879,432.568840603897));
#56303=CARTESIAN_POINT('',(370.693063805276,-111.97200726879,424.593179074794));
#56304=CARTESIAN_POINT('',(370.069506932822,-248.97200726879,432.568840603897));
#56305=CARTESIAN_POINT('Origin',(376.674809952104,-111.97200726879,425.060846729135));
#56306=CARTESIAN_POINT('Ctrl Pts',(382.584752280163,-111.97200726879,426.446927731622));
#56307=CARTESIAN_POINT('Ctrl Pts',(382.584752280163,-111.213452760812,426.446927731622));
#56308=CARTESIAN_POINT('Ctrl Pts',(382.436553503998,-110.407792297934,426.385213930697));
#56309=CARTESIAN_POINT('Ctrl Pts',(381.838503760257,-108.931056193358,426.160976637205));
#56310=CARTESIAN_POINT('Ctrl Pts',(381.388651133482,-108.259536519781,426.001391630682));
#56311=CARTESIAN_POINT('Ctrl Pts',(380.349632476106,-107.199354583986,425.689320091903));
#56312=CARTESIAN_POINT('Ctrl Pts',(379.689566163776,-106.738309454725,425.51579090435));
#56313=CARTESIAN_POINT('Ctrl Pts',(378.230432619979,-106.124510775769,425.230011112368));
#56314=CARTESIAN_POINT('Ctrl Pts',(377.430831413079,-105.97200726879,425.119954349988));
#56315=CARTESIAN_POINT('Ctrl Pts',(376.674809952104,-105.97200726879,425.060846729135));
#56316=CARTESIAN_POINT('Origin',(376.051253079649,-111.97200726879,433.036508258238));
#56317=CARTESIAN_POINT('Origin',(376.051253079649,-180.47200726879,433.036508258238));
#56318=CARTESIAN_POINT('Origin',(375.115917770968,-180.47200726879,445.000000551892));
#56319=CARTESIAN_POINT('Origin',(375.115917770968,-254.97200726879,445.000000551892));
#56320=CARTESIAN_POINT('Origin',(375.115917770968,-105.97200726879,445.000000551892));
#56321=CARTESIAN_POINT('Origin',(375.115917770968,-255.97200726879,445.000000551892));
#56322=CARTESIAN_POINT('',(356.173721639348,-255.47200726879,443.519052979813));
#56323=CARTESIAN_POINT('Origin',(375.115917770968,-255.47200726879,445.000000551892));
#56324=CARTESIAN_POINT('Origin',(356.173721639348,-255.97200726879,443.519052979813));
#56325=CARTESIAN_POINT('Origin',(376.635837647575,-255.47200726879,425.559325574704));
#56326=CARTESIAN_POINT('',(373.595997894361,-255.472007268791,464.440675529081));
#56327=CARTESIAN_POINT('Origin',(375.115917770968,-255.47200726879,445.000000551892));
#56328=CARTESIAN_POINT('Origin',(375.115917770968,-255.22200726879,445.000000551892));
#56329=CARTESIAN_POINT('',(373.576511742096,-255.222007268791,464.689914951866));
#56330=CARTESIAN_POINT('Origin',(375.115917770968,-105.72200726879,445.000000551892));
#56331=CARTESIAN_POINT('',(373.595997894361,-105.47200726879,464.440675529081));
#56332=CARTESIAN_POINT('',(373.576511742096,-105.72200726879,464.689914951866));
#56333=CARTESIAN_POINT('Origin',(375.115917770968,-105.47200726879,445.000000551892));
#56334=CARTESIAN_POINT('Origin',(376.596865343047,-105.47200726879,426.057804420273));
#56335=CARTESIAN_POINT('',(356.173721639348,-105.47200726879,443.519052979813));
#56336=CARTESIAN_POINT('Origin',(375.115917770968,-105.47200726879,445.000000551892));
#56337=CARTESIAN_POINT('Origin',(375.115917770968,-104.97200726879,445.000000551892));
#56338=CARTESIAN_POINT('Origin',(356.173721639348,-104.97200726879,443.519052979813));
#56339=CARTESIAN_POINT('',(0.,0.,0.));
#56340=CARTESIAN_POINT('Origin',(371.018259814925,-255.47200726879,420.650814731371));
#56341=CARTESIAN_POINT('',(370.635385768447,-255.47200726879,425.548000437897));
#56342=CARTESIAN_POINT('',(370.635385768447,-240.47200726879,425.548000437897));
#56343=CARTESIAN_POINT('',(370.635385768447,-240.47200726879,425.548000437897));
#56344=CARTESIAN_POINT('',(371.018259814925,-255.47200726879,420.650814731371));
#56345=CARTESIAN_POINT('',(370.082925320099,-255.47200726879,432.614296615326));
#56346=CARTESIAN_POINT('',(371.018259814925,-240.47200726879,420.650814731371));
#56347=CARTESIAN_POINT('',(371.018259814925,-255.47200726879,420.650814731371));
#56348=CARTESIAN_POINT('',(370.082925320099,-240.47200726879,432.614296615326));
#56349=CARTESIAN_POINT('Origin',(382.98175210858,-255.47200726879,421.586150040052));
#56350=CARTESIAN_POINT('',(382.98175210858,-255.47200726879,421.586150040052));
#56351=CARTESIAN_POINT('',(379.97647207537,-255.47200726879,421.351189841262));
#56352=CARTESIAN_POINT('',(382.98175210858,-240.47200726879,421.586150040052));
#56353=CARTESIAN_POINT('',(382.98175210858,-255.47200726879,421.586150040052));
#56354=CARTESIAN_POINT('',(379.97647207537,-240.47200726879,421.351189841262));
#56355=CARTESIAN_POINT('Origin',(382.358195236125,-255.47200726879,429.561811569155));
#56356=CARTESIAN_POINT('',(382.597461150368,-240.47200726879,426.501458886426));
#56357=CARTESIAN_POINT('',(382.597461150368,-255.47200726879,426.501458886426));
#56358=CARTESIAN_POINT('',(382.597461150368,-240.47200726879,426.501458886426));
#56359=CARTESIAN_POINT('',(381.734639177527,-240.47200726879,437.537462688559));
#56360=CARTESIAN_POINT('',(381.734639177527,-255.47200726879,437.537462688559));
#56361=CARTESIAN_POINT('Origin',(375.100523052509,-240.47200726879,445.043193410383));
#56362=CARTESIAN_POINT('',(345.191792318373,-240.47200726879,442.704855138679));
#56363=CARTESIAN_POINT('Origin',(375.100523052509,-240.47200726879,445.043193410383));
#56364=CARTESIAN_POINT('Origin',(375.100523052509,-240.47200726879,445.043193410383));
#56365=CARTESIAN_POINT('Origin',(375.100523052509,-240.47200726879,445.043193410383));
#56366=CARTESIAN_POINT('Origin',(375.100523052509,-255.47200726879,445.043193410383));
#56367=CARTESIAN_POINT('Origin',(375.100523052509,-240.47200726879,445.043193410383));
#56368=CARTESIAN_POINT('',(345.191792318373,-255.47200726879,442.704855138679));
#56369=CARTESIAN_POINT('Origin',(375.100523052509,-255.47200726879,445.043193410383));
#56370=CARTESIAN_POINT('',(345.191792318373,-240.47200726879,442.704855138679));
#56371=CARTESIAN_POINT('Origin',(375.100523052509,-255.47200726879,445.043193410383));
#56372=CARTESIAN_POINT('',(0.,0.,0.));
#56373=CARTESIAN_POINT('Origin',(263.115917770968,-255.47200726879,445.000000551893));
#56374=CARTESIAN_POINT('',(263.115917770968,-255.47200726879,463.500000551893));
#56375=CARTESIAN_POINT('Origin',(263.115917770968,-255.47200726879,445.000000551893));
#56376=CARTESIAN_POINT('',(263.115917770968,-260.47200726879,463.500000551893));
#56377=CARTESIAN_POINT('',(263.115917770968,-255.47200726879,463.500000551893));
#56378=CARTESIAN_POINT('Origin',(263.115917770968,-260.47200726879,445.000000551893));
#56379=CARTESIAN_POINT('Origin',(263.115917770968,-255.47200726879,445.000000551893));
#56380=CARTESIAN_POINT('',(263.115917770968,-260.47200726879,478.000000551893));
#56381=CARTESIAN_POINT('Origin',(263.115917770968,-260.47200726879,445.000000551893));
#56382=CARTESIAN_POINT('',(263.115917770968,-255.47200726879,478.000000551893));
#56383=CARTESIAN_POINT('',(263.115917770968,-255.47200726879,478.000000551893));
#56384=CARTESIAN_POINT('Origin',(263.115917770968,-255.47200726879,445.000000551893));
#56385=CARTESIAN_POINT('Origin',(263.115917770968,-260.47200726879,445.000000551893));
#56386=CARTESIAN_POINT('Origin',(263.115917770968,-255.47200726879,445.000000551893));
#56387=CARTESIAN_POINT('',(0.,0.,0.));
#56388=CARTESIAN_POINT('',(0.,0.,0.));
#56389=CARTESIAN_POINT('',(0.,0.,0.));
#56390=CARTESIAN_POINT('',(814.82506569565,-465.944014537577,63.6606351219309));
#56391=CARTESIAN_POINT('',(814.82506569565,-435.944014537578,63.6606351219307));
#56392=CARTESIAN_POINT('',(814.82506569565,-375.944014537578,63.6606351219311));
#56393=CARTESIAN_POINT('',(814.82506569565,-405.944014537578,63.6606351219308));
#56394=CARTESIAN_POINT('',(677.568088703695,-360.944014537578,853.648069682691));
#56395=CARTESIAN_POINT('',(677.568088703689,104.999999999998,36.3519314210911));
#56396=CARTESIAN_POINT('',(677.56808870369,74.9999999999979,36.351931421091));
#56397=CARTESIAN_POINT('',(677.568088703689,14.999999999998,36.351931421092));
#56398=CARTESIAN_POINT('',(677.56808870369,44.9999999999979,36.3519314210912));
#56399=CARTESIAN_POINT('',(0.,0.,0.));
#56400=CARTESIAN_POINT('',(64.2413304763198,-7.17648163117701E-12,31.9795795849542));
#56401=CARTESIAN_POINT('',(526.231835541931,-360.944014537579,-3.19744231092045E-12));
#56402=CARTESIAN_POINT('',(112.,154.999999999999,-3.5527136788005E-13));
#56403=CARTESIAN_POINT('',(0.,0.,0.));
#56404=CARTESIAN_POINT('',(0.,0.,0.));
#56405=CARTESIAN_POINT('Origin',(263.115917770968,8.52799273121002,445.000000551893));
#56406=CARTESIAN_POINT('',(263.115917770968,10.52799273121,473.000000551893));
#56407=CARTESIAN_POINT('Origin',(263.115917770968,10.52799273121,445.000000551893));
#56408=CARTESIAN_POINT('',(263.115917770968,8.52799273120999,475.000000551893));
#56409=CARTESIAN_POINT('Origin',(263.115917770968,8.52799273120999,473.000000551893));
#56410=CARTESIAN_POINT('',(263.115917770968,8.52799273121006,415.000000551893));
#56411=CARTESIAN_POINT('Origin',(263.115917770968,8.52799273121002,445.000000551893));
#56412=CARTESIAN_POINT('Origin',(263.115917770968,8.52799273121002,445.000000551893));
#56413=CARTESIAN_POINT('Origin',(263.115917770968,0.527992731210016,445.000000551893));
#56414=CARTESIAN_POINT('',(263.115917770968,2.52799273121005,415.000000551893));
#56415=CARTESIAN_POINT('',(263.115917770968,0.52799273121005,415.000000551893));
#56416=CARTESIAN_POINT('Origin',(263.115917770968,2.52799273121002,445.000000551893));
#56417=CARTESIAN_POINT('Origin',(263.115917770968,10.52799273121,445.000000551893));
#56418=CARTESIAN_POINT('',(276.863644855836,10.52799273121,439.000000551893));
#56419=CARTESIAN_POINT('',(282.115917770968,10.52799273121,439.000000551893));
#56420=CARTESIAN_POINT('',(272.615917770968,10.52799273121,439.000000551893));
#56421=CARTESIAN_POINT('',(282.115917770968,10.52799273121,451.000000551893));
#56422=CARTESIAN_POINT('',(282.115917770968,10.52799273121,448.000000551893));
#56423=CARTESIAN_POINT('',(276.863644855836,10.52799273121,451.000000551893));
#56424=CARTESIAN_POINT('',(269.989781313402,10.52799273121,451.000000551893));
#56425=CARTESIAN_POINT('Origin',(263.115917770968,10.52799273121,445.000000551893));
#56426=CARTESIAN_POINT('Origin',(263.115917770968,2.52799273121002,445.000000551893));
#56427=CARTESIAN_POINT('',(263.115917770968,0.527992731210052,413.000000551893));
#56428=CARTESIAN_POINT('Origin',(263.115917770968,0.527992731210016,445.000000551893));
#56429=CARTESIAN_POINT('Origin',(263.115917770968,2.52799273121005,413.000000551893));
#56430=CARTESIAN_POINT('Origin',(263.115917770968,0.527992731210016,445.000000551893));
#56431=CARTESIAN_POINT('',(199.31403287824,0.52799273121003,454.464116154264));
#56432=CARTESIAN_POINT('',(205.064770108999,0.527992731210025,455.562765644546));
#56433=CARTESIAN_POINT('Origin',(207.471787643001,0.527992731210056,427.363480684421));
#56434=CARTESIAN_POINT('',(205.441455406363,0.527992731210025,457.456490516082));
#56435=CARTESIAN_POINT('Origin',(263.115917770968,0.527992731210016,445.000000551893));
#56436=CARTESIAN_POINT('',(200.54890193992,0.527992731210021,460.672222155654));
#56437=CARTESIAN_POINT('Origin',(218.456648799204,0.52799273120999,482.58810699052));
#56438=CARTESIAN_POINT('',(201.095181820417,0.527992731210021,462.710966424822));
#56439=CARTESIAN_POINT('Origin',(263.115917770968,0.527992731210016,445.000000551893));
#56440=CARTESIAN_POINT('',(206.940123231516,0.527992731210016,463.049594983223));
#56441=CARTESIAN_POINT('Origin',(205.645803107665,0.527992731210047,434.777379981771));
#56442=CARTESIAN_POINT('',(207.560766630536,0.527992731210014,464.877951478433));
#56443=CARTESIAN_POINT('Origin',(263.115917770968,0.527992731210016,445.000000551893));
#56444=CARTESIAN_POINT('',(203.129806843349,0.527992731210012,468.704778462252));
#56445=CARTESIAN_POINT('Origin',(223.744947442398,0.527992731209983,488.095739855457));
#56446=CARTESIAN_POINT('',(203.937522750105,0.52799273121001,470.654777158886));
#56447=CARTESIAN_POINT('Origin',(263.115917770968,0.527992731210016,445.000000551893));
#56448=CARTESIAN_POINT('',(209.776659773475,0.527992731210007,470.227590756887));
#56449=CARTESIAN_POINT('Origin',(204.803148167944,0.527992731210039,442.366191151322));
#56450=CARTESIAN_POINT('',(210.630641893519,0.527992731210005,471.959295189222));
#56451=CARTESIAN_POINT('Origin',(263.115917770968,0.527992731210016,445.000000551893));
#56452=CARTESIAN_POINT('',(206.737090736042,0.527992731210001,476.331739446597));
#56453=CARTESIAN_POINT('Origin',(229.706894303609,0.527992731209974,492.865992672514));
#56454=CARTESIAN_POINT('',(207.792422425951,0.527992731209999,478.159627552356));
#56455=CARTESIAN_POINT('Origin',(263.115917770968,0.527992731210016,445.000000551893));
#56456=CARTESIAN_POINT('',(213.525845808207,0.527992731209999,476.973935467734));
#56457=CARTESIAN_POINT('Origin',(204.958240883485,0.527992731210034,450.000067529947));
#56458=CARTESIAN_POINT('',(214.598554778434,0.527992731209996,478.579357894238));
#56459=CARTESIAN_POINT('Origin',(263.115917770968,0.527992731210016,445.000000551893));
#56460=CARTESIAN_POINT('',(211.309031990467,0.527992731209992,483.422605691655));
#56461=CARTESIAN_POINT('Origin',(236.240478819077,0.527992731209967,496.817245093427));
#56462=CARTESIAN_POINT('',(212.59392244572,0.52799273120999,485.097107534263));
#56463=CARTESIAN_POINT('Origin',(263.115917770968,0.527992731210016,445.000000551893));
#56464=CARTESIAN_POINT('',(218.123531723188,0.52799273120999,483.173197287322));
#56465=CARTESIAN_POINT('Origin',(206.108427574925,0.527992731210025,457.548391376297));
#56466=CARTESIAN_POINT('',(219.396613195705,0.527992731209987,484.62486848517));
#56467=CARTESIAN_POINT('Origin',(263.115917770968,0.527992731210016,445.000000551893));
#56468=CARTESIAN_POINT('',(216.767403424178,0.527992731209983,489.856050510013));
#56469=CARTESIAN_POINT('Origin',(243.233909546292,0.527992731209963,499.881890093779));
#56470=CARTESIAN_POINT('',(218.259867812848,0.527992731209981,491.348514898684));
#56471=CARTESIAN_POINT('Origin',(263.115917770968,0.527992731210016,445.000000551893));
#56472=CARTESIAN_POINT('',(223.491049837692,0.527992731209981,488.719305127157));
#56473=CARTESIAN_POINT('Origin',(208.234028229082,0.527992731210014,464.88200877657));
#56474=CARTESIAN_POINT('',(224.94272103554,0.527992731209981,489.992386599674));
#56475=CARTESIAN_POINT('Origin',(263.115917770968,0.527992731210016,445.000000551893));
#56476=CARTESIAN_POINT('',(223.018810788598,0.527992731209974,495.521995877141));
#56477=CARTESIAN_POINT('Origin',(250.567526946565,0.527992731209956,502.007490747936));
#56478=CARTESIAN_POINT('',(224.693312631207,0.527992731209972,496.806886332395));
#56479=CARTESIAN_POINT('Origin',(263.115917770968,0.527992731210016,445.000000551893));
#56480=CARTESIAN_POINT('',(229.536560428624,0.527992731209974,493.517363544428));
#56481=CARTESIAN_POINT('Origin',(211.298673229435,0.527992731210005,471.875439503784));
#56482=CARTESIAN_POINT('',(231.141982855127,0.527992731209972,494.590072514654));
#56483=CARTESIAN_POINT('Origin',(263.115917770968,0.527992731210016,445.000000551893));
#56484=CARTESIAN_POINT('',(229.956290770506,0.527992731209967,500.323495896911));
#56485=CARTESIAN_POINT('Origin',(258.115850792915,0.527992731209952,503.157677439376));
#56486=CARTESIAN_POINT('',(231.784178876265,0.527992731209965,501.378827586819));
#56487=CARTESIAN_POINT('Origin',(263.115917770968,0.527992731210016,445.000000551893));
#56488=CARTESIAN_POINT('',(236.15662313364,0.527992731209967,497.485276429342));
#56489=CARTESIAN_POINT('Origin',(215.249925650348,0.527992731209996,478.409024019253));
#56490=CARTESIAN_POINT('',(237.888327565975,0.527992731209965,498.339258549387));
#56491=CARTESIAN_POINT('Origin',(263.115917770968,0.527992731210016,445.000000551893));
#56492=CARTESIAN_POINT('',(237.461141163976,0.527992731209959,504.178395572756));
#56493=CARTESIAN_POINT('Origin',(265.74972717154,0.52799273120995,503.312770154917));
#56494=CARTESIAN_POINT('',(239.41113986061,0.527992731209959,504.986111479512));
#56495=CARTESIAN_POINT('Origin',(263.115917770968,0.527992731210016,445.000000551893));
#56496=CARTESIAN_POINT('',(243.237966844429,0.527992731209961,500.555151692326));
#56497=CARTESIAN_POINT('Origin',(220.020178467405,0.527992731209987,484.370970880464));
#56498=CARTESIAN_POINT('',(245.066323339639,0.527992731209961,501.175795091346));
#56499=CARTESIAN_POINT('Origin',(263.115917770968,0.527992731210016,445.000000551893));
#56500=CARTESIAN_POINT('',(245.40495189804,0.527992731209954,507.020736502444));
#56501=CARTESIAN_POINT('Origin',(273.338538341091,0.527992731209947,502.470115215196));
#56502=CARTESIAN_POINT('',(247.443696167208,0.527992731209952,507.567016382941));
#56503=CARTESIAN_POINT('Origin',(263.115917770968,0.527992731210016,445.000000551893));
#56504=CARTESIAN_POINT('',(250.65942780678,0.527992731209956,502.674462916499));
#56505=CARTESIAN_POINT('Origin',(225.527811332342,0.527992731209981,489.659269523657));
#56506=CARTESIAN_POINT('',(252.553152678316,0.527992731209954,503.051148213862));
#56507=CARTESIAN_POINT('Origin',(263.115917770968,0.527992731210016,445.000000551893));
#56508=CARTESIAN_POINT('',(253.651802168598,0.527992731209947,508.801885444622));
#56509=CARTESIAN_POINT('Origin',(280.752437638441,0.527992731209947,500.64413067986));
#56510=CARTESIAN_POINT('',(255.744408530607,0.527992731209947,509.077382298647));
#56511=CARTESIAN_POINT('Origin',(263.115917770968,0.527992731210016,445.000000551893));
#56512=CARTESIAN_POINT('',(258.29402276601,0.527992731209952,503.806948099231));
#56513=CARTESIAN_POINT('Origin',(231.678587119835,0.527992731209972,494.183435692855));
#56514=CARTESIAN_POINT('',(260.22071385628,0.527992731209952,503.933230105063));
#56515=CARTESIAN_POINT('Origin',(263.115917770968,0.527992731210016,445.000000551893));
#56516=CARTESIAN_POINT('',(262.06058608106,0.527992731209945,509.49136644706));
#56517=CARTESIAN_POINT('Origin',(287.864571191092,0.527992731209947,497.866059650567));
#56518=CARTESIAN_POINT('',(264.171249460877,0.527992731209943,509.49136644706));
#56519=CARTESIAN_POINT('Origin',(263.115917770968,0.527992731210016,445.000000551893));
#56520=CARTESIAN_POINT('',(266.011121685657,0.52799273120995,503.933230105063));
#56521=CARTESIAN_POINT('Origin',(238.367264350845,0.527992731209965,497.866059650567));
#56522=CARTESIAN_POINT('',(267.937812775927,0.52799273120995,503.806948099231));
#56523=CARTESIAN_POINT('Origin',(263.115917770968,0.527992731210016,445.000000551893));
#56524=CARTESIAN_POINT('',(270.48742701133,0.527992731209941,509.077382298647));
#56525=CARTESIAN_POINT('Origin',(294.553248422101,0.52799273120995,494.183435692855));
#56526=CARTESIAN_POINT('',(272.580033373339,0.527992731209941,508.801885444621));
#56527=CARTESIAN_POINT('Origin',(263.115917770968,0.527992731210016,445.000000551893));
#56528=CARTESIAN_POINT('',(273.678682863621,0.527992731209947,503.051148213862));
#56529=CARTESIAN_POINT('Origin',(245.479397903496,0.527992731209961,500.64413067986));
#56530=CARTESIAN_POINT('',(275.572407735157,0.527992731209947,502.674462916499));
#56531=CARTESIAN_POINT('Origin',(263.115917770968,0.527992731210016,445.000000551893));
#56532=CARTESIAN_POINT('',(278.788139374729,0.527992731209941,507.567016382941));
#56533=CARTESIAN_POINT('Origin',(300.704024209595,0.527992731209952,489.659269523657));
#56534=CARTESIAN_POINT('',(280.826883643897,0.527992731209941,507.020736502444));
#56535=CARTESIAN_POINT('Origin',(263.115917770968,0.527992731210016,445.000000551893));
#56536=CARTESIAN_POINT('',(281.165512202298,0.527992731209947,501.175795091345));
#56537=CARTESIAN_POINT('Origin',(252.893297200846,0.527992731209956,502.470115215196));
#56538=CARTESIAN_POINT('',(282.993868697508,0.527992731209947,500.555151692326));
#56539=CARTESIAN_POINT('Origin',(263.115917770968,0.527992731210016,445.000000551893));
#56540=CARTESIAN_POINT('',(286.820695681327,0.527992731209941,504.986111479512));
#56541=CARTESIAN_POINT('Origin',(306.211657074532,0.527992731209956,484.370970880463));
#56542=CARTESIAN_POINT('',(288.770694377961,0.527992731209941,504.178395572756));
#56543=CARTESIAN_POINT('Origin',(263.115917770968,0.527992731210016,445.000000551893));
#56544=CARTESIAN_POINT('',(288.343507975962,0.527992731209947,498.339258549386));
#56545=CARTESIAN_POINT('Origin',(260.482108370397,0.527992731209952,503.312770154917));
#56546=CARTESIAN_POINT('',(290.075212408297,0.527992731209947,497.485276429342));
#56547=CARTESIAN_POINT('Origin',(263.115917770968,0.527992731210016,445.000000551893));
#56548=CARTESIAN_POINT('',(294.447656665672,0.527992731209941,501.378827586819));
#56549=CARTESIAN_POINT('Origin',(310.981909891589,0.527992731209961,478.409024019252));
#56550=CARTESIAN_POINT('',(296.275544771431,0.527992731209943,500.32349589691));
#56551=CARTESIAN_POINT('Origin',(263.115917770968,0.527992731210016,445.000000551893));
#56552=CARTESIAN_POINT('',(295.089852686809,0.52799273120995,494.590072514654));
#56553=CARTESIAN_POINT('Origin',(268.115984749022,0.52799273120995,503.157677439376));
#56554=CARTESIAN_POINT('',(296.695275113313,0.52799273120995,493.517363544428));
#56555=CARTESIAN_POINT('Origin',(263.115917770968,0.527992731210016,445.000000551893));
#56556=CARTESIAN_POINT('',(301.53852291073,0.527992731209945,496.806886332394));
#56557=CARTESIAN_POINT('Origin',(314.933162312502,0.527992731209967,471.875439503784));
#56558=CARTESIAN_POINT('',(303.213024753338,0.527992731209945,495.521995877141));
#56559=CARTESIAN_POINT('Origin',(263.115917770968,0.527992731210016,445.000000551893));
#56560=CARTESIAN_POINT('',(301.289114506397,0.527992731209952,489.992386599673));
#56561=CARTESIAN_POINT('Origin',(275.664308595372,0.527992731209947,502.007490747936));
#56562=CARTESIAN_POINT('',(302.740785704245,0.527992731209952,488.719305127157));
#56563=CARTESIAN_POINT('Origin',(263.115917770968,0.527992731210016,445.000000551893));
#56564=CARTESIAN_POINT('',(307.971967729088,0.527992731209947,491.348514898683));
#56565=CARTESIAN_POINT('Origin',(317.997807312854,0.527992731209974,464.882008776569));
#56566=CARTESIAN_POINT('',(309.464432117759,0.52799273120995,489.856050510013));
#56567=CARTESIAN_POINT('Origin',(263.115917770968,0.527992731210016,445.000000551893));
#56568=CARTESIAN_POINT('',(306.835222346232,0.527992731209956,484.624868485169));
#56569=CARTESIAN_POINT('Origin',(282.997925995645,0.527992731209947,499.881890093779));
#56570=CARTESIAN_POINT('',(308.108303818749,0.527992731209956,483.173197287322));
#56571=CARTESIAN_POINT('Origin',(263.115917770968,0.527992731210016,445.000000551893));
#56572=CARTESIAN_POINT('',(313.637913096216,0.527992731209952,485.097107534263));
#56573=CARTESIAN_POINT('Origin',(320.123407967011,0.527992731209981,457.548391376296));
#56574=CARTESIAN_POINT('',(314.92280355147,0.527992731209954,483.422605691655));
#56575=CARTESIAN_POINT('Origin',(263.115917770968,0.527992731210016,445.000000551893));
#56576=CARTESIAN_POINT('',(311.633280763503,0.527992731209961,478.579357894237));
#56577=CARTESIAN_POINT('Origin',(289.99135672286,0.527992731209947,496.817245093426));
#56578=CARTESIAN_POINT('',(312.705989733729,0.527992731209963,476.973935467734));
#56579=CARTESIAN_POINT('Origin',(263.115917770968,0.527992731210016,445.000000551893));
#56580=CARTESIAN_POINT('',(318.439413115986,0.527992731209959,478.159627552356));
#56581=CARTESIAN_POINT('Origin',(321.273594658451,0.52799273120999,450.000067529946));
#56582=CARTESIAN_POINT('',(319.494744805894,0.527992731209961,476.331739446597));
#56583=CARTESIAN_POINT('Origin',(263.115917770968,0.527992731210016,445.000000551893));
#56584=CARTESIAN_POINT('',(315.601193648417,0.527992731209967,471.959295189222));
#56585=CARTESIAN_POINT('Origin',(296.524941238328,0.52799273120995,492.865992672513));
#56586=CARTESIAN_POINT('',(316.455175768462,0.527992731209967,470.227590756886));
#56587=CARTESIAN_POINT('Origin',(263.115917770968,0.527992731210016,445.000000551893));
#56588=CARTESIAN_POINT('',(322.294312791831,0.527992731209965,470.654777158885));
#56589=CARTESIAN_POINT('Origin',(321.428687373992,0.527992731209999,442.366191151322));
#56590=CARTESIAN_POINT('',(323.102028698587,0.527992731209967,468.704778462251));
#56591=CARTESIAN_POINT('Origin',(263.115917770968,0.527992731210016,445.000000551893));
#56592=CARTESIAN_POINT('',(318.671068911401,0.527992731209974,464.877951478433));
#56593=CARTESIAN_POINT('Origin',(302.486888099539,0.527992731209954,488.095739855457));
#56594=CARTESIAN_POINT('',(319.291712310421,0.527992731209976,463.049594983222));
#56595=CARTESIAN_POINT('Origin',(263.115917770968,0.527992731210016,445.000000551893));
#56596=CARTESIAN_POINT('',(325.136653721519,0.527992731209974,462.710966424821));
#56597=CARTESIAN_POINT('Origin',(320.586032434271,0.527992731210007,434.77737998177));
#56598=CARTESIAN_POINT('',(325.682933602016,0.527992731209976,460.672222155653));
#56599=CARTESIAN_POINT('Origin',(263.115917770968,0.527992731210016,445.000000551893));
#56600=CARTESIAN_POINT('',(320.790380135574,0.527992731209981,457.456490516081));
#56601=CARTESIAN_POINT('Origin',(307.775186742732,0.527992731209959,482.588106990519));
#56602=CARTESIAN_POINT('',(321.167065432937,0.527992731209983,455.562765644545));
#56603=CARTESIAN_POINT('Origin',(263.115917770968,0.527992731210016,445.000000551893));
#56604=CARTESIAN_POINT('',(326.917802663697,0.527992731209983,454.464116154263));
#56605=CARTESIAN_POINT('Origin',(318.760047898935,0.527992731210016,427.36348068442));
#56606=CARTESIAN_POINT('',(327.193299517722,0.527992731209985,452.371509792254));
#56607=CARTESIAN_POINT('Origin',(263.115917770968,0.527992731210016,445.000000551893));
#56608=CARTESIAN_POINT('',(321.922865318307,0.52799273120999,449.821895556851));
#56609=CARTESIAN_POINT('Origin',(312.29935291193,0.527992731209963,476.437331203026));
#56610=CARTESIAN_POINT('',(322.049147324138,0.527992731209992,447.895204466581));
#56611=CARTESIAN_POINT('Origin',(263.115917770968,0.527992731210016,445.000000551893));
#56612=CARTESIAN_POINT('',(327.607283666135,0.527992731209992,446.055332241801));
#56613=CARTESIAN_POINT('Origin',(315.981976869642,0.527992731210025,420.251347131769));
#56614=CARTESIAN_POINT('',(327.607283666135,0.527992731209994,443.944668861984));
#56615=CARTESIAN_POINT('Origin',(263.115917770968,0.527992731210016,445.000000551893));
#56616=CARTESIAN_POINT('',(322.049147324138,0.527992731209999,442.104796637205));
#56617=CARTESIAN_POINT('Origin',(315.981976869642,0.52799273120997,469.748653972016));
#56618=CARTESIAN_POINT('',(321.922865318307,0.527992731210001,440.178105546934));
#56619=CARTESIAN_POINT('Origin',(263.115917770968,0.527992731210016,445.000000551893));
#56620=CARTESIAN_POINT('',(327.193299517722,0.527992731210001,437.628491311531));
#56621=CARTESIAN_POINT('Origin',(312.29935291193,0.527992731210034,413.56266990076));
#56622=CARTESIAN_POINT('',(326.917802663696,0.527992731210003,435.535884949522));
#56623=CARTESIAN_POINT('Origin',(263.115917770968,0.527992731210016,445.000000551893));
#56624=CARTESIAN_POINT('',(321.167065432937,0.527992731210007,434.43723545924));
#56625=CARTESIAN_POINT('Origin',(318.760047898935,0.527992731209976,462.636520419365));
#56626=CARTESIAN_POINT('',(320.790380135574,0.52799273121001,432.543510587704));
#56627=CARTESIAN_POINT('Origin',(263.115917770968,0.527992731210016,445.000000551893));
#56628=CARTESIAN_POINT('',(325.682933602016,0.527992731210012,429.327778948132));
#56629=CARTESIAN_POINT('Origin',(307.775186742732,0.527992731210043,407.411894113266));
#56630=CARTESIAN_POINT('',(325.136653721519,0.527992731210014,427.289034678965));
#56631=CARTESIAN_POINT('Origin',(263.115917770968,0.527992731210016,445.000000551893));
#56632=CARTESIAN_POINT('',(319.29171231042,0.527992731210016,426.950406120563));
#56633=CARTESIAN_POINT('Origin',(320.586032434271,0.527992731209983,455.222621122015));
#56634=CARTESIAN_POINT('',(318.671068911401,0.527992731210016,425.122049625353));
#56635=CARTESIAN_POINT('Origin',(263.115917770968,0.527992731210016,445.000000551893));
#56636=CARTESIAN_POINT('',(323.102028698587,0.527992731210021,421.295222641534));
#56637=CARTESIAN_POINT('Origin',(302.486888099538,0.527992731210052,401.904261248329));
#56638=CARTESIAN_POINT('',(322.294312791831,0.527992731210025,419.345223944901));
#56639=CARTESIAN_POINT('Origin',(263.115917770968,0.527992731210016,445.000000551893));
#56640=CARTESIAN_POINT('',(316.455175768461,0.527992731210025,419.772410346899));
#56641=CARTESIAN_POINT('Origin',(321.428687373992,0.527992731209992,447.633809952464));
#56642=CARTESIAN_POINT('',(315.601193648417,0.527992731210025,418.040705914564));
#56643=CARTESIAN_POINT('Origin',(263.115917770968,0.527992731210016,445.000000551893));
#56644=CARTESIAN_POINT('',(319.494744805894,0.52799273121003,413.668261657189));
#56645=CARTESIAN_POINT('Origin',(296.524941238327,0.527992731210056,397.134008431272));
#56646=CARTESIAN_POINT('',(318.439413115985,0.527992731210034,411.84037355143));
#56647=CARTESIAN_POINT('Origin',(263.115917770968,0.527992731210016,445.000000551893));
#56648=CARTESIAN_POINT('',(312.705989733729,0.527992731210034,413.026065636052));
#56649=CARTESIAN_POINT('Origin',(321.273594658451,0.527992731210001,439.999933573839));
#56650=CARTESIAN_POINT('',(311.633280763503,0.527992731210034,411.420643209548));
#56651=CARTESIAN_POINT('Origin',(263.115917770968,0.527992731210016,445.000000551893));
#56652=CARTESIAN_POINT('',(314.92280355147,0.527992731210039,406.577395412131));
#56653=CARTESIAN_POINT('Origin',(289.991356722859,0.527992731210065,393.18275601036));
#56654=CARTESIAN_POINT('',(313.637913096216,0.527992731210043,404.902893569523));
#56655=CARTESIAN_POINT('Origin',(263.115917770968,0.527992731210016,445.000000551893));
#56656=CARTESIAN_POINT('',(308.108303818748,0.527992731210043,406.826803816464));
#56657=CARTESIAN_POINT('Origin',(320.123407967011,0.52799273121001,432.451609727489));
#56658=CARTESIAN_POINT('',(306.835222346232,0.527992731210043,405.375132618617));
#56659=CARTESIAN_POINT('Origin',(263.115917770968,0.527992731210016,445.000000551893));
#56660=CARTESIAN_POINT('',(309.464432117758,0.527992731210047,400.143950593773));
#56661=CARTESIAN_POINT('Origin',(282.997925995644,0.52799273121007,390.118111010007));
#56662=CARTESIAN_POINT('',(307.971967729088,0.527992731210052,398.651486205102));
#56663=CARTESIAN_POINT('Origin',(263.115917770968,0.527992731210016,445.000000551893));
#56664=CARTESIAN_POINT('',(302.740785704244,0.527992731210052,401.280695976629));
#56665=CARTESIAN_POINT('Origin',(317.997807312854,0.527992731210016,425.117992327216));
#56666=CARTESIAN_POINT('',(301.289114506397,0.527992731210052,400.007614504112));
#56667=CARTESIAN_POINT('Origin',(263.115917770968,0.527992731210016,445.000000551893));
#56668=CARTESIAN_POINT('',(303.213024753338,0.527992731210056,394.478005226645));
#56669=CARTESIAN_POINT('Origin',(275.664308595371,0.527992731210074,387.99251035585));
#56670=CARTESIAN_POINT('',(301.53852291073,0.527992731210061,393.193114771391));
#56671=CARTESIAN_POINT('Origin',(263.115917770968,0.527992731210016,445.000000551893));
#56672=CARTESIAN_POINT('',(296.695275113313,0.527992731210056,396.482637559358));
#56673=CARTESIAN_POINT('Origin',(314.933162312501,0.52799273121003,418.124561600002));
#56674=CARTESIAN_POINT('',(295.089852686809,0.527992731210061,395.409928589132));
#56675=CARTESIAN_POINT('Origin',(263.115917770968,0.527992731210016,445.000000551893));
#56676=CARTESIAN_POINT('',(296.275544771431,0.527992731210065,389.676505206875));
#56677=CARTESIAN_POINT('Origin',(268.115984749021,0.527992731210079,386.84232366441));
#56678=CARTESIAN_POINT('',(294.447656665672,0.52799273121007,388.621173516967));
#56679=CARTESIAN_POINT('Origin',(263.115917770968,0.527992731210016,445.000000551893));
#56680=CARTESIAN_POINT('',(290.075212408297,0.527992731210065,392.514724674444));
#56681=CARTESIAN_POINT('Origin',(310.981909891589,0.527992731210034,411.590977084533));
#56682=CARTESIAN_POINT('',(288.343507975962,0.527992731210065,391.6607425544));
#56683=CARTESIAN_POINT('Origin',(263.115917770968,0.527992731210016,445.000000551893));
#56684=CARTESIAN_POINT('',(288.77069437796,0.527992731210074,385.82160553103));
#56685=CARTESIAN_POINT('Origin',(260.482108370397,0.527992731210083,386.687230948869));
#56686=CARTESIAN_POINT('',(286.820695681326,0.527992731210074,385.013889624274));
#56687=CARTESIAN_POINT('Origin',(263.115917770968,0.527992731210016,445.000000551893));
#56688=CARTESIAN_POINT('',(282.993868697508,0.52799273121007,389.44484941146));
#56689=CARTESIAN_POINT('Origin',(306.211657074532,0.527992731210043,405.629030223323));
#56690=CARTESIAN_POINT('',(281.165512202297,0.527992731210074,388.824206012441));
#56691=CARTESIAN_POINT('Origin',(263.115917770968,0.527992731210016,445.000000551893));
#56692=CARTESIAN_POINT('',(280.826883643896,0.527992731210079,382.979264601342));
#56693=CARTESIAN_POINT('Origin',(252.893297200846,0.527992731210083,387.52988588859));
#56694=CARTESIAN_POINT('',(278.788139374728,0.527992731210079,382.432984720845));
#56695=CARTESIAN_POINT('Origin',(263.115917770968,0.527992731210016,445.000000551893));
#56696=CARTESIAN_POINT('',(275.572407735156,0.527992731210079,387.325538187287));
#56697=CARTESIAN_POINT('Origin',(300.704024209595,0.527992731210052,400.340731580129));
#56698=CARTESIAN_POINT('',(273.67868286362,0.527992731210079,386.948852889924));
#56699=CARTESIAN_POINT('Origin',(263.115917770968,0.527992731210016,445.000000551893));
#56700=CARTESIAN_POINT('',(272.580033373339,0.527992731210083,381.198115659165));
#56701=CARTESIAN_POINT('Origin',(245.479397903495,0.527992731210083,389.355870423926));
#56702=CARTESIAN_POINT('',(270.487427011329,0.527992731210087,380.922618805139));
#56703=CARTESIAN_POINT('Origin',(263.115917770968,0.527992731210016,445.000000551893));
#56704=CARTESIAN_POINT('',(267.937812775926,0.527992731210079,386.193053004555));
#56705=CARTESIAN_POINT('Origin',(294.553248422101,0.527992731210061,395.816565410931));
#56706=CARTESIAN_POINT('',(266.011121685656,0.527992731210083,386.066770998723));
#56707=CARTESIAN_POINT('Origin',(263.115917770968,0.527992731210016,445.000000551893));
#56708=CARTESIAN_POINT('',(264.171249460876,0.527992731210087,380.508634656726));
#56709=CARTESIAN_POINT('Origin',(238.367264350844,0.527992731210083,392.133941453219));
#56710=CARTESIAN_POINT('',(262.060586081059,0.527992731210087,380.508634656726));
#56711=CARTESIAN_POINT('Origin',(263.115917770968,0.527992731210016,445.000000551893));
#56712=CARTESIAN_POINT('',(260.22071385628,0.527992731210083,386.066770998723));
#56713=CARTESIAN_POINT('Origin',(287.864571191091,0.527992731210065,392.133941453219));
#56714=CARTESIAN_POINT('',(258.294022766009,0.527992731210083,386.193053004555));
#56715=CARTESIAN_POINT('Origin',(263.115917770968,0.527992731210016,445.000000551893));
#56716=CARTESIAN_POINT('',(255.744408530606,0.527992731210092,380.922618805139));
#56717=CARTESIAN_POINT('Origin',(231.678587119835,0.527992731210083,395.816565410931));
#56718=CARTESIAN_POINT('',(253.651802168597,0.527992731210092,381.198115659165));
#56719=CARTESIAN_POINT('Origin',(263.115917770968,0.527992731210016,445.000000551893));
#56720=CARTESIAN_POINT('',(252.553152678315,0.527992731210087,386.948852889924));
#56721=CARTESIAN_POINT('Origin',(280.75243763844,0.527992731210074,389.355870423926));
#56722=CARTESIAN_POINT('',(250.659427806779,0.527992731210087,387.325538187287));
#56723=CARTESIAN_POINT('Origin',(263.115917770968,0.527992731210016,445.000000551893));
#56724=CARTESIAN_POINT('',(247.443696167207,0.527992731210092,382.432984720845));
#56725=CARTESIAN_POINT('Origin',(225.527811332341,0.527992731210079,400.340731580129));
#56726=CARTESIAN_POINT('',(245.40495189804,0.527992731210092,382.979264601342));
#56727=CARTESIAN_POINT('Origin',(263.115917770968,0.527992731210016,445.000000551893));
#56728=CARTESIAN_POINT('',(245.066323339638,0.527992731210087,388.824206012441));
#56729=CARTESIAN_POINT('Origin',(273.33853834109,0.527992731210079,387.52988588859));
#56730=CARTESIAN_POINT('',(243.237966844428,0.527992731210087,389.44484941146));
#56731=CARTESIAN_POINT('Origin',(263.115917770968,0.527992731210016,445.000000551893));
#56732=CARTESIAN_POINT('',(239.411139860609,0.527992731210092,385.013889624274));
#56733=CARTESIAN_POINT('Origin',(220.020178467404,0.527992731210074,405.629030223323));
#56734=CARTESIAN_POINT('',(237.461141163976,0.527992731210092,385.82160553103));
#56735=CARTESIAN_POINT('Origin',(263.115917770968,0.527992731210016,445.000000551893));
#56736=CARTESIAN_POINT('',(237.888327565974,0.527992731210087,391.6607425544));
#56737=CARTESIAN_POINT('Origin',(265.749727171539,0.527992731210079,386.687230948869));
#56738=CARTESIAN_POINT('',(236.156623133639,0.527992731210083,392.514724674444));
#56739=CARTESIAN_POINT('Origin',(263.115917770968,0.527992731210016,445.000000551893));
#56740=CARTESIAN_POINT('',(231.784178876264,0.527992731210092,388.621173516967));
#56741=CARTESIAN_POINT('Origin',(215.249925650347,0.52799273121007,411.590977084534));
#56742=CARTESIAN_POINT('',(229.956290770505,0.527992731210092,389.676505206876));
#56743=CARTESIAN_POINT('Origin',(263.115917770968,0.527992731210016,445.000000551893));
#56744=CARTESIAN_POINT('',(231.141982855127,0.527992731210083,395.409928589132));
#56745=CARTESIAN_POINT('Origin',(258.115850792914,0.527992731210083,386.84232366441));
#56746=CARTESIAN_POINT('',(229.536560428623,0.527992731210083,396.482637559359));
#56747=CARTESIAN_POINT('Origin',(263.115917770968,0.527992731210016,445.000000551893));
#56748=CARTESIAN_POINT('',(224.693312631206,0.527992731210087,393.193114771392));
#56749=CARTESIAN_POINT('Origin',(211.298673229435,0.527992731210065,418.124561600002));
#56750=CARTESIAN_POINT('',(223.018810788598,0.527992731210087,394.478005226645));
#56751=CARTESIAN_POINT('Origin',(263.115917770968,0.527992731210016,445.000000551893));
#56752=CARTESIAN_POINT('',(224.942721035539,0.527992731210079,400.007614504113));
#56753=CARTESIAN_POINT('Origin',(250.567526946565,0.527992731210083,387.99251035585));
#56754=CARTESIAN_POINT('',(223.491049837692,0.527992731210079,401.280695976629));
#56755=CARTESIAN_POINT('Origin',(263.115917770968,0.527992731210016,445.000000551893));
#56756=CARTESIAN_POINT('',(218.259867812848,0.527992731210083,398.651486205103));
#56757=CARTESIAN_POINT('Origin',(208.234028229082,0.527992731210061,425.117992327217));
#56758=CARTESIAN_POINT('',(216.767403424177,0.527992731210083,400.143950593773));
#56759=CARTESIAN_POINT('Origin',(263.115917770968,0.527992731210016,445.000000551893));
#56760=CARTESIAN_POINT('',(219.396613195704,0.527992731210079,405.375132618617));
#56761=CARTESIAN_POINT('Origin',(243.233909546291,0.527992731210083,390.118111010007));
#56762=CARTESIAN_POINT('',(218.123531723188,0.527992731210074,406.826803816464));
#56763=CARTESIAN_POINT('Origin',(263.115917770968,0.527992731210016,445.000000551893));
#56764=CARTESIAN_POINT('',(212.59392244572,0.527992731210079,404.902893569523));
#56765=CARTESIAN_POINT('Origin',(206.108427574925,0.527992731210052,432.45160972749));
#56766=CARTESIAN_POINT('',(211.309031990466,0.527992731210079,406.577395412131));
#56767=CARTESIAN_POINT('Origin',(263.115917770968,0.527992731210016,445.000000551893));
#56768=CARTESIAN_POINT('',(214.598554778433,0.52799273121007,411.420643209549));
#56769=CARTESIAN_POINT('Origin',(236.240478819077,0.527992731210083,393.18275601036));
#56770=CARTESIAN_POINT('',(213.525845808207,0.52799273121007,413.026065636052));
#56771=CARTESIAN_POINT('Origin',(263.115917770968,0.527992731210016,445.000000551893));
#56772=CARTESIAN_POINT('',(207.79242242595,0.527992731210074,411.840373551431));
#56773=CARTESIAN_POINT('Origin',(204.958240883485,0.527992731210043,439.99993357384));
#56774=CARTESIAN_POINT('',(206.737090736042,0.527992731210074,413.668261657189));
#56775=CARTESIAN_POINT('Origin',(263.115917770968,0.527992731210016,445.000000551893));
#56776=CARTESIAN_POINT('',(210.630641893519,0.527992731210065,418.040705914564));
#56777=CARTESIAN_POINT('Origin',(229.706894303608,0.527992731210083,397.134008431273));
#56778=CARTESIAN_POINT('',(209.776659773475,0.527992731210065,419.7724103469));
#56779=CARTESIAN_POINT('Origin',(263.115917770968,0.527992731210016,445.000000551893));
#56780=CARTESIAN_POINT('',(203.937522750105,0.527992731210065,419.345223944901));
#56781=CARTESIAN_POINT('Origin',(204.803148167944,0.527992731210034,447.633809952465));
#56782=CARTESIAN_POINT('',(203.129806843349,0.527992731210065,421.295222641535));
#56783=CARTESIAN_POINT('Origin',(263.115917770968,0.527992731210016,445.000000551893));
#56784=CARTESIAN_POINT('',(207.560766630535,0.527992731210061,425.122049625353));
#56785=CARTESIAN_POINT('Origin',(223.744947442398,0.527992731210079,401.904261248329));
#56786=CARTESIAN_POINT('',(206.940123231516,0.527992731210056,426.950406120564));
#56787=CARTESIAN_POINT('Origin',(263.115917770968,0.527992731210016,445.000000551893));
#56788=CARTESIAN_POINT('',(201.095181820417,0.527992731210061,427.289034678965));
#56789=CARTESIAN_POINT('Origin',(205.645803107665,0.527992731210025,455.222621122016));
#56790=CARTESIAN_POINT('',(200.54890193992,0.527992731210056,429.327778948133));
#56791=CARTESIAN_POINT('Origin',(263.115917770968,0.527992731210016,445.000000551893));
#56792=CARTESIAN_POINT('',(205.441455406362,0.527992731210052,432.543510587705));
#56793=CARTESIAN_POINT('Origin',(218.456648799204,0.527992731210074,407.411894113266));
#56794=CARTESIAN_POINT('',(205.064770108999,0.527992731210047,434.437235459241));
#56795=CARTESIAN_POINT('Origin',(263.115917770968,0.527992731210016,445.000000551893));
#56796=CARTESIAN_POINT('',(199.31403287824,0.527992731210052,435.535884949523));
#56797=CARTESIAN_POINT('Origin',(207.471787643001,0.527992731210016,462.636520419366));
#56798=CARTESIAN_POINT('',(199.038536024214,0.527992731210047,437.628491311532));
#56799=CARTESIAN_POINT('Origin',(263.115917770968,0.527992731210016,445.000000551893));
#56800=CARTESIAN_POINT('',(204.30897022363,0.527992731210043,440.178105546935));
#56801=CARTESIAN_POINT('Origin',(213.932482630006,0.52799273121007,413.56266990076));
#56802=CARTESIAN_POINT('',(204.182688217798,0.527992731210043,442.104796637205));
#56803=CARTESIAN_POINT('Origin',(263.115917770968,0.527992731210016,445.000000551893));
#56804=CARTESIAN_POINT('',(198.624551875801,0.527992731210043,443.944668861985));
#56805=CARTESIAN_POINT('Origin',(210.249858672294,0.527992731210007,469.748653972017));
#56806=CARTESIAN_POINT('',(198.624551875801,0.527992731210039,446.055332241802));
#56807=CARTESIAN_POINT('Origin',(263.115917770968,0.527992731210016,445.000000551893));
#56808=CARTESIAN_POINT('',(204.182688217798,0.527992731210034,447.895204466582));
#56809=CARTESIAN_POINT('Origin',(210.249858672294,0.527992731210065,420.25134713177));
#56810=CARTESIAN_POINT('',(204.30897022363,0.527992731210034,449.821895556852));
#56811=CARTESIAN_POINT('Origin',(263.115917770968,0.527992731210016,445.000000551893));
#56812=CARTESIAN_POINT('',(199.038536024214,0.52799273121003,452.371509792255));
#56813=CARTESIAN_POINT('Origin',(213.932482630006,0.527992731209999,476.437331203026));
#56814=CARTESIAN_POINT('Origin',(263.115917770968,0.527992731210016,445.000000551893));
#56815=CARTESIAN_POINT('Origin',(282.115917770968,0.527992731210016,439.000000551893));
#56816=CARTESIAN_POINT('',(282.115917770968,-19.47200726879,451.000000551893));
#56817=CARTESIAN_POINT('',(282.115917770968,-19.47200726879,439.000000551893));
#56818=CARTESIAN_POINT('',(282.115917770968,-19.47200726879,442.000000551893));
#56819=CARTESIAN_POINT('',(282.115917770968,0.527992731210003,451.000000551893));
#56820=CARTESIAN_POINT('',(282.115917770968,0.527992731210016,439.000000551893));
#56821=CARTESIAN_POINT('Origin',(274.115917770968,0.527992731210021,439.000000551893));
#56822=CARTESIAN_POINT('',(276.863644855836,-19.47200726879,439.000000551893));
#56823=CARTESIAN_POINT('',(268.615917770968,-19.47200726879,439.000000551893));
#56824=CARTESIAN_POINT('',(276.863644855836,0.527992731210016,439.000000551893));
#56825=CARTESIAN_POINT('Origin',(263.115917770968,0.527992731210016,445.000000551893));
#56826=CARTESIAN_POINT('',(276.863644855836,-19.47200726879,451.000000551893));
#56827=CARTESIAN_POINT('Origin',(263.115917770968,-19.47200726879,445.000000551893));
#56828=CARTESIAN_POINT('',(276.863644855836,0.527992731210005,451.000000551893));
#56829=CARTESIAN_POINT('Origin',(282.115917770968,0.527992731210003,451.000000551893));
#56830=CARTESIAN_POINT('',(272.615917770968,-19.47200726879,451.000000551893));
#56831=CARTESIAN_POINT('Origin',(263.115917770968,-19.47200726879,445.000000551893));
#56832=CARTESIAN_POINT('',(205.064770108999,-19.47200726879,455.562765644546));
#56833=CARTESIAN_POINT('',(205.064770108999,-19.47200726879,455.562765644546));
#56834=CARTESIAN_POINT('',(205.441455406362,-19.47200726879,457.456490516082));
#56835=CARTESIAN_POINT('Origin',(263.115917770968,-19.47200726879,445.000000551893));
#56836=CARTESIAN_POINT('',(205.441455406362,-19.47200726879,457.456490516082));
#56837=CARTESIAN_POINT('Origin',(218.456648799204,-19.47200726879,482.58810699052));
#56838=CARTESIAN_POINT('',(200.54890193992,-19.47200726879,460.672222155654));
#56839=CARTESIAN_POINT('Origin',(218.456648799204,-19.47200726879,482.58810699052));
#56840=CARTESIAN_POINT('',(200.54890193992,-19.47200726879,460.672222155654));
#56841=CARTESIAN_POINT('Origin',(207.471787643001,-19.4720072687899,427.363480684421));
#56842=CARTESIAN_POINT('',(199.31403287824,-19.47200726879,454.464116154264));
#56843=CARTESIAN_POINT('',(199.31403287824,-19.47200726879,454.464116154264));
#56844=CARTESIAN_POINT('Origin',(207.471787643001,-19.4720072687899,427.363480684421));
#56845=CARTESIAN_POINT('Origin',(263.115917770968,-19.47200726879,445.000000551893));
#56846=CARTESIAN_POINT('',(206.940123231516,-19.47200726879,463.049594983223));
#56847=CARTESIAN_POINT('',(206.940123231516,-19.47200726879,463.049594983223));
#56848=CARTESIAN_POINT('',(207.560766630536,-19.47200726879,464.877951478433));
#56849=CARTESIAN_POINT('Origin',(263.115917770968,-19.47200726879,445.000000551893));
#56850=CARTESIAN_POINT('',(207.560766630536,-19.47200726879,464.877951478433));
#56851=CARTESIAN_POINT('Origin',(223.744947442398,-19.47200726879,488.095739855457));
#56852=CARTESIAN_POINT('',(203.129806843349,-19.47200726879,468.704778462252));
#56853=CARTESIAN_POINT('Origin',(223.744947442398,-19.47200726879,488.095739855457));
#56854=CARTESIAN_POINT('',(203.129806843349,-19.47200726879,468.704778462252));
#56855=CARTESIAN_POINT('Origin',(205.645803107665,-19.47200726879,434.777379981771));
#56856=CARTESIAN_POINT('',(201.095181820417,-19.47200726879,462.710966424822));
#56857=CARTESIAN_POINT('',(201.095181820417,-19.47200726879,462.710966424822));
#56858=CARTESIAN_POINT('Origin',(205.645803107665,-19.47200726879,434.777379981771));
#56859=CARTESIAN_POINT('Origin',(263.115917770968,-19.47200726879,445.000000551893));
#56860=CARTESIAN_POINT('',(209.776659773475,-19.47200726879,470.227590756887));
#56861=CARTESIAN_POINT('',(209.776659773475,-19.47200726879,470.227590756887));
#56862=CARTESIAN_POINT('',(210.630641893519,-19.47200726879,471.959295189222));
#56863=CARTESIAN_POINT('Origin',(263.115917770968,-19.47200726879,445.000000551893));
#56864=CARTESIAN_POINT('',(210.630641893519,-19.47200726879,471.959295189222));
#56865=CARTESIAN_POINT('Origin',(229.706894303609,-19.47200726879,492.865992672514));
#56866=CARTESIAN_POINT('',(206.737090736042,-19.47200726879,476.331739446597));
#56867=CARTESIAN_POINT('Origin',(229.706894303609,-19.47200726879,492.865992672514));
#56868=CARTESIAN_POINT('',(206.737090736042,-19.47200726879,476.331739446597));
#56869=CARTESIAN_POINT('Origin',(204.803148167944,-19.47200726879,442.366191151322));
#56870=CARTESIAN_POINT('',(203.937522750105,-19.47200726879,470.654777158886));
#56871=CARTESIAN_POINT('',(203.937522750105,-19.47200726879,470.654777158886));
#56872=CARTESIAN_POINT('Origin',(204.803148167944,-19.47200726879,442.366191151322));
#56873=CARTESIAN_POINT('Origin',(263.115917770968,-19.47200726879,445.000000551893));
#56874=CARTESIAN_POINT('',(213.525845808207,-19.47200726879,476.973935467734));
#56875=CARTESIAN_POINT('',(213.525845808207,-19.47200726879,476.973935467734));
#56876=CARTESIAN_POINT('',(214.598554778434,-19.47200726879,478.579357894238));
#56877=CARTESIAN_POINT('Origin',(263.115917770968,-19.47200726879,445.000000551893));
#56878=CARTESIAN_POINT('',(214.598554778434,-19.47200726879,478.579357894238));
#56879=CARTESIAN_POINT('Origin',(236.240478819077,-19.47200726879,496.817245093427));
#56880=CARTESIAN_POINT('',(211.309031990467,-19.47200726879,483.422605691655));
#56881=CARTESIAN_POINT('Origin',(236.240478819077,-19.47200726879,496.817245093427));
#56882=CARTESIAN_POINT('',(211.309031990467,-19.47200726879,483.422605691655));
#56883=CARTESIAN_POINT('Origin',(204.958240883485,-19.47200726879,450.000067529947));
#56884=CARTESIAN_POINT('',(207.792422425951,-19.47200726879,478.159627552356));
#56885=CARTESIAN_POINT('',(207.792422425951,-19.47200726879,478.159627552356));
#56886=CARTESIAN_POINT('Origin',(204.958240883485,-19.47200726879,450.000067529947));
#56887=CARTESIAN_POINT('Origin',(263.115917770968,-19.47200726879,445.000000551893));
#56888=CARTESIAN_POINT('',(218.123531723188,-19.47200726879,483.173197287322));
#56889=CARTESIAN_POINT('',(218.123531723188,-19.47200726879,483.173197287322));
#56890=CARTESIAN_POINT('',(219.396613195705,-19.47200726879,484.624868485169));
#56891=CARTESIAN_POINT('Origin',(263.115917770968,-19.47200726879,445.000000551893));
#56892=CARTESIAN_POINT('',(219.396613195705,-19.47200726879,484.624868485169));
#56893=CARTESIAN_POINT('Origin',(243.233909546292,-19.47200726879,499.881890093779));
#56894=CARTESIAN_POINT('',(216.767403424178,-19.47200726879,489.856050510013));
#56895=CARTESIAN_POINT('Origin',(243.233909546292,-19.47200726879,499.881890093779));
#56896=CARTESIAN_POINT('',(216.767403424178,-19.47200726879,489.856050510013));
#56897=CARTESIAN_POINT('Origin',(206.108427574925,-19.47200726879,457.548391376297));
#56898=CARTESIAN_POINT('',(212.59392244572,-19.47200726879,485.097107534263));
#56899=CARTESIAN_POINT('',(212.59392244572,-19.47200726879,485.097107534263));
#56900=CARTESIAN_POINT('Origin',(206.108427574925,-19.47200726879,457.548391376297));
#56901=CARTESIAN_POINT('Origin',(263.115917770968,-19.47200726879,445.000000551893));
#56902=CARTESIAN_POINT('',(223.491049837692,-19.47200726879,488.719305127157));
#56903=CARTESIAN_POINT('',(223.491049837692,-19.47200726879,488.719305127157));
#56904=CARTESIAN_POINT('',(224.94272103554,-19.47200726879,489.992386599674));
#56905=CARTESIAN_POINT('Origin',(263.115917770968,-19.47200726879,445.000000551893));
#56906=CARTESIAN_POINT('',(224.94272103554,-19.47200726879,489.992386599674));
#56907=CARTESIAN_POINT('Origin',(250.567526946565,-19.47200726879,502.007490747936));
#56908=CARTESIAN_POINT('',(223.018810788598,-19.47200726879,495.521995877141));
#56909=CARTESIAN_POINT('Origin',(250.567526946565,-19.47200726879,502.007490747936));
#56910=CARTESIAN_POINT('',(223.018810788598,-19.47200726879,495.521995877141));
#56911=CARTESIAN_POINT('Origin',(208.234028229082,-19.47200726879,464.88200877657));
#56912=CARTESIAN_POINT('',(218.259867812848,-19.47200726879,491.348514898684));
#56913=CARTESIAN_POINT('',(218.259867812848,-19.47200726879,491.348514898684));
#56914=CARTESIAN_POINT('Origin',(208.234028229082,-19.47200726879,464.88200877657));
#56915=CARTESIAN_POINT('Origin',(263.115917770968,-19.47200726879,445.000000551893));
#56916=CARTESIAN_POINT('',(229.536560428624,-19.47200726879,493.517363544428));
#56917=CARTESIAN_POINT('',(229.536560428624,-19.47200726879,493.517363544428));
#56918=CARTESIAN_POINT('',(231.141982855127,-19.47200726879,494.590072514654));
#56919=CARTESIAN_POINT('Origin',(263.115917770968,-19.47200726879,445.000000551893));
#56920=CARTESIAN_POINT('',(231.141982855127,-19.47200726879,494.590072514654));
#56921=CARTESIAN_POINT('Origin',(258.115850792915,-19.47200726879,503.157677439376));
#56922=CARTESIAN_POINT('',(229.956290770506,-19.47200726879,500.323495896911));
#56923=CARTESIAN_POINT('Origin',(258.115850792915,-19.47200726879,503.157677439376));
#56924=CARTESIAN_POINT('',(229.956290770506,-19.47200726879,500.323495896911));
#56925=CARTESIAN_POINT('Origin',(211.298673229435,-19.47200726879,471.875439503784));
#56926=CARTESIAN_POINT('',(224.693312631207,-19.47200726879,496.806886332395));
#56927=CARTESIAN_POINT('',(224.693312631207,-19.47200726879,496.806886332395));
#56928=CARTESIAN_POINT('Origin',(211.298673229435,-19.47200726879,471.875439503784));
#56929=CARTESIAN_POINT('Origin',(263.115917770968,-19.47200726879,445.000000551893));
#56930=CARTESIAN_POINT('',(236.15662313364,-19.47200726879,497.485276429342));
#56931=CARTESIAN_POINT('',(236.15662313364,-19.47200726879,497.485276429342));
#56932=CARTESIAN_POINT('',(237.888327565975,-19.47200726879,498.339258549387));
#56933=CARTESIAN_POINT('Origin',(263.115917770968,-19.47200726879,445.000000551893));
#56934=CARTESIAN_POINT('',(237.888327565975,-19.47200726879,498.339258549387));
#56935=CARTESIAN_POINT('Origin',(265.74972717154,-19.4720072687901,503.312770154917));
#56936=CARTESIAN_POINT('',(237.461141163976,-19.47200726879,504.178395572756));
#56937=CARTESIAN_POINT('Origin',(265.74972717154,-19.4720072687901,503.312770154917));
#56938=CARTESIAN_POINT('',(237.461141163976,-19.47200726879,504.178395572756));
#56939=CARTESIAN_POINT('Origin',(215.249925650348,-19.47200726879,478.409024019253));
#56940=CARTESIAN_POINT('',(231.784178876265,-19.47200726879,501.378827586819));
#56941=CARTESIAN_POINT('',(231.784178876265,-19.47200726879,501.378827586819));
#56942=CARTESIAN_POINT('Origin',(215.249925650348,-19.47200726879,478.409024019253));
#56943=CARTESIAN_POINT('Origin',(263.115917770968,-19.47200726879,445.000000551893));
#56944=CARTESIAN_POINT('',(243.237966844429,-19.47200726879,500.555151692326));
#56945=CARTESIAN_POINT('',(243.237966844429,-19.47200726879,500.555151692326));
#56946=CARTESIAN_POINT('',(245.066323339639,-19.47200726879,501.175795091346));
#56947=CARTESIAN_POINT('Origin',(263.115917770968,-19.47200726879,445.000000551893));
#56948=CARTESIAN_POINT('',(245.066323339639,-19.47200726879,501.175795091346));
#56949=CARTESIAN_POINT('Origin',(273.338538341091,-19.4720072687901,502.470115215196));
#56950=CARTESIAN_POINT('',(245.40495189804,-19.47200726879,507.020736502444));
#56951=CARTESIAN_POINT('Origin',(273.338538341091,-19.4720072687901,502.470115215196));
#56952=CARTESIAN_POINT('',(245.40495189804,-19.47200726879,507.020736502444));
#56953=CARTESIAN_POINT('Origin',(220.020178467404,-19.47200726879,484.370970880464));
#56954=CARTESIAN_POINT('',(239.41113986061,-19.47200726879,504.986111479512));
#56955=CARTESIAN_POINT('',(239.41113986061,-19.47200726879,504.986111479512));
#56956=CARTESIAN_POINT('Origin',(220.020178467404,-19.47200726879,484.370970880464));
#56957=CARTESIAN_POINT('Origin',(263.115917770968,-19.47200726879,445.000000551893));
#56958=CARTESIAN_POINT('',(250.65942780678,-19.47200726879,502.674462916499));
#56959=CARTESIAN_POINT('',(250.65942780678,-19.47200726879,502.674462916499));
#56960=CARTESIAN_POINT('',(252.553152678316,-19.47200726879,503.051148213862));
#56961=CARTESIAN_POINT('Origin',(263.115917770968,-19.47200726879,445.000000551893));
#56962=CARTESIAN_POINT('',(252.553152678316,-19.47200726879,503.051148213862));
#56963=CARTESIAN_POINT('Origin',(280.752437638441,-19.4720072687901,500.64413067986));
#56964=CARTESIAN_POINT('',(253.651802168598,-19.4720072687901,508.801885444622));
#56965=CARTESIAN_POINT('Origin',(280.752437638441,-19.4720072687901,500.64413067986));
#56966=CARTESIAN_POINT('',(253.651802168598,-19.4720072687901,508.801885444622));
#56967=CARTESIAN_POINT('Origin',(225.527811332342,-19.47200726879,489.659269523657));
#56968=CARTESIAN_POINT('',(247.443696167208,-19.47200726879,507.567016382941));
#56969=CARTESIAN_POINT('',(247.443696167208,-19.47200726879,507.567016382941));
#56970=CARTESIAN_POINT('Origin',(225.527811332342,-19.47200726879,489.659269523657));
#56971=CARTESIAN_POINT('Origin',(263.115917770968,-19.47200726879,445.000000551893));
#56972=CARTESIAN_POINT('',(258.29402276601,-19.47200726879,503.806948099231));
#56973=CARTESIAN_POINT('',(258.29402276601,-19.47200726879,503.806948099231));
#56974=CARTESIAN_POINT('',(260.22071385628,-19.47200726879,503.933230105063));
#56975=CARTESIAN_POINT('Origin',(263.115917770968,-19.47200726879,445.000000551893));
#56976=CARTESIAN_POINT('',(260.22071385628,-19.47200726879,503.933230105063));
#56977=CARTESIAN_POINT('Origin',(287.864571191092,-19.4720072687901,497.866059650567));
#56978=CARTESIAN_POINT('',(262.06058608106,-19.4720072687901,509.49136644706));
#56979=CARTESIAN_POINT('Origin',(287.864571191092,-19.4720072687901,497.866059650567));
#56980=CARTESIAN_POINT('',(262.06058608106,-19.4720072687901,509.49136644706));
#56981=CARTESIAN_POINT('Origin',(231.678587119835,-19.47200726879,494.183435692855));
#56982=CARTESIAN_POINT('',(255.744408530607,-19.4720072687901,509.077382298647));
#56983=CARTESIAN_POINT('',(255.744408530607,-19.4720072687901,509.077382298647));
#56984=CARTESIAN_POINT('Origin',(231.678587119835,-19.47200726879,494.183435692855));
#56985=CARTESIAN_POINT('Origin',(263.115917770968,-19.47200726879,445.000000551893));
#56986=CARTESIAN_POINT('',(266.011121685657,-19.4720072687901,503.933230105063));
#56987=CARTESIAN_POINT('',(266.011121685657,-19.4720072687901,503.933230105063));
#56988=CARTESIAN_POINT('',(267.937812775927,-19.4720072687901,503.806948099231));
#56989=CARTESIAN_POINT('Origin',(263.115917770968,-19.47200726879,445.000000551893));
#56990=CARTESIAN_POINT('',(267.937812775927,-19.4720072687901,503.806948099231));
#56991=CARTESIAN_POINT('Origin',(294.553248422101,-19.4720072687901,494.183435692855));
#56992=CARTESIAN_POINT('',(270.48742701133,-19.4720072687901,509.077382298647));
#56993=CARTESIAN_POINT('Origin',(294.553248422101,-19.4720072687901,494.183435692855));
#56994=CARTESIAN_POINT('',(270.48742701133,-19.4720072687901,509.077382298647));
#56995=CARTESIAN_POINT('Origin',(238.367264350845,-19.47200726879,497.866059650567));
#56996=CARTESIAN_POINT('',(264.171249460877,-19.4720072687901,509.49136644706));
#56997=CARTESIAN_POINT('',(264.171249460877,-19.4720072687901,509.49136644706));
#56998=CARTESIAN_POINT('Origin',(238.367264350845,-19.47200726879,497.866059650567));
#56999=CARTESIAN_POINT('Origin',(263.115917770968,-19.47200726879,445.000000551893));
#57000=CARTESIAN_POINT('',(273.678682863621,-19.4720072687901,503.051148213862));
#57001=CARTESIAN_POINT('',(273.678682863621,-19.4720072687901,503.051148213862));
#57002=CARTESIAN_POINT('',(275.572407735157,-19.4720072687901,502.674462916499));
#57003=CARTESIAN_POINT('Origin',(263.115917770968,-19.47200726879,445.000000551893));
#57004=CARTESIAN_POINT('',(275.572407735157,-19.4720072687901,502.674462916499));
#57005=CARTESIAN_POINT('Origin',(300.704024209595,-19.47200726879,489.659269523657));
#57006=CARTESIAN_POINT('',(278.788139374729,-19.4720072687901,507.567016382941));
#57007=CARTESIAN_POINT('Origin',(300.704024209595,-19.47200726879,489.659269523657));
#57008=CARTESIAN_POINT('',(278.788139374729,-19.4720072687901,507.567016382941));
#57009=CARTESIAN_POINT('Origin',(245.479397903496,-19.47200726879,500.64413067986));
#57010=CARTESIAN_POINT('',(272.580033373339,-19.4720072687901,508.801885444621));
#57011=CARTESIAN_POINT('',(272.580033373339,-19.4720072687901,508.801885444621));
#57012=CARTESIAN_POINT('Origin',(245.479397903496,-19.47200726879,500.64413067986));
#57013=CARTESIAN_POINT('Origin',(263.115917770968,-19.47200726879,445.000000551893));
#57014=CARTESIAN_POINT('',(281.165512202298,-19.4720072687901,501.175795091345));
#57015=CARTESIAN_POINT('',(281.165512202298,-19.4720072687901,501.175795091345));
#57016=CARTESIAN_POINT('',(282.993868697508,-19.4720072687901,500.555151692326));
#57017=CARTESIAN_POINT('Origin',(263.115917770968,-19.47200726879,445.000000551893));
#57018=CARTESIAN_POINT('',(282.993868697508,-19.4720072687901,500.555151692326));
#57019=CARTESIAN_POINT('Origin',(306.211657074532,-19.47200726879,484.370970880463));
#57020=CARTESIAN_POINT('',(286.820695681327,-19.4720072687901,504.986111479512));
#57021=CARTESIAN_POINT('Origin',(306.211657074532,-19.47200726879,484.370970880463));
#57022=CARTESIAN_POINT('',(286.820695681327,-19.4720072687901,504.986111479512));
#57023=CARTESIAN_POINT('Origin',(252.893297200846,-19.47200726879,502.470115215196));
#57024=CARTESIAN_POINT('',(280.826883643897,-19.4720072687901,507.020736502444));
#57025=CARTESIAN_POINT('',(280.826883643897,-19.4720072687901,507.020736502444));
#57026=CARTESIAN_POINT('Origin',(252.893297200846,-19.47200726879,502.470115215196));
#57027=CARTESIAN_POINT('Origin',(263.115917770968,-19.47200726879,445.000000551893));
#57028=CARTESIAN_POINT('',(288.343507975962,-19.4720072687901,498.339258549386));
#57029=CARTESIAN_POINT('',(288.343507975962,-19.4720072687901,498.339258549386));
#57030=CARTESIAN_POINT('',(290.075212408297,-19.4720072687901,497.485276429342));
#57031=CARTESIAN_POINT('Origin',(263.115917770968,-19.47200726879,445.000000551893));
#57032=CARTESIAN_POINT('',(290.075212408297,-19.4720072687901,497.485276429342));
#57033=CARTESIAN_POINT('Origin',(310.981909891589,-19.47200726879,478.409024019252));
#57034=CARTESIAN_POINT('',(294.447656665672,-19.4720072687901,501.378827586819));
#57035=CARTESIAN_POINT('Origin',(310.981909891589,-19.47200726879,478.409024019252));
#57036=CARTESIAN_POINT('',(294.447656665672,-19.4720072687901,501.378827586819));
#57037=CARTESIAN_POINT('Origin',(260.482108370397,-19.47200726879,503.312770154917));
#57038=CARTESIAN_POINT('',(288.770694377961,-19.4720072687901,504.178395572756));
#57039=CARTESIAN_POINT('',(288.770694377961,-19.4720072687901,504.178395572756));
#57040=CARTESIAN_POINT('Origin',(260.482108370397,-19.47200726879,503.312770154917));
#57041=CARTESIAN_POINT('Origin',(263.115917770968,-19.47200726879,445.000000551893));
#57042=CARTESIAN_POINT('',(295.089852686809,-19.4720072687901,494.590072514654));
#57043=CARTESIAN_POINT('',(295.089852686809,-19.4720072687901,494.590072514654));
#57044=CARTESIAN_POINT('',(296.695275113313,-19.4720072687901,493.517363544428));
#57045=CARTESIAN_POINT('Origin',(263.115917770968,-19.47200726879,445.000000551893));
#57046=CARTESIAN_POINT('',(296.695275113313,-19.4720072687901,493.517363544428));
#57047=CARTESIAN_POINT('Origin',(314.933162312502,-19.47200726879,471.875439503784));
#57048=CARTESIAN_POINT('',(301.53852291073,-19.4720072687901,496.806886332394));
#57049=CARTESIAN_POINT('Origin',(314.933162312502,-19.47200726879,471.875439503784));
#57050=CARTESIAN_POINT('',(301.53852291073,-19.4720072687901,496.806886332394));
#57051=CARTESIAN_POINT('Origin',(268.115984749022,-19.4720072687901,503.157677439376));
#57052=CARTESIAN_POINT('',(296.275544771431,-19.4720072687901,500.32349589691));
#57053=CARTESIAN_POINT('',(296.275544771431,-19.4720072687901,500.32349589691));
#57054=CARTESIAN_POINT('Origin',(268.115984749022,-19.4720072687901,503.157677439376));
#57055=CARTESIAN_POINT('Origin',(263.115917770968,-19.47200726879,445.000000551893));
#57056=CARTESIAN_POINT('',(301.289114506397,-19.47200726879,489.992386599673));
#57057=CARTESIAN_POINT('',(301.289114506397,-19.47200726879,489.992386599673));
#57058=CARTESIAN_POINT('',(302.740785704245,-19.47200726879,488.719305127157));
#57059=CARTESIAN_POINT('Origin',(263.115917770968,-19.47200726879,445.000000551893));
#57060=CARTESIAN_POINT('',(302.740785704245,-19.47200726879,488.719305127157));
#57061=CARTESIAN_POINT('Origin',(317.997807312854,-19.47200726879,464.882008776569));
#57062=CARTESIAN_POINT('',(307.971967729088,-19.4720072687901,491.348514898683));
#57063=CARTESIAN_POINT('Origin',(317.997807312854,-19.47200726879,464.882008776569));
#57064=CARTESIAN_POINT('',(307.971967729088,-19.4720072687901,491.348514898683));
#57065=CARTESIAN_POINT('Origin',(275.664308595372,-19.4720072687901,502.007490747936));
#57066=CARTESIAN_POINT('',(303.213024753338,-19.4720072687901,495.521995877141));
#57067=CARTESIAN_POINT('',(303.213024753338,-19.4720072687901,495.521995877141));
#57068=CARTESIAN_POINT('Origin',(275.664308595372,-19.4720072687901,502.007490747936));
#57069=CARTESIAN_POINT('Origin',(263.115917770968,-19.47200726879,445.000000551893));
#57070=CARTESIAN_POINT('',(306.835222346232,-19.47200726879,484.624868485169));
#57071=CARTESIAN_POINT('',(306.835222346232,-19.47200726879,484.624868485169));
#57072=CARTESIAN_POINT('',(308.108303818749,-19.47200726879,483.173197287322));
#57073=CARTESIAN_POINT('Origin',(263.115917770968,-19.47200726879,445.000000551893));
#57074=CARTESIAN_POINT('',(308.108303818749,-19.47200726879,483.173197287322));
#57075=CARTESIAN_POINT('Origin',(320.123407967011,-19.47200726879,457.548391376296));
#57076=CARTESIAN_POINT('',(313.637913096216,-19.47200726879,485.097107534263));
#57077=CARTESIAN_POINT('Origin',(320.123407967011,-19.47200726879,457.548391376296));
#57078=CARTESIAN_POINT('',(313.637913096216,-19.47200726879,485.097107534263));
#57079=CARTESIAN_POINT('Origin',(282.997925995645,-19.4720072687901,499.881890093779));
#57080=CARTESIAN_POINT('',(309.464432117759,-19.4720072687901,489.856050510013));
#57081=CARTESIAN_POINT('',(309.464432117759,-19.4720072687901,489.856050510013));
#57082=CARTESIAN_POINT('Origin',(282.997925995645,-19.4720072687901,499.881890093779));
#57083=CARTESIAN_POINT('Origin',(263.115917770968,-19.47200726879,445.000000551893));
#57084=CARTESIAN_POINT('',(311.633280763503,-19.47200726879,478.579357894237));
#57085=CARTESIAN_POINT('',(311.633280763503,-19.47200726879,478.579357894237));
#57086=CARTESIAN_POINT('',(312.705989733729,-19.47200726879,476.973935467734));
#57087=CARTESIAN_POINT('Origin',(263.115917770968,-19.47200726879,445.000000551893));
#57088=CARTESIAN_POINT('',(312.705989733729,-19.47200726879,476.973935467734));
#57089=CARTESIAN_POINT('Origin',(321.273594658451,-19.47200726879,450.000067529946));
#57090=CARTESIAN_POINT('',(318.439413115986,-19.47200726879,478.159627552356));
#57091=CARTESIAN_POINT('Origin',(321.273594658451,-19.47200726879,450.000067529946));
#57092=CARTESIAN_POINT('',(318.439413115986,-19.47200726879,478.159627552356));
#57093=CARTESIAN_POINT('Origin',(289.99135672286,-19.4720072687901,496.817245093426));
#57094=CARTESIAN_POINT('',(314.92280355147,-19.47200726879,483.422605691655));
#57095=CARTESIAN_POINT('',(314.92280355147,-19.47200726879,483.422605691655));
#57096=CARTESIAN_POINT('Origin',(289.99135672286,-19.4720072687901,496.817245093426));
#57097=CARTESIAN_POINT('Origin',(263.115917770968,-19.47200726879,445.000000551893));
#57098=CARTESIAN_POINT('',(315.601193648417,-19.47200726879,471.959295189222));
#57099=CARTESIAN_POINT('',(315.601193648417,-19.47200726879,471.959295189222));
#57100=CARTESIAN_POINT('',(316.455175768462,-19.47200726879,470.227590756886));
#57101=CARTESIAN_POINT('Origin',(263.115917770968,-19.47200726879,445.000000551893));
#57102=CARTESIAN_POINT('',(316.455175768462,-19.47200726879,470.227590756886));
#57103=CARTESIAN_POINT('Origin',(321.428687373992,-19.47200726879,442.366191151322));
#57104=CARTESIAN_POINT('',(322.294312791831,-19.47200726879,470.654777158885));
#57105=CARTESIAN_POINT('Origin',(321.428687373992,-19.47200726879,442.366191151322));
#57106=CARTESIAN_POINT('',(322.294312791831,-19.47200726879,470.654777158885));
#57107=CARTESIAN_POINT('Origin',(296.524941238328,-19.4720072687901,492.865992672513));
#57108=CARTESIAN_POINT('',(319.494744805894,-19.47200726879,476.331739446597));
#57109=CARTESIAN_POINT('',(319.494744805894,-19.47200726879,476.331739446597));
#57110=CARTESIAN_POINT('Origin',(296.524941238328,-19.4720072687901,492.865992672513));
#57111=CARTESIAN_POINT('Origin',(263.115917770968,-19.47200726879,445.000000551893));
#57112=CARTESIAN_POINT('',(318.671068911401,-19.47200726879,464.877951478433));
#57113=CARTESIAN_POINT('',(318.671068911401,-19.47200726879,464.877951478433));
#57114=CARTESIAN_POINT('',(319.291712310421,-19.47200726879,463.049594983222));
#57115=CARTESIAN_POINT('Origin',(263.115917770968,-19.47200726879,445.000000551893));
#57116=CARTESIAN_POINT('',(319.291712310421,-19.47200726879,463.049594983222));
#57117=CARTESIAN_POINT('Origin',(320.586032434271,-19.47200726879,434.77737998177));
#57118=CARTESIAN_POINT('',(325.136653721519,-19.47200726879,462.710966424821));
#57119=CARTESIAN_POINT('Origin',(320.586032434271,-19.47200726879,434.77737998177));
#57120=CARTESIAN_POINT('',(325.136653721519,-19.47200726879,462.710966424821));
#57121=CARTESIAN_POINT('Origin',(302.486888099539,-19.47200726879,488.095739855457));
#57122=CARTESIAN_POINT('',(323.102028698587,-19.47200726879,468.704778462251));
#57123=CARTESIAN_POINT('',(323.102028698587,-19.47200726879,468.704778462251));
#57124=CARTESIAN_POINT('Origin',(302.486888099539,-19.47200726879,488.095739855457));
#57125=CARTESIAN_POINT('Origin',(263.115917770968,-19.47200726879,445.000000551893));
#57126=CARTESIAN_POINT('',(320.790380135574,-19.47200726879,457.456490516081));
#57127=CARTESIAN_POINT('',(320.790380135574,-19.47200726879,457.456490516081));
#57128=CARTESIAN_POINT('',(321.167065432937,-19.47200726879,455.562765644545));
#57129=CARTESIAN_POINT('Origin',(263.115917770968,-19.47200726879,445.000000551893));
#57130=CARTESIAN_POINT('',(321.167065432937,-19.47200726879,455.562765644545));
#57131=CARTESIAN_POINT('Origin',(318.760047898935,-19.47200726879,427.36348068442));
#57132=CARTESIAN_POINT('',(326.917802663697,-19.47200726879,454.464116154263));
#57133=CARTESIAN_POINT('Origin',(318.760047898935,-19.47200726879,427.36348068442));
#57134=CARTESIAN_POINT('',(326.917802663697,-19.47200726879,454.464116154263));
#57135=CARTESIAN_POINT('Origin',(307.775186742732,-19.47200726879,482.588106990519));
#57136=CARTESIAN_POINT('',(325.682933602016,-19.47200726879,460.672222155653));
#57137=CARTESIAN_POINT('',(325.682933602016,-19.47200726879,460.672222155653));
#57138=CARTESIAN_POINT('Origin',(307.775186742732,-19.47200726879,482.588106990519));
#57139=CARTESIAN_POINT('Origin',(263.115917770968,-19.47200726879,445.000000551893));
#57140=CARTESIAN_POINT('',(321.922865318307,-19.47200726879,449.821895556851));
#57141=CARTESIAN_POINT('',(321.922865318307,-19.47200726879,449.821895556851));
#57142=CARTESIAN_POINT('',(322.049147324138,-19.47200726879,447.895204466581));
#57143=CARTESIAN_POINT('Origin',(263.115917770968,-19.47200726879,445.000000551893));
#57144=CARTESIAN_POINT('',(322.049147324138,-19.47200726879,447.895204466581));
#57145=CARTESIAN_POINT('Origin',(315.981976869642,-19.47200726879,420.251347131769));
#57146=CARTESIAN_POINT('',(327.607283666135,-19.47200726879,446.055332241801));
#57147=CARTESIAN_POINT('Origin',(315.981976869642,-19.47200726879,420.251347131769));
#57148=CARTESIAN_POINT('',(327.607283666135,-19.47200726879,446.055332241801));
#57149=CARTESIAN_POINT('Origin',(312.29935291193,-19.47200726879,476.437331203026));
#57150=CARTESIAN_POINT('',(327.193299517722,-19.47200726879,452.371509792254));
#57151=CARTESIAN_POINT('',(327.193299517722,-19.47200726879,452.371509792254));
#57152=CARTESIAN_POINT('Origin',(312.29935291193,-19.47200726879,476.437331203026));
#57153=CARTESIAN_POINT('Origin',(263.115917770968,-19.47200726879,445.000000551893));
#57154=CARTESIAN_POINT('',(322.049147324138,-19.47200726879,442.104796637205));
#57155=CARTESIAN_POINT('',(322.049147324138,-19.47200726879,442.104796637205));
#57156=CARTESIAN_POINT('',(321.922865318306,-19.47200726879,440.178105546934));
#57157=CARTESIAN_POINT('Origin',(263.115917770968,-19.47200726879,445.000000551893));
#57158=CARTESIAN_POINT('',(321.922865318306,-19.47200726879,440.178105546934));
#57159=CARTESIAN_POINT('Origin',(312.29935291193,-19.47200726879,413.56266990076));
#57160=CARTESIAN_POINT('',(327.193299517722,-19.47200726879,437.628491311531));
#57161=CARTESIAN_POINT('Origin',(312.29935291193,-19.47200726879,413.56266990076));
#57162=CARTESIAN_POINT('',(327.193299517722,-19.47200726879,437.628491311531));
#57163=CARTESIAN_POINT('Origin',(315.981976869642,-19.47200726879,469.748653972016));
#57164=CARTESIAN_POINT('',(327.607283666135,-19.47200726879,443.944668861984));
#57165=CARTESIAN_POINT('',(327.607283666135,-19.47200726879,443.944668861984));
#57166=CARTESIAN_POINT('Origin',(315.981976869642,-19.47200726879,469.748653972016));
#57167=CARTESIAN_POINT('Origin',(263.115917770968,-19.47200726879,445.000000551893));
#57168=CARTESIAN_POINT('',(321.167065432937,-19.47200726879,434.43723545924));
#57169=CARTESIAN_POINT('',(321.167065432937,-19.47200726879,434.43723545924));
#57170=CARTESIAN_POINT('',(320.790380135574,-19.47200726879,432.543510587704));
#57171=CARTESIAN_POINT('Origin',(263.115917770968,-19.47200726879,445.000000551893));
#57172=CARTESIAN_POINT('',(320.790380135574,-19.47200726879,432.543510587704));
#57173=CARTESIAN_POINT('Origin',(307.775186742732,-19.47200726879,407.411894113266));
#57174=CARTESIAN_POINT('',(325.682933602016,-19.47200726879,429.327778948132));
#57175=CARTESIAN_POINT('Origin',(307.775186742732,-19.47200726879,407.411894113266));
#57176=CARTESIAN_POINT('',(325.682933602016,-19.47200726879,429.327778948132));
#57177=CARTESIAN_POINT('Origin',(318.760047898935,-19.47200726879,462.636520419365));
#57178=CARTESIAN_POINT('',(326.917802663696,-19.47200726879,435.535884949522));
#57179=CARTESIAN_POINT('',(326.917802663696,-19.47200726879,435.535884949522));
#57180=CARTESIAN_POINT('Origin',(318.760047898935,-19.47200726879,462.636520419365));
#57181=CARTESIAN_POINT('Origin',(263.115917770968,-19.47200726879,445.000000551893));
#57182=CARTESIAN_POINT('',(319.29171231042,-19.47200726879,426.950406120563));
#57183=CARTESIAN_POINT('',(319.29171231042,-19.47200726879,426.950406120563));
#57184=CARTESIAN_POINT('',(318.671068911401,-19.47200726879,425.122049625353));
#57185=CARTESIAN_POINT('Origin',(263.115917770968,-19.47200726879,445.000000551893));
#57186=CARTESIAN_POINT('',(318.671068911401,-19.47200726879,425.122049625353));
#57187=CARTESIAN_POINT('Origin',(302.486888099538,-19.47200726879,401.904261248329));
#57188=CARTESIAN_POINT('',(323.102028698587,-19.47200726879,421.295222641534));
#57189=CARTESIAN_POINT('Origin',(302.486888099538,-19.47200726879,401.904261248329));
#57190=CARTESIAN_POINT('',(323.102028698587,-19.47200726879,421.295222641534));
#57191=CARTESIAN_POINT('Origin',(320.586032434271,-19.47200726879,455.222621122015));
#57192=CARTESIAN_POINT('',(325.136653721519,-19.47200726879,427.289034678965));
#57193=CARTESIAN_POINT('',(325.136653721519,-19.47200726879,427.289034678965));
#57194=CARTESIAN_POINT('Origin',(320.586032434271,-19.47200726879,455.222621122015));
#57195=CARTESIAN_POINT('Origin',(263.115917770968,-19.47200726879,445.000000551893));
#57196=CARTESIAN_POINT('',(316.455175768461,-19.47200726879,419.772410346899));
#57197=CARTESIAN_POINT('',(316.455175768461,-19.47200726879,419.772410346899));
#57198=CARTESIAN_POINT('',(315.601193648417,-19.47200726879,418.040705914564));
#57199=CARTESIAN_POINT('Origin',(263.115917770968,-19.47200726879,445.000000551893));
#57200=CARTESIAN_POINT('',(315.601193648417,-19.47200726879,418.040705914564));
#57201=CARTESIAN_POINT('Origin',(296.524941238327,-19.4720072687899,397.134008431272));
#57202=CARTESIAN_POINT('',(319.494744805894,-19.47200726879,413.668261657189));
#57203=CARTESIAN_POINT('Origin',(296.524941238327,-19.4720072687899,397.134008431272));
#57204=CARTESIAN_POINT('',(319.494744805894,-19.47200726879,413.668261657189));
#57205=CARTESIAN_POINT('Origin',(321.428687373992,-19.47200726879,447.633809952464));
#57206=CARTESIAN_POINT('',(322.294312791831,-19.47200726879,419.345223944901));
#57207=CARTESIAN_POINT('',(322.294312791831,-19.47200726879,419.345223944901));
#57208=CARTESIAN_POINT('Origin',(321.428687373992,-19.47200726879,447.633809952464));
#57209=CARTESIAN_POINT('Origin',(263.115917770968,-19.47200726879,445.000000551893));
#57210=CARTESIAN_POINT('',(312.705989733729,-19.47200726879,413.026065636052));
#57211=CARTESIAN_POINT('',(312.705989733729,-19.47200726879,413.026065636052));
#57212=CARTESIAN_POINT('',(311.633280763503,-19.47200726879,411.420643209548));
#57213=CARTESIAN_POINT('Origin',(263.115917770968,-19.47200726879,445.000000551893));
#57214=CARTESIAN_POINT('',(311.633280763503,-19.47200726879,411.420643209548));
#57215=CARTESIAN_POINT('Origin',(289.991356722859,-19.4720072687899,393.18275601036));
#57216=CARTESIAN_POINT('',(314.92280355147,-19.47200726879,406.577395412131));
#57217=CARTESIAN_POINT('Origin',(289.991356722859,-19.4720072687899,393.18275601036));
#57218=CARTESIAN_POINT('',(314.92280355147,-19.47200726879,406.577395412131));
#57219=CARTESIAN_POINT('Origin',(321.273594658451,-19.47200726879,439.999933573839));
#57220=CARTESIAN_POINT('',(318.439413115985,-19.47200726879,411.84037355143));
#57221=CARTESIAN_POINT('',(318.439413115985,-19.47200726879,411.84037355143));
#57222=CARTESIAN_POINT('Origin',(321.273594658451,-19.47200726879,439.999933573839));
#57223=CARTESIAN_POINT('Origin',(263.115917770968,-19.47200726879,445.000000551893));
#57224=CARTESIAN_POINT('',(308.108303818748,-19.47200726879,406.826803816464));
#57225=CARTESIAN_POINT('',(308.108303818748,-19.47200726879,406.826803816464));
#57226=CARTESIAN_POINT('',(306.835222346232,-19.47200726879,405.375132618617));
#57227=CARTESIAN_POINT('Origin',(263.115917770968,-19.47200726879,445.000000551893));
#57228=CARTESIAN_POINT('',(306.835222346232,-19.47200726879,405.375132618617));
#57229=CARTESIAN_POINT('Origin',(282.997925995644,-19.4720072687899,390.118111010007));
#57230=CARTESIAN_POINT('',(309.464432117758,-19.47200726879,400.143950593773));
#57231=CARTESIAN_POINT('Origin',(282.997925995644,-19.4720072687899,390.118111010007));
#57232=CARTESIAN_POINT('',(309.464432117758,-19.47200726879,400.143950593773));
#57233=CARTESIAN_POINT('Origin',(320.123407967011,-19.47200726879,432.451609727489));
#57234=CARTESIAN_POINT('',(313.637913096216,-19.47200726879,404.902893569523));
#57235=CARTESIAN_POINT('',(313.637913096216,-19.47200726879,404.902893569523));
#57236=CARTESIAN_POINT('Origin',(320.123407967011,-19.47200726879,432.451609727489));
#57237=CARTESIAN_POINT('Origin',(263.115917770968,-19.47200726879,445.000000551893));
#57238=CARTESIAN_POINT('',(302.740785704244,-19.4720072687899,401.280695976629));
#57239=CARTESIAN_POINT('',(302.740785704244,-19.4720072687899,401.280695976629));
#57240=CARTESIAN_POINT('',(301.289114506397,-19.4720072687899,400.007614504112));
#57241=CARTESIAN_POINT('Origin',(263.115917770968,-19.47200726879,445.000000551893));
#57242=CARTESIAN_POINT('',(301.289114506397,-19.4720072687899,400.007614504112));
#57243=CARTESIAN_POINT('Origin',(275.664308595371,-19.4720072687899,387.99251035585));
#57244=CARTESIAN_POINT('',(303.213024753338,-19.4720072687899,394.478005226645));
#57245=CARTESIAN_POINT('Origin',(275.664308595371,-19.4720072687899,387.99251035585));
#57246=CARTESIAN_POINT('',(303.213024753338,-19.4720072687899,394.478005226645));
#57247=CARTESIAN_POINT('Origin',(317.997807312854,-19.47200726879,425.117992327216));
#57248=CARTESIAN_POINT('',(307.971967729088,-19.4720072687899,398.651486205102));
#57249=CARTESIAN_POINT('',(307.971967729088,-19.4720072687899,398.651486205102));
#57250=CARTESIAN_POINT('Origin',(317.997807312854,-19.47200726879,425.117992327216));
#57251=CARTESIAN_POINT('Origin',(263.115917770968,-19.47200726879,445.000000551893));
#57252=CARTESIAN_POINT('',(296.695275113313,-19.4720072687899,396.482637559358));
#57253=CARTESIAN_POINT('',(296.695275113313,-19.4720072687899,396.482637559358));
#57254=CARTESIAN_POINT('',(295.089852686809,-19.4720072687899,395.409928589132));
#57255=CARTESIAN_POINT('Origin',(263.115917770968,-19.47200726879,445.000000551893));
#57256=CARTESIAN_POINT('',(295.089852686809,-19.4720072687899,395.409928589132));
#57257=CARTESIAN_POINT('Origin',(268.115984749021,-19.4720072687899,386.84232366441));
#57258=CARTESIAN_POINT('',(296.275544771431,-19.4720072687899,389.676505206875));
#57259=CARTESIAN_POINT('Origin',(268.115984749021,-19.4720072687899,386.84232366441));
#57260=CARTESIAN_POINT('',(296.275544771431,-19.4720072687899,389.676505206875));
#57261=CARTESIAN_POINT('Origin',(314.933162312501,-19.47200726879,418.124561600002));
#57262=CARTESIAN_POINT('',(301.53852291073,-19.4720072687899,393.193114771391));
#57263=CARTESIAN_POINT('',(301.53852291073,-19.4720072687899,393.193114771391));
#57264=CARTESIAN_POINT('Origin',(314.933162312501,-19.47200726879,418.124561600002));
#57265=CARTESIAN_POINT('Origin',(263.115917770968,-19.47200726879,445.000000551893));
#57266=CARTESIAN_POINT('',(290.075212408297,-19.4720072687899,392.514724674444));
#57267=CARTESIAN_POINT('',(290.075212408297,-19.4720072687899,392.514724674444));
#57268=CARTESIAN_POINT('',(288.343507975962,-19.4720072687899,391.6607425544));
#57269=CARTESIAN_POINT('Origin',(263.115917770968,-19.47200726879,445.000000551893));
#57270=CARTESIAN_POINT('',(288.343507975962,-19.4720072687899,391.6607425544));
#57271=CARTESIAN_POINT('Origin',(260.482108370397,-19.4720072687899,386.687230948869));
#57272=CARTESIAN_POINT('',(288.77069437796,-19.4720072687899,385.82160553103));
#57273=CARTESIAN_POINT('Origin',(260.482108370397,-19.4720072687899,386.687230948869));
#57274=CARTESIAN_POINT('',(288.77069437796,-19.4720072687899,385.82160553103));
#57275=CARTESIAN_POINT('Origin',(310.981909891589,-19.47200726879,411.590977084533));
#57276=CARTESIAN_POINT('',(294.447656665672,-19.4720072687899,388.621173516967));
#57277=CARTESIAN_POINT('',(294.447656665672,-19.4720072687899,388.621173516967));
#57278=CARTESIAN_POINT('Origin',(310.981909891589,-19.47200726879,411.590977084533));
#57279=CARTESIAN_POINT('Origin',(263.115917770968,-19.47200726879,445.000000551893));
#57280=CARTESIAN_POINT('',(282.993868697508,-19.4720072687899,389.44484941146));
#57281=CARTESIAN_POINT('',(282.993868697508,-19.4720072687899,389.44484941146));
#57282=CARTESIAN_POINT('',(281.165512202297,-19.4720072687899,388.82420601244));
#57283=CARTESIAN_POINT('Origin',(263.115917770968,-19.47200726879,445.000000551893));
#57284=CARTESIAN_POINT('',(281.165512202297,-19.4720072687899,388.82420601244));
#57285=CARTESIAN_POINT('Origin',(252.893297200845,-19.4720072687899,387.52988588859));
#57286=CARTESIAN_POINT('',(280.826883643896,-19.4720072687899,382.979264601342));
#57287=CARTESIAN_POINT('Origin',(252.893297200845,-19.4720072687899,387.52988588859));
#57288=CARTESIAN_POINT('',(280.826883643896,-19.4720072687899,382.979264601342));
#57289=CARTESIAN_POINT('Origin',(306.211657074532,-19.47200726879,405.629030223323));
#57290=CARTESIAN_POINT('',(286.820695681326,-19.4720072687899,385.013889624274));
#57291=CARTESIAN_POINT('',(286.820695681326,-19.4720072687899,385.013889624274));
#57292=CARTESIAN_POINT('Origin',(306.211657074532,-19.47200726879,405.629030223323));
#57293=CARTESIAN_POINT('Origin',(263.115917770968,-19.47200726879,445.000000551893));
#57294=CARTESIAN_POINT('',(275.572407735156,-19.4720072687899,387.325538187287));
#57295=CARTESIAN_POINT('',(275.572407735156,-19.4720072687899,387.325538187287));
#57296=CARTESIAN_POINT('',(273.67868286362,-19.4720072687899,386.948852889924));
#57297=CARTESIAN_POINT('Origin',(263.115917770968,-19.47200726879,445.000000551893));
#57298=CARTESIAN_POINT('',(273.67868286362,-19.4720072687899,386.948852889924));
#57299=CARTESIAN_POINT('Origin',(245.479397903495,-19.4720072687899,389.355870423926));
#57300=CARTESIAN_POINT('',(272.580033373339,-19.4720072687899,381.198115659165));
#57301=CARTESIAN_POINT('Origin',(245.479397903495,-19.4720072687899,389.355870423926));
#57302=CARTESIAN_POINT('',(272.580033373339,-19.4720072687899,381.198115659165));
#57303=CARTESIAN_POINT('Origin',(300.704024209595,-19.4720072687899,400.340731580129));
#57304=CARTESIAN_POINT('',(278.788139374728,-19.4720072687899,382.432984720845));
#57305=CARTESIAN_POINT('',(278.788139374728,-19.4720072687899,382.432984720845));
#57306=CARTESIAN_POINT('Origin',(300.704024209595,-19.4720072687899,400.340731580129));
#57307=CARTESIAN_POINT('Origin',(263.115917770968,-19.47200726879,445.000000551893));
#57308=CARTESIAN_POINT('',(267.937812775926,-19.4720072687899,386.193053004555));
#57309=CARTESIAN_POINT('',(267.937812775926,-19.4720072687899,386.193053004555));
#57310=CARTESIAN_POINT('',(266.011121685656,-19.4720072687899,386.066770998723));
#57311=CARTESIAN_POINT('Origin',(263.115917770968,-19.47200726879,445.000000551893));
#57312=CARTESIAN_POINT('',(266.011121685656,-19.4720072687899,386.066770998723));
#57313=CARTESIAN_POINT('Origin',(238.367264350844,-19.4720072687899,392.133941453219));
#57314=CARTESIAN_POINT('',(264.171249460876,-19.4720072687899,380.508634656726));
#57315=CARTESIAN_POINT('Origin',(238.367264350844,-19.4720072687899,392.133941453219));
#57316=CARTESIAN_POINT('',(264.171249460876,-19.4720072687899,380.508634656726));
#57317=CARTESIAN_POINT('Origin',(294.553248422101,-19.4720072687899,395.816565410931));
#57318=CARTESIAN_POINT('',(270.487427011329,-19.4720072687899,380.922618805139));
#57319=CARTESIAN_POINT('',(270.487427011329,-19.4720072687899,380.922618805139));
#57320=CARTESIAN_POINT('Origin',(294.553248422101,-19.4720072687899,395.816565410931));
#57321=CARTESIAN_POINT('Origin',(263.115917770968,-19.47200726879,445.000000551893));
#57322=CARTESIAN_POINT('',(260.22071385628,-19.4720072687899,386.066770998723));
#57323=CARTESIAN_POINT('',(260.22071385628,-19.4720072687899,386.066770998723));
#57324=CARTESIAN_POINT('',(258.294022766009,-19.4720072687899,386.193053004555));
#57325=CARTESIAN_POINT('Origin',(263.115917770968,-19.47200726879,445.000000551893));
#57326=CARTESIAN_POINT('',(258.294022766009,-19.4720072687899,386.193053004555));
#57327=CARTESIAN_POINT('Origin',(231.678587119835,-19.4720072687899,395.816565410931));
#57328=CARTESIAN_POINT('',(255.744408530606,-19.4720072687899,380.922618805139));
#57329=CARTESIAN_POINT('Origin',(231.678587119835,-19.4720072687899,395.816565410931));
#57330=CARTESIAN_POINT('',(255.744408530606,-19.4720072687899,380.922618805139));
#57331=CARTESIAN_POINT('Origin',(287.864571191091,-19.4720072687899,392.133941453219));
#57332=CARTESIAN_POINT('',(262.060586081059,-19.4720072687899,380.508634656726));
#57333=CARTESIAN_POINT('',(262.060586081059,-19.4720072687899,380.508634656726));
#57334=CARTESIAN_POINT('Origin',(287.864571191091,-19.4720072687899,392.133941453219));
#57335=CARTESIAN_POINT('Origin',(263.115917770968,-19.47200726879,445.000000551893));
#57336=CARTESIAN_POINT('',(252.553152678315,-19.4720072687899,386.948852889924));
#57337=CARTESIAN_POINT('',(252.553152678315,-19.4720072687899,386.948852889924));
#57338=CARTESIAN_POINT('',(250.659427806779,-19.4720072687899,387.325538187287));
#57339=CARTESIAN_POINT('Origin',(263.115917770968,-19.47200726879,445.000000551893));
#57340=CARTESIAN_POINT('',(250.659427806779,-19.4720072687899,387.325538187287));
#57341=CARTESIAN_POINT('Origin',(225.527811332341,-19.4720072687899,400.340731580129));
#57342=CARTESIAN_POINT('',(247.443696167207,-19.4720072687899,382.432984720845));
#57343=CARTESIAN_POINT('Origin',(225.527811332341,-19.4720072687899,400.340731580129));
#57344=CARTESIAN_POINT('',(247.443696167207,-19.4720072687899,382.432984720845));
#57345=CARTESIAN_POINT('Origin',(280.75243763844,-19.4720072687899,389.355870423926));
#57346=CARTESIAN_POINT('',(253.651802168597,-19.4720072687899,381.198115659165));
#57347=CARTESIAN_POINT('',(253.651802168597,-19.4720072687899,381.198115659165));
#57348=CARTESIAN_POINT('Origin',(280.75243763844,-19.4720072687899,389.355870423926));
#57349=CARTESIAN_POINT('Origin',(263.115917770968,-19.47200726879,445.000000551893));
#57350=CARTESIAN_POINT('',(245.066323339638,-19.4720072687899,388.824206012441));
#57351=CARTESIAN_POINT('',(245.066323339638,-19.4720072687899,388.824206012441));
#57352=CARTESIAN_POINT('',(243.237966844428,-19.4720072687899,389.44484941146));
#57353=CARTESIAN_POINT('Origin',(263.115917770968,-19.47200726879,445.000000551893));
#57354=CARTESIAN_POINT('',(243.237966844428,-19.4720072687899,389.44484941146));
#57355=CARTESIAN_POINT('Origin',(220.020178467404,-19.4720072687899,405.629030223323));
#57356=CARTESIAN_POINT('',(239.411139860609,-19.4720072687899,385.013889624274));
#57357=CARTESIAN_POINT('Origin',(220.020178467404,-19.4720072687899,405.629030223323));
#57358=CARTESIAN_POINT('',(239.411139860609,-19.4720072687899,385.013889624274));
#57359=CARTESIAN_POINT('Origin',(273.33853834109,-19.4720072687899,387.52988588859));
#57360=CARTESIAN_POINT('',(245.40495189804,-19.4720072687899,382.979264601342));
#57361=CARTESIAN_POINT('',(245.40495189804,-19.4720072687899,382.979264601342));
#57362=CARTESIAN_POINT('Origin',(273.33853834109,-19.4720072687899,387.52988588859));
#57363=CARTESIAN_POINT('Origin',(263.115917770968,-19.47200726879,445.000000551893));
#57364=CARTESIAN_POINT('',(237.888327565974,-19.4720072687899,391.6607425544));
#57365=CARTESIAN_POINT('',(237.888327565974,-19.4720072687899,391.6607425544));
#57366=CARTESIAN_POINT('',(236.156623133639,-19.4720072687899,392.514724674444));
#57367=CARTESIAN_POINT('Origin',(263.115917770968,-19.47200726879,445.000000551893));
#57368=CARTESIAN_POINT('',(236.156623133639,-19.4720072687899,392.514724674444));
#57369=CARTESIAN_POINT('Origin',(215.249925650347,-19.4720072687899,411.590977084534));
#57370=CARTESIAN_POINT('',(231.784178876264,-19.4720072687899,388.621173516967));
#57371=CARTESIAN_POINT('Origin',(215.249925650347,-19.4720072687899,411.590977084534));
#57372=CARTESIAN_POINT('',(231.784178876264,-19.4720072687899,388.621173516967));
#57373=CARTESIAN_POINT('Origin',(265.749727171539,-19.4720072687899,386.687230948869));
#57374=CARTESIAN_POINT('',(237.461141163976,-19.4720072687899,385.82160553103));
#57375=CARTESIAN_POINT('',(237.461141163976,-19.4720072687899,385.82160553103));
#57376=CARTESIAN_POINT('Origin',(265.749727171539,-19.4720072687899,386.687230948869));
#57377=CARTESIAN_POINT('Origin',(263.115917770968,-19.47200726879,445.000000551893));
#57378=CARTESIAN_POINT('',(231.141982855127,-19.4720072687899,395.409928589132));
#57379=CARTESIAN_POINT('',(231.141982855127,-19.4720072687899,395.409928589132));
#57380=CARTESIAN_POINT('',(229.536560428623,-19.4720072687899,396.482637559359));
#57381=CARTESIAN_POINT('Origin',(263.115917770968,-19.47200726879,445.000000551893));
#57382=CARTESIAN_POINT('',(229.536560428623,-19.4720072687899,396.482637559359));
#57383=CARTESIAN_POINT('Origin',(211.298673229435,-19.4720072687899,418.124561600002));
#57384=CARTESIAN_POINT('',(224.693312631206,-19.4720072687899,393.193114771392));
#57385=CARTESIAN_POINT('Origin',(211.298673229435,-19.4720072687899,418.124561600002));
#57386=CARTESIAN_POINT('',(224.693312631206,-19.4720072687899,393.193114771392));
#57387=CARTESIAN_POINT('Origin',(258.115850792914,-19.4720072687899,386.84232366441));
#57388=CARTESIAN_POINT('',(229.956290770505,-19.4720072687899,389.676505206876));
#57389=CARTESIAN_POINT('',(229.956290770505,-19.4720072687899,389.676505206876));
#57390=CARTESIAN_POINT('Origin',(258.115850792914,-19.4720072687899,386.84232366441));
#57391=CARTESIAN_POINT('Origin',(263.115917770968,-19.47200726879,445.000000551893));
#57392=CARTESIAN_POINT('',(224.942721035539,-19.4720072687899,400.007614504113));
#57393=CARTESIAN_POINT('',(224.942721035539,-19.4720072687899,400.007614504113));
#57394=CARTESIAN_POINT('',(223.491049837692,-19.4720072687899,401.280695976629));
#57395=CARTESIAN_POINT('Origin',(263.115917770968,-19.47200726879,445.000000551893));
#57396=CARTESIAN_POINT('',(223.491049837692,-19.4720072687899,401.280695976629));
#57397=CARTESIAN_POINT('Origin',(208.234028229082,-19.4720072687899,425.117992327217));
#57398=CARTESIAN_POINT('',(218.259867812848,-19.4720072687899,398.651486205103));
#57399=CARTESIAN_POINT('Origin',(208.234028229082,-19.4720072687899,425.117992327217));
#57400=CARTESIAN_POINT('',(218.259867812848,-19.4720072687899,398.651486205103));
#57401=CARTESIAN_POINT('Origin',(250.567526946564,-19.4720072687899,387.99251035585));
#57402=CARTESIAN_POINT('',(223.018810788598,-19.4720072687899,394.478005226645));
#57403=CARTESIAN_POINT('',(223.018810788598,-19.4720072687899,394.478005226645));
#57404=CARTESIAN_POINT('Origin',(250.567526946564,-19.4720072687899,387.99251035585));
#57405=CARTESIAN_POINT('Origin',(263.115917770968,-19.47200726879,445.000000551893));
#57406=CARTESIAN_POINT('',(219.396613195704,-19.4720072687899,405.375132618617));
#57407=CARTESIAN_POINT('',(219.396613195704,-19.4720072687899,405.375132618617));
#57408=CARTESIAN_POINT('',(218.123531723188,-19.4720072687899,406.826803816464));
#57409=CARTESIAN_POINT('Origin',(263.115917770968,-19.47200726879,445.000000551893));
#57410=CARTESIAN_POINT('',(218.123531723188,-19.4720072687899,406.826803816464));
#57411=CARTESIAN_POINT('Origin',(206.108427574925,-19.4720072687899,432.45160972749));
#57412=CARTESIAN_POINT('',(212.59392244572,-19.4720072687899,404.902893569523));
#57413=CARTESIAN_POINT('Origin',(206.108427574925,-19.4720072687899,432.45160972749));
#57414=CARTESIAN_POINT('',(212.59392244572,-19.4720072687899,404.902893569523));
#57415=CARTESIAN_POINT('Origin',(243.233909546291,-19.4720072687899,390.118111010007));
#57416=CARTESIAN_POINT('',(216.767403424177,-19.4720072687899,400.143950593773));
#57417=CARTESIAN_POINT('',(216.767403424177,-19.4720072687899,400.143950593773));
#57418=CARTESIAN_POINT('Origin',(243.233909546291,-19.4720072687899,390.118111010007));
#57419=CARTESIAN_POINT('Origin',(263.115917770968,-19.47200726879,445.000000551893));
#57420=CARTESIAN_POINT('',(214.598554778433,-19.4720072687899,411.420643209549));
#57421=CARTESIAN_POINT('',(214.598554778433,-19.4720072687899,411.420643209549));
#57422=CARTESIAN_POINT('',(213.525845808207,-19.4720072687899,413.026065636052));
#57423=CARTESIAN_POINT('Origin',(263.115917770968,-19.47200726879,445.000000551893));
#57424=CARTESIAN_POINT('',(213.525845808207,-19.4720072687899,413.026065636052));
#57425=CARTESIAN_POINT('Origin',(204.958240883485,-19.47200726879,439.99993357384));
#57426=CARTESIAN_POINT('',(207.79242242595,-19.4720072687899,411.840373551431));
#57427=CARTESIAN_POINT('Origin',(204.958240883485,-19.47200726879,439.99993357384));
#57428=CARTESIAN_POINT('',(207.79242242595,-19.4720072687899,411.840373551431));
#57429=CARTESIAN_POINT('Origin',(236.240478819077,-19.4720072687899,393.18275601036));
#57430=CARTESIAN_POINT('',(211.309031990466,-19.4720072687899,406.577395412131));
#57431=CARTESIAN_POINT('',(211.309031990466,-19.4720072687899,406.577395412131));
#57432=CARTESIAN_POINT('Origin',(236.240478819077,-19.4720072687899,393.18275601036));
#57433=CARTESIAN_POINT('Origin',(263.115917770968,-19.47200726879,445.000000551893));
#57434=CARTESIAN_POINT('',(210.630641893519,-19.4720072687899,418.040705914564));
#57435=CARTESIAN_POINT('',(210.630641893519,-19.4720072687899,418.040705914564));
#57436=CARTESIAN_POINT('',(209.776659773475,-19.4720072687899,419.7724103469));
#57437=CARTESIAN_POINT('Origin',(263.115917770968,-19.47200726879,445.000000551893));
#57438=CARTESIAN_POINT('',(209.776659773475,-19.4720072687899,419.7724103469));
#57439=CARTESIAN_POINT('Origin',(204.803148167944,-19.47200726879,447.633809952465));
#57440=CARTESIAN_POINT('',(203.937522750105,-19.4720072687899,419.345223944901));
#57441=CARTESIAN_POINT('Origin',(204.803148167944,-19.47200726879,447.633809952465));
#57442=CARTESIAN_POINT('',(203.937522750105,-19.4720072687899,419.345223944901));
#57443=CARTESIAN_POINT('Origin',(229.706894303608,-19.4720072687899,397.134008431273));
#57444=CARTESIAN_POINT('',(206.737090736042,-19.4720072687899,413.668261657189));
#57445=CARTESIAN_POINT('',(206.737090736042,-19.4720072687899,413.668261657189));
#57446=CARTESIAN_POINT('Origin',(229.706894303608,-19.4720072687899,397.134008431273));
#57447=CARTESIAN_POINT('Origin',(263.115917770968,-19.47200726879,445.000000551893));
#57448=CARTESIAN_POINT('',(207.560766630535,-19.4720072687899,425.122049625353));
#57449=CARTESIAN_POINT('',(207.560766630535,-19.4720072687899,425.122049625353));
#57450=CARTESIAN_POINT('',(206.940123231516,-19.4720072687899,426.950406120564));
#57451=CARTESIAN_POINT('Origin',(263.115917770968,-19.47200726879,445.000000551893));
#57452=CARTESIAN_POINT('',(206.940123231516,-19.4720072687899,426.950406120564));
#57453=CARTESIAN_POINT('Origin',(205.645803107665,-19.47200726879,455.222621122016));
#57454=CARTESIAN_POINT('',(201.095181820417,-19.4720072687899,427.289034678965));
#57455=CARTESIAN_POINT('Origin',(205.645803107665,-19.47200726879,455.222621122016));
#57456=CARTESIAN_POINT('',(201.095181820417,-19.4720072687899,427.289034678965));
#57457=CARTESIAN_POINT('Origin',(223.744947442398,-19.4720072687899,401.904261248329));
#57458=CARTESIAN_POINT('',(203.129806843349,-19.4720072687899,421.295222641535));
#57459=CARTESIAN_POINT('',(203.129806843349,-19.4720072687899,421.295222641535));
#57460=CARTESIAN_POINT('Origin',(223.744947442398,-19.4720072687899,401.904261248329));
#57461=CARTESIAN_POINT('Origin',(263.115917770968,-19.47200726879,445.000000551893));
#57462=CARTESIAN_POINT('',(205.441455406362,-19.4720072687899,432.543510587705));
#57463=CARTESIAN_POINT('',(205.441455406362,-19.4720072687899,432.543510587705));
#57464=CARTESIAN_POINT('',(205.064770108999,-19.47200726879,434.437235459241));
#57465=CARTESIAN_POINT('Origin',(263.115917770968,-19.47200726879,445.000000551893));
#57466=CARTESIAN_POINT('',(205.064770108999,-19.47200726879,434.437235459241));
#57467=CARTESIAN_POINT('Origin',(207.471787643001,-19.47200726879,462.636520419366));
#57468=CARTESIAN_POINT('',(199.31403287824,-19.47200726879,435.535884949523));
#57469=CARTESIAN_POINT('Origin',(207.471787643001,-19.47200726879,462.636520419366));
#57470=CARTESIAN_POINT('',(199.31403287824,-19.47200726879,435.535884949522));
#57471=CARTESIAN_POINT('Origin',(218.456648799204,-19.4720072687899,407.411894113266));
#57472=CARTESIAN_POINT('',(200.54890193992,-19.4720072687899,429.327778948133));
#57473=CARTESIAN_POINT('',(200.54890193992,-19.4720072687899,429.327778948133));
#57474=CARTESIAN_POINT('Origin',(218.456648799204,-19.4720072687899,407.411894113266));
#57475=CARTESIAN_POINT('Origin',(263.115917770968,-19.47200726879,445.000000551893));
#57476=CARTESIAN_POINT('',(204.30897022363,-19.47200726879,440.178105546935));
#57477=CARTESIAN_POINT('',(204.30897022363,-19.47200726879,440.178105546935));
#57478=CARTESIAN_POINT('',(204.182688217798,-19.47200726879,442.104796637205));
#57479=CARTESIAN_POINT('Origin',(263.115917770968,-19.47200726879,445.000000551893));
#57480=CARTESIAN_POINT('',(204.182688217798,-19.47200726879,442.104796637205));
#57481=CARTESIAN_POINT('Origin',(210.249858672294,-19.47200726879,469.748653972017));
#57482=CARTESIAN_POINT('',(198.624551875801,-19.47200726879,443.944668861985));
#57483=CARTESIAN_POINT('Origin',(210.249858672294,-19.47200726879,469.748653972017));
#57484=CARTESIAN_POINT('',(198.624551875801,-19.47200726879,443.944668861985));
#57485=CARTESIAN_POINT('Origin',(213.932482630006,-19.4720072687899,413.56266990076));
#57486=CARTESIAN_POINT('',(199.038536024214,-19.47200726879,437.628491311532));
#57487=CARTESIAN_POINT('',(199.038536024214,-19.47200726879,437.628491311532));
#57488=CARTESIAN_POINT('Origin',(213.932482630006,-19.4720072687899,413.56266990076));
#57489=CARTESIAN_POINT('Origin',(263.115917770968,-19.47200726879,445.000000551893));
#57490=CARTESIAN_POINT('',(198.624551875801,-19.47200726879,446.055332241802));
#57491=CARTESIAN_POINT('Origin',(263.115917770968,-19.47200726879,445.000000551893));
#57492=CARTESIAN_POINT('',(198.624551875801,-19.47200726879,446.055332241802));
#57493=CARTESIAN_POINT('Origin',(263.115917770968,-19.47200726879,445.000000551893));
#57494=CARTESIAN_POINT('Origin',(263.115917770968,-19.47200726879,445.000000551893));
#57495=CARTESIAN_POINT('Origin',(263.115917770968,-19.47200726879,445.000000551893));
#57496=CARTESIAN_POINT('Origin',(263.115917770968,-19.47200726879,445.000000551893));
#57497=CARTESIAN_POINT('Origin',(263.115917770968,-19.47200726879,445.000000551893));
#57498=CARTESIAN_POINT('Origin',(263.115917770968,-19.47200726879,445.000000551893));
#57499=CARTESIAN_POINT('Origin',(263.115917770968,-19.47200726879,445.000000551893));
#57500=CARTESIAN_POINT('Origin',(263.115917770968,-19.47200726879,445.000000551893));
#57501=CARTESIAN_POINT('Origin',(263.115917770968,-19.47200726879,445.000000551893));
#57502=CARTESIAN_POINT('Origin',(263.115917770968,-19.47200726879,445.000000551893));
#57503=CARTESIAN_POINT('Origin',(263.115917770968,-19.47200726879,445.000000551893));
#57504=CARTESIAN_POINT('Origin',(263.115917770968,-19.47200726879,445.000000551893));
#57505=CARTESIAN_POINT('Origin',(263.115917770968,-19.47200726879,445.000000551893));
#57506=CARTESIAN_POINT('Origin',(263.115917770968,-19.47200726879,445.000000551893));
#57507=CARTESIAN_POINT('Origin',(263.115917770968,-19.47200726879,445.000000551893));
#57508=CARTESIAN_POINT('Origin',(263.115917770968,-19.47200726879,445.000000551893));
#57509=CARTESIAN_POINT('Origin',(263.115917770968,-19.47200726879,445.000000551893));
#57510=CARTESIAN_POINT('Origin',(263.115917770968,-19.47200726879,445.000000551893));
#57511=CARTESIAN_POINT('Origin',(263.115917770968,-19.47200726879,445.000000551893));
#57512=CARTESIAN_POINT('Origin',(263.115917770968,-19.47200726879,445.000000551893));
#57513=CARTESIAN_POINT('Origin',(263.115917770968,-19.47200726879,445.000000551893));
#57514=CARTESIAN_POINT('Origin',(263.115917770968,-19.47200726879,445.000000551893));
#57515=CARTESIAN_POINT('Origin',(263.115917770968,-19.47200726879,445.000000551893));
#57516=CARTESIAN_POINT('Origin',(263.115917770968,-19.47200726879,445.000000551893));
#57517=CARTESIAN_POINT('Origin',(263.115917770968,-19.47200726879,445.000000551893));
#57518=CARTESIAN_POINT('Origin',(263.115917770968,-19.47200726879,445.000000551893));
#57519=CARTESIAN_POINT('Origin',(263.115917770968,-19.47200726879,445.000000551893));
#57520=CARTESIAN_POINT('Origin',(263.115917770968,-19.47200726879,445.000000551893));
#57521=CARTESIAN_POINT('Origin',(263.115917770968,-19.47200726879,445.000000551893));
#57522=CARTESIAN_POINT('Origin',(263.115917770968,-19.47200726879,445.000000551893));
#57523=CARTESIAN_POINT('Origin',(263.115917770968,-19.47200726879,445.000000551893));
#57524=CARTESIAN_POINT('Origin',(263.115917770968,-19.47200726879,445.000000551893));
#57525=CARTESIAN_POINT('Origin',(263.115917770968,-19.47200726879,445.000000551893));
#57526=CARTESIAN_POINT('Origin',(263.115917770968,-19.47200726879,445.000000551893));
#57527=CARTESIAN_POINT('Origin',(263.115917770968,-19.47200726879,445.000000551893));
#57528=CARTESIAN_POINT('Origin',(263.115917770968,-19.47200726879,445.000000551893));
#57529=CARTESIAN_POINT('Origin',(263.115917770968,-19.47200726879,445.000000551893));
#57530=CARTESIAN_POINT('Origin',(263.115917770968,-19.47200726879,445.000000551893));
#57531=CARTESIAN_POINT('Origin',(263.115917770968,-19.47200726879,445.000000551893));
#57532=CARTESIAN_POINT('Origin',(263.115917770968,-19.47200726879,445.000000551893));
#57533=CARTESIAN_POINT('Origin',(263.115917770968,-19.47200726879,445.000000551893));
#57534=CARTESIAN_POINT('Origin',(263.115917770968,-19.47200726879,445.000000551893));
#57535=CARTESIAN_POINT('Origin',(263.115917770968,-19.47200726879,445.000000551893));
#57536=CARTESIAN_POINT('Origin',(263.115917770968,-19.47200726879,445.000000551893));
#57537=CARTESIAN_POINT('Origin',(263.115917770968,-19.47200726879,445.000000551893));
#57538=CARTESIAN_POINT('Origin',(263.115917770968,-19.47200726879,445.000000551893));
#57539=CARTESIAN_POINT('Origin',(263.115917770968,-19.47200726879,445.000000551893));
#57540=CARTESIAN_POINT('Origin',(263.115917770968,-19.47200726879,445.000000551893));
#57541=CARTESIAN_POINT('Origin',(263.115917770968,-19.47200726879,445.000000551893));
#57542=CARTESIAN_POINT('Origin',(263.115917770968,-19.47200726879,445.000000551893));
#57543=CARTESIAN_POINT('Origin',(263.115917770968,-19.47200726879,445.000000551893));
#57544=CARTESIAN_POINT('Origin',(263.115917770968,-19.47200726879,445.000000551893));
#57545=CARTESIAN_POINT('Origin',(263.115917770968,-19.47200726879,445.000000551893));
#57546=CARTESIAN_POINT('Origin',(263.115917770968,-19.47200726879,445.000000551893));
#57547=CARTESIAN_POINT('Origin',(263.115917770968,-19.47200726879,445.000000551893));
#57548=CARTESIAN_POINT('Origin',(263.115917770968,-19.47200726879,445.000000551893));
#57549=CARTESIAN_POINT('Origin',(263.115917770968,-19.47200726879,445.000000551893));
#57550=CARTESIAN_POINT('Origin',(263.115917770968,-19.47200726879,445.000000551893));
#57551=CARTESIAN_POINT('Origin',(263.115917770968,-19.47200726879,445.000000551893));
#57552=CARTESIAN_POINT('Origin',(263.115917770968,-19.47200726879,445.000000551893));
#57553=CARTESIAN_POINT('Origin',(263.115917770968,-19.47200726879,445.000000551893));
#57554=CARTESIAN_POINT('Origin',(263.115917770968,-19.47200726879,445.000000551893));
#57555=CARTESIAN_POINT('Origin',(263.115917770968,-19.47200726879,445.000000551893));
#57556=CARTESIAN_POINT('Origin',(263.115917770968,-19.47200726879,445.000000551893));
#57557=CARTESIAN_POINT('Origin',(263.115917770968,-19.47200726879,445.000000551893));
#57558=CARTESIAN_POINT('Origin',(263.115917770968,-19.47200726879,445.000000551893));
#57559=CARTESIAN_POINT('Origin',(263.115917770968,-19.47200726879,445.000000551893));
#57560=CARTESIAN_POINT('Origin',(263.115917770968,-19.47200726879,445.000000551893));
#57561=CARTESIAN_POINT('Origin',(263.115917770968,-19.47200726879,445.000000551893));
#57562=CARTESIAN_POINT('Origin',(263.115917770968,-19.47200726879,445.000000551893));
#57563=CARTESIAN_POINT('Origin',(263.115917770968,-19.47200726879,445.000000551893));
#57564=CARTESIAN_POINT('Origin',(263.115917770968,-19.47200726879,445.000000551893));
#57565=CARTESIAN_POINT('Origin',(263.115917770968,-19.47200726879,445.000000551893));
#57566=CARTESIAN_POINT('Origin',(263.115917770968,-19.47200726879,445.000000551893));
#57567=CARTESIAN_POINT('Origin',(263.115917770968,-19.47200726879,445.000000551893));
#57568=CARTESIAN_POINT('Origin',(263.115917770968,-19.47200726879,445.000000551893));
#57569=CARTESIAN_POINT('Origin',(263.115917770968,-19.47200726879,445.000000551893));
#57570=CARTESIAN_POINT('Origin',(263.115917770968,-19.47200726879,445.000000551893));
#57571=CARTESIAN_POINT('Origin',(263.115917770968,-19.47200726879,445.000000551893));
#57572=CARTESIAN_POINT('Origin',(263.115917770968,-19.47200726879,445.000000551893));
#57573=CARTESIAN_POINT('Origin',(263.115917770968,-19.47200726879,445.000000551893));
#57574=CARTESIAN_POINT('Origin',(263.115917770968,-19.47200726879,445.000000551893));
#57575=CARTESIAN_POINT('Origin',(263.115917770968,-19.47200726879,445.000000551893));
#57576=CARTESIAN_POINT('Origin',(263.115917770968,-19.47200726879,445.000000551893));
#57577=CARTESIAN_POINT('Origin',(263.115917770968,-19.47200726879,445.000000551893));
#57578=CARTESIAN_POINT('Origin',(263.115917770968,-19.47200726879,445.000000551893));
#57579=CARTESIAN_POINT('Origin',(263.115917770968,-19.47200726879,445.000000551893));
#57580=CARTESIAN_POINT('Origin',(263.115917770968,-19.47200726879,445.000000551893));
#57581=CARTESIAN_POINT('Origin',(263.115917770968,-19.47200726879,445.000000551893));
#57582=CARTESIAN_POINT('Origin',(263.115917770968,-19.47200726879,445.000000551893));
#57583=CARTESIAN_POINT('Origin',(263.115917770968,-19.47200726879,445.000000551893));
#57584=CARTESIAN_POINT('Origin',(263.115917770968,-19.47200726879,445.000000551893));
#57585=CARTESIAN_POINT('Origin',(263.115917770968,-19.47200726879,445.000000551893));
#57586=CARTESIAN_POINT('',(204.182688217798,-19.47200726879,447.895204466582));
#57587=CARTESIAN_POINT('',(204.182688217798,-19.47200726879,447.895204466582));
#57588=CARTESIAN_POINT('',(204.30897022363,-19.47200726879,449.821895556852));
#57589=CARTESIAN_POINT('Origin',(263.115917770968,-19.47200726879,445.000000551893));
#57590=CARTESIAN_POINT('',(204.30897022363,-19.47200726879,449.821895556852));
#57591=CARTESIAN_POINT('Origin',(213.932482630006,-19.47200726879,476.437331203026));
#57592=CARTESIAN_POINT('',(199.038536024214,-19.47200726879,452.371509792255));
#57593=CARTESIAN_POINT('Origin',(213.932482630006,-19.47200726879,476.437331203026));
#57594=CARTESIAN_POINT('',(199.038536024214,-19.47200726879,452.371509792255));
#57595=CARTESIAN_POINT('Origin',(210.249858672294,-19.4720072687899,420.25134713177));
#57596=CARTESIAN_POINT('Origin',(210.249858672294,-19.4720072687899,420.25134713177));
#57597=CARTESIAN_POINT('Origin',(263.115917770968,-19.47200726879,445.000000551893));
#57598=CARTESIAN_POINT('Origin',(263.115917770968,-19.47200726879,445.000000551893));
#57599=CARTESIAN_POINT('Origin',(263.115917770968,-19.47200726879,445.000000551893));
#57600=CARTESIAN_POINT('',(0.,0.,0.));
#57601=CARTESIAN_POINT('Origin',(375.115917770968,8.52799273120997,445.000000551893));
#57602=CARTESIAN_POINT('',(347.201102419107,10.52799273121,442.817551498303));
#57603=CARTESIAN_POINT('Origin',(375.115917770968,10.52799273121,445.000000551893));
#57604=CARTESIAN_POINT('',(345.207187036831,8.52799273120998,442.661662280189));
#57605=CARTESIAN_POINT('Origin',(347.201102419107,8.52799273120997,442.817551498303));
#57606=CARTESIAN_POINT('',(405.024648505105,8.52799273120996,447.338338823596));
#57607=CARTESIAN_POINT('Origin',(375.115917770968,8.52799273120997,445.000000551893));
#57608=CARTESIAN_POINT('Origin',(375.115917770968,8.52799273120997,445.000000551893));
#57609=CARTESIAN_POINT('Origin',(375.115917770968,0.527992731209963,445.000000551893));
#57610=CARTESIAN_POINT('',(405.024648505105,2.52799273120996,447.338338823596));
#57611=CARTESIAN_POINT('',(405.024648505105,0.527992731209953,447.338338823596));
#57612=CARTESIAN_POINT('Origin',(375.115917770968,2.52799273120996,445.000000551893));
#57613=CARTESIAN_POINT('Origin',(375.115917770968,10.52799273121,445.000000551893));
#57614=CARTESIAN_POINT('',(370.20573283719,10.52799273121,430.826430644628));
#57615=CARTESIAN_POINT('',(370.61511919622,10.52799273121,425.590136765932));
#57616=CARTESIAN_POINT('',(369.87464541018,10.52799273121,435.061234831742));
#57617=CARTESIAN_POINT('',(382.578611489874,10.52799273121,426.525472074613));
#57618=CARTESIAN_POINT('',(379.587738416461,10.52799273121,426.291638247443));
#57619=CARTESIAN_POINT('',(382.169225130845,10.52799273121,431.76176595331));
#57620=CARTESIAN_POINT('',(381.63344452432,10.52799273121,438.614717079772));
#57621=CARTESIAN_POINT('Origin',(375.115917770968,10.52799273121,445.000000551893));
#57622=CARTESIAN_POINT('Origin',(375.115917770968,2.52799273120996,445.000000551893));
#57623=CARTESIAN_POINT('',(407.018563887381,0.527992731209954,447.49422804171));
#57624=CARTESIAN_POINT('Origin',(375.115917770968,0.527992731209963,445.000000551893));
#57625=CARTESIAN_POINT('Origin',(407.01856388738,2.52799273120995,447.49422804171));
#57626=CARTESIAN_POINT('Origin',(375.115917770968,0.527992731209963,445.000000551893));
#57627=CARTESIAN_POINT('',(369.955795828192,0.527992731209939,392.88413862239));
#57628=CARTESIAN_POINT('',(368.669502598942,0.527992731209941,398.570383318602));
#57629=CARTESIAN_POINT('Origin',(395.540875463479,0.527992731209934,401.660384084767));
#57630=CARTESIAN_POINT('',(366.851654333074,0.527992731209943,398.859263942806));
#57631=CARTESIAN_POINT('Origin',(375.115917770968,0.527992731209963,445.000000551893));
#57632=CARTESIAN_POINT('',(363.86600065809,0.527992731209941,393.851889266405));
#57633=CARTESIAN_POINT('Origin',(342.261939664104,0.527992731209959,410.127126067386));
#57634=CARTESIAN_POINT('',(361.866608510987,0.527992731209941,394.332992279718));
#57635=CARTESIAN_POINT('Origin',(375.115917770968,0.527992731209963,445.000000551893));
#57636=CARTESIAN_POINT('',(361.48567633301,0.527992731209945,400.150450461139));
#57637=CARTESIAN_POINT('Origin',(388.509600623927,0.527992731209934,398.99879935135));
#57638=CARTESIAN_POINT('',(359.735399681749,0.527992731209945,400.720148606485));
#57639=CARTESIAN_POINT('Origin',(375.115917770968,0.527992731209963,445.000000551893));
#57640=CARTESIAN_POINT('',(356.003178379154,0.527992731209945,396.241482157054));
#57641=CARTESIAN_POINT('Origin',(337.211107188252,0.527992731209961,415.695963510098));
#57642=CARTESIAN_POINT('',(354.103663159699,0.527992731209945,397.029435834866));
#57643=CARTESIAN_POINT('Origin',(375.115917770968,0.527992731209963,445.000000551893));
#57644=CARTESIAN_POINT('',(354.637471847458,0.52799273120995,402.834862374034));
#57645=CARTESIAN_POINT('Origin',(381.148528861449,0.527992731209936,397.469916860725));
#57646=CARTESIAN_POINT('',(352.997864430793,0.52799273120995,403.671350181463));
#57647=CARTESIAN_POINT('Origin',(375.115917770968,0.527992731209963,445.000000551893));
#57648=CARTESIAN_POINT('',(348.610975175589,0.52799273120995,399.831671590828));
#57649=CARTESIAN_POINT('Origin',(333.0936169478,0.527992731209967,421.986363599303));
#57650=CARTESIAN_POINT('',(346.858109252615,0.52799273120995,400.907073898524));
#57651=CARTESIAN_POINT('Origin',(375.115917770968,0.527992731209963,445.000000551893));
#57652=CARTESIAN_POINT('',(348.293514664609,0.527992731209954,406.557519926939));
#57653=CARTESIAN_POINT('Origin',(373.638914192836,0.527992731209939,397.11138277388));
#57654=CARTESIAN_POINT('',(346.804949058683,0.527992731209954,407.640200290488));
#57655=CARTESIAN_POINT('Origin',(375.115917770968,0.527992731209963,445.000000551893));
#57656=CARTESIAN_POINT('',(341.871411623583,0.527992731209954,404.534055188714));
#57657=CARTESIAN_POINT('Origin',(330.010855217635,0.527992731209972,428.843435808162));
#57658=CARTESIAN_POINT('',(340.308356373543,0.527992731209956,405.870426152421));
#57659=CARTESIAN_POINT('Origin',(375.115917770968,0.527992731209963,445.000000551893));
#57660=CARTESIAN_POINT('',(342.61001406469,0.527992731209959,411.226758936108));
#57661=CARTESIAN_POINT('Origin',(366.16566825421,0.527992731209941,397.93202538994));
#57662=CARTESIAN_POINT('',(341.309143694988,0.527992731209959,412.528972672017));
#57663=CARTESIAN_POINT('Origin',(375.115917770968,0.527992731209963,445.000000551893));
#57664=CARTESIAN_POINT('',(335.950438145117,0.527992731209961,410.232844660214));
#57665=CARTESIAN_POINT('Origin',(328.038729822654,0.527992731209976,436.098336261576));
#57666=CARTESIAN_POINT('',(334.615681175749,0.527992731209961,411.797278391646));
#57667=CARTESIAN_POINT('Origin',(375.115917770968,0.527992731209963,445.000000551893));
#57668=CARTESIAN_POINT('',(337.726916694929,0.527992731209961,416.72760724082));
#57669=CARTESIAN_POINT('Origin',(358.912807162862,0.527992731209945,399.911637764141));
#57670=CARTESIAN_POINT('',(336.645773307294,0.527992731209963,418.217289525112));
#57671=CARTESIAN_POINT('Origin',(375.115917770968,0.527992731209963,445.000000551893));
#57672=CARTESIAN_POINT('',(330.993848757813,0.527992731209963,416.787716895342));
#57673=CARTESIAN_POINT('Origin',(327.225801035189,0.527992731209981,443.572425232748));
#57674=CARTESIAN_POINT('',(329.920256215508,0.527992731209963,418.541691843973));
#57675=CARTESIAN_POINT('Origin',(375.115917770968,0.527992731209963,445.000000551893));
#57676=CARTESIAN_POINT('',(333.764460618641,0.527992731209967,422.924615699545));
#57677=CARTESIAN_POINT('Origin',(352.058920429727,0.52799273120995,403.001475269873));
#57678=CARTESIAN_POINT('',(332.929665551385,0.527992731209967,424.565085610408));
#57679=CARTESIAN_POINT('Origin',(375.115917770968,0.527992731209963,445.000000551893));
#57680=CARTESIAN_POINT('',(327.123691142365,0.527992731209967,424.037269185296));
#57681=CARTESIAN_POINT('Origin',(327.592085859944,0.527992731209985,451.081665846128));
#57682=CARTESIAN_POINT('',(326.337698438563,0.527992731209972,425.937596666782));
#57683=CARTESIAN_POINT('Origin',(375.115917770968,0.527992731209963,445.000000551893));
#57684=CARTESIAN_POINT('',(330.820214655061,0.527992731209972,429.665193397337));
#57685=CARTESIAN_POINT('Origin',(345.77277349292,0.527992731209954,407.125455853163));
#57686=CARTESIAN_POINT('',(330.252323333266,0.527992731209972,431.416057121158));
#57687=CARTESIAN_POINT('Origin',(375.115917770968,0.527992731209963,445.000000551893));
#57688=CARTESIAN_POINT('',(324.435261423582,0.527992731209972,431.802993492812));
#57689=CARTESIAN_POINT('Origin',(329.128565148903,0.52799273120999,458.441155676074));
#57690=CARTESIAN_POINT('',(323.956222307212,0.527992731209976,433.802881137733));
#57691=CARTESIAN_POINT('Origin',(375.115917770968,0.527992731209963,445.000000551893));
#57692=CARTESIAN_POINT('',(328.966675911205,0.527992731209976,436.783364940581));
#57693=CARTESIAN_POINT('Origin',(340.209152152551,0.527992731209959,412.182033425343));
#57694=CARTESIAN_POINT('',(328.679671703937,0.527992731209976,438.601510401696));
#57695=CARTESIAN_POINT('Origin',(375.115917770968,0.527992731209963,445.000000551893));
#57696=CARTESIAN_POINT('',(322.994757663527,0.527992731209981,439.893671912479));
#57697=CARTESIAN_POINT('Origin',(331.797405682692,0.52799273120999,465.469679658226));
#57698=CARTESIAN_POINT('',(322.834467667472,0.527992731209981,441.943875849769));
#57699=CARTESIAN_POINT('Origin',(375.115917770968,0.527992731209963,445.000000551893));
#57700=CARTESIAN_POINT('',(328.249484662489,0.527992731209981,444.103857322026));
#57701=CARTESIAN_POINT('Origin',(335.50505123062,0.527992731209963,418.046698264767));
#57702=CARTESIAN_POINT('',(328.250434565844,0.527992731209981,445.944515745103));
#57703=CARTESIAN_POINT('Origin',(375.115917770968,0.527992731209963,445.000000551893));
#57704=CARTESIAN_POINT('',(322.837649845529,0.527992731209985,448.11008509018));
#57705=CARTESIAN_POINT('Origin',(335.532891749993,0.527992731209994,471.994172205811));
#57706=CARTESIAN_POINT('',(323.000055841466,0.527992731209985,450.160122494669));
#57707=CARTESIAN_POINT('Origin',(375.115917770968,0.527992731209963,445.000000551893));
#57708=CARTESIAN_POINT('',(328.686300537678,0.527992731209985,451.446415723918));
#57709=CARTESIAN_POINT('Origin',(331.776301303842,0.527992731209967,424.575042859381));
#57710=CARTESIAN_POINT('',(328.975181161882,0.527992731209985,453.264263989787));
#57711=CARTESIAN_POINT('Origin',(375.115917770968,0.527992731209963,445.000000551893));
#57712=CARTESIAN_POINT('',(323.96780648548,0.52799273120999,456.24991766477));
#57713=CARTESIAN_POINT('Origin',(340.243043286462,0.527992731209994,477.853978658756));
#57714=CARTESIAN_POINT('',(324.448909498793,0.52799273120999,458.249309811874));
#57715=CARTESIAN_POINT('Origin',(375.115917770968,0.527992731209963,445.000000551893));
#57716=CARTESIAN_POINT('',(330.266367680215,0.527992731209985,458.630241989851));
#57717=CARTESIAN_POINT('Origin',(329.114716570426,0.527992731209972,431.606317698934));
#57718=CARTESIAN_POINT('',(330.836065825561,0.52799273120999,460.380518641112));
#57719=CARTESIAN_POINT('Origin',(375.115917770968,0.527992731209963,445.000000551893));
#57720=CARTESIAN_POINT('',(326.357399376129,0.52799273120999,464.112739943707));
#57721=CARTESIAN_POINT('Origin',(345.811880729174,0.527992731209994,482.904811134609));
#57722=CARTESIAN_POINT('',(327.145353053941,0.527992731209994,466.012255163162));
#57723=CARTESIAN_POINT('Origin',(375.115917770968,0.527992731209963,445.000000551893));
#57724=CARTESIAN_POINT('',(332.95077959311,0.52799273120999,465.478446475402));
#57725=CARTESIAN_POINT('Origin',(327.5858340798,0.527992731209976,438.967389461411));
#57726=CARTESIAN_POINT('',(333.787267400539,0.52799273120999,467.118053892068));
#57727=CARTESIAN_POINT('Origin',(375.115917770968,0.527992731209963,445.000000551893));
#57728=CARTESIAN_POINT('',(329.947588809904,0.527992731209994,471.504943147272));
#57729=CARTESIAN_POINT('Origin',(352.102280818378,0.527992731209994,487.022301375061));
#57730=CARTESIAN_POINT('',(331.022991117599,0.527992731209994,473.257809070246));
#57731=CARTESIAN_POINT('Origin',(375.115917770968,0.527992731209963,445.000000551893));
#57732=CARTESIAN_POINT('',(336.673437146014,0.527992731209994,471.822403658252));
#57733=CARTESIAN_POINT('Origin',(327.227299992955,0.527992731209981,446.477004130025));
#57734=CARTESIAN_POINT('',(337.756117509564,0.527992731209994,473.310969264178));
#57735=CARTESIAN_POINT('Origin',(375.115917770968,0.527992731209963,445.000000551893));
#57736=CARTESIAN_POINT('',(334.64997240779,0.527992731209999,478.244506699278));
#57737=CARTESIAN_POINT('Origin',(358.959353027238,0.527992731209994,490.105063105225));
#57738=CARTESIAN_POINT('',(335.986343371497,0.527992731209999,479.807561949318));
#57739=CARTESIAN_POINT('Origin',(375.115917770968,0.527992731209963,445.000000551893));
#57740=CARTESIAN_POINT('',(341.342676155183,0.527992731209994,477.505904258171));
#57741=CARTESIAN_POINT('Origin',(328.047942609015,0.527992731209985,453.95025006865));
#57742=CARTESIAN_POINT('',(342.644889891093,0.527992731209994,478.806774627873));
#57743=CARTESIAN_POINT('Origin',(375.115917770968,0.527992731209963,445.000000551893));
#57744=CARTESIAN_POINT('',(340.34876187929,0.527992731209999,484.165480177744));
#57745=CARTESIAN_POINT('Origin',(366.214253480652,0.527992731209994,492.077188500207));
#57746=CARTESIAN_POINT('',(341.913195610722,0.527992731209999,485.500237147112));
#57747=CARTESIAN_POINT('Origin',(375.115917770968,0.527992731209963,445.000000551893));
#57748=CARTESIAN_POINT('',(346.843524459896,0.527992731209994,482.389001627931));
#57749=CARTESIAN_POINT('Origin',(330.027554983216,0.52799273120999,461.203111159998));
#57750=CARTESIAN_POINT('',(348.333206744188,0.527992731209994,483.470145015567));
#57751=CARTESIAN_POINT('Origin',(375.115917770968,0.527992731209963,445.000000551893));
#57752=CARTESIAN_POINT('',(346.903634114418,0.527992731209999,489.122069565048));
#57753=CARTESIAN_POINT('Origin',(373.688342451824,0.52799273120999,492.890117287672));
#57754=CARTESIAN_POINT('',(348.657609063049,0.527992731209999,490.195662107353));
#57755=CARTESIAN_POINT('Origin',(375.115917770968,0.527992731209963,445.000000551893));
#57756=CARTESIAN_POINT('',(353.040532918621,0.527992731209994,486.35145770422));
#57757=CARTESIAN_POINT('Origin',(333.117392488949,0.52799273120999,468.056997893134));
#57758=CARTESIAN_POINT('',(354.681002829484,0.527992731209994,487.186252771476));
#57759=CARTESIAN_POINT('Origin',(375.115917770968,0.527992731209963,445.000000551893));
#57760=CARTESIAN_POINT('',(354.153186404372,0.527992731209999,492.992227180495));
#57761=CARTESIAN_POINT('Origin',(381.197583065204,0.52799273120999,492.523832462917));
#57762=CARTESIAN_POINT('',(356.053513885857,0.527992731209999,493.778219884297));
#57763=CARTESIAN_POINT('Origin',(375.115917770968,0.527992731209963,445.000000551893));
#57764=CARTESIAN_POINT('',(359.781110616413,0.527992731209994,489.2957036678));
#57765=CARTESIAN_POINT('Origin',(337.241373072239,0.527992731209994,474.343144829941));
#57766=CARTESIAN_POINT('',(361.531974340233,0.527992731209994,489.863594989594));
#57767=CARTESIAN_POINT('Origin',(375.115917770968,0.527992731209963,445.000000551893));
#57768=CARTESIAN_POINT('',(361.918910711888,0.527992731209999,495.680656899279));
#57769=CARTESIAN_POINT('Origin',(388.55707289515,0.527992731209985,490.987353173957));
#57770=CARTESIAN_POINT('',(363.918798356808,0.527992731209994,496.159696015649));
#57771=CARTESIAN_POINT('Origin',(375.115917770968,0.527992731209963,445.000000551893));
#57772=CARTESIAN_POINT('',(366.899282159657,0.527992731209994,491.149242411656));
#57773=CARTESIAN_POINT('Origin',(342.297950644419,0.527992731209994,479.90676617031));
#57774=CARTESIAN_POINT('',(368.717427620771,0.52799273120999,491.436246618923));
#57775=CARTESIAN_POINT('Origin',(375.115917770968,0.527992731209963,445.000000551893));
#57776=CARTESIAN_POINT('',(370.009589131554,0.527992731209994,497.121160659334));
#57777=CARTESIAN_POINT('Origin',(395.585596877302,0.527992731209981,488.318512640169));
#57778=CARTESIAN_POINT('',(372.059793068845,0.527992731209994,497.281450655388));
#57779=CARTESIAN_POINT('Origin',(375.115917770968,0.527992731209963,445.000000551893));
#57780=CARTESIAN_POINT('',(374.219774541101,0.52799273120999,491.866433660372));
#57781=CARTESIAN_POINT('Origin',(348.162615483842,0.527992731209994,484.61086709224));
#57782=CARTESIAN_POINT('',(376.060432964178,0.52799273120999,491.865483757017));
#57783=CARTESIAN_POINT('Origin',(375.115917770968,0.527992731209963,445.000000551893));
#57784=CARTESIAN_POINT('',(378.226002309256,0.52799273120999,497.278268477331));
#57785=CARTESIAN_POINT('Origin',(402.110089424886,0.527992731209976,484.583026572868));
#57786=CARTESIAN_POINT('',(380.276039713744,0.52799273120999,497.115862481395));
#57787=CARTESIAN_POINT('Origin',(375.115917770968,0.527992731209963,445.000000551893));
#57788=CARTESIAN_POINT('',(381.562332942994,0.527992731209985,491.429617785183));
#57789=CARTESIAN_POINT('Origin',(354.690960078457,0.527992731209994,488.339617019018));
#57790=CARTESIAN_POINT('',(383.380181208862,0.527992731209985,491.140737160979));
#57791=CARTESIAN_POINT('Origin',(375.115917770968,0.527992731209963,445.000000551893));
#57792=CARTESIAN_POINT('',(386.365834883846,0.52799273120999,496.14811183738));
#57793=CARTESIAN_POINT('Origin',(407.969895877832,0.527992731209972,479.872875036399));
#57794=CARTESIAN_POINT('',(388.365227030949,0.527992731209985,495.667008824067));
#57795=CARTESIAN_POINT('Origin',(375.115917770968,0.527992731209963,445.000000551893));
#57796=CARTESIAN_POINT('',(388.746159208926,0.527992731209985,489.849550642646));
#57797=CARTESIAN_POINT('Origin',(361.72223491801,0.527992731209994,491.001201752435));
#57798=CARTESIAN_POINT('',(390.496435860187,0.527992731209981,489.2798524973));
#57799=CARTESIAN_POINT('Origin',(375.115917770968,0.527992731209963,445.000000551893));
#57800=CARTESIAN_POINT('',(394.228657162783,0.527992731209985,493.758518946731));
#57801=CARTESIAN_POINT('Origin',(413.020728353684,0.527992731209967,474.304037593687));
#57802=CARTESIAN_POINT('',(396.128172382238,0.527992731209981,492.970565268919));
#57803=CARTESIAN_POINT('Origin',(375.115917770968,0.527992731209963,445.000000551893));
#57804=CARTESIAN_POINT('',(395.594363694478,0.527992731209981,487.165138729751));
#57805=CARTESIAN_POINT('Origin',(369.083306680487,0.527992731209994,492.53008424306));
#57806=CARTESIAN_POINT('',(397.233971111143,0.527992731209976,486.328650922322));
#57807=CARTESIAN_POINT('Origin',(375.115917770968,0.527992731209963,445.000000551893));
#57808=CARTESIAN_POINT('',(401.620860366348,0.527992731209981,490.168329512957));
#57809=CARTESIAN_POINT('Origin',(417.138218594136,0.527992731209961,468.013637504482));
#57810=CARTESIAN_POINT('',(403.373726289321,0.527992731209976,489.092927205261));
#57811=CARTESIAN_POINT('Origin',(375.115917770968,0.527992731209963,445.000000551893));
#57812=CARTESIAN_POINT('',(401.938320877327,0.527992731209976,483.442481176847));
#57813=CARTESIAN_POINT('Origin',(376.5929213491,0.52799273120999,492.888618329905));
#57814=CARTESIAN_POINT('',(403.426886483253,0.527992731209972,482.359800813297));
#57815=CARTESIAN_POINT('Origin',(375.115917770968,0.527992731209963,445.000000551893));
#57816=CARTESIAN_POINT('',(408.360423918353,0.527992731209972,485.465945915071));
#57817=CARTESIAN_POINT('Origin',(420.220980324301,0.527992731209959,461.156565295623));
#57818=CARTESIAN_POINT('',(409.923479168393,0.527992731209972,484.129574951364));
#57819=CARTESIAN_POINT('Origin',(375.115917770968,0.527992731209963,445.000000551893));
#57820=CARTESIAN_POINT('',(407.621821477246,0.527992731209972,478.773242167677));
#57821=CARTESIAN_POINT('Origin',(384.066167287726,0.527992731209985,492.067975713845));
#57822=CARTESIAN_POINT('',(408.922691846948,0.527992731209967,477.471028431768));
#57823=CARTESIAN_POINT('Origin',(375.115917770968,0.527992731209963,445.000000551893));
#57824=CARTESIAN_POINT('',(414.28139739682,0.527992731209967,479.767156443571));
#57825=CARTESIAN_POINT('Origin',(422.193105719283,0.527992731209954,453.901664842209));
#57826=CARTESIAN_POINT('',(415.616154366188,0.527992731209967,478.202722712139));
#57827=CARTESIAN_POINT('Origin',(375.115917770968,0.527992731209963,445.000000551893));
#57828=CARTESIAN_POINT('',(412.504918847007,0.527992731209967,473.272393862965));
#57829=CARTESIAN_POINT('Origin',(391.319028379074,0.527992731209981,490.088363339644));
#57830=CARTESIAN_POINT('',(413.586062234642,0.527992731209963,471.782711578673));
#57831=CARTESIAN_POINT('Origin',(375.115917770968,0.527992731209963,445.000000551893));
#57832=CARTESIAN_POINT('',(419.237986784123,0.527992731209963,473.212284208443));
#57833=CARTESIAN_POINT('Origin',(423.006034506748,0.527992731209947,446.427575871037));
#57834=CARTESIAN_POINT('',(420.311579326428,0.527992731209963,471.458309259812));
#57835=CARTESIAN_POINT('Origin',(375.115917770968,0.527992731209963,445.000000551893));
#57836=CARTESIAN_POINT('',(416.467374923295,0.527992731209961,467.07538540424));
#57837=CARTESIAN_POINT('Origin',(398.17291511221,0.527992731209976,486.998525833912));
#57838=CARTESIAN_POINT('',(417.302169990551,0.527992731209961,465.434915493377));
#57839=CARTESIAN_POINT('Origin',(375.115917770968,0.527992731209963,445.000000551893));
#57840=CARTESIAN_POINT('',(423.108144399571,0.527992731209959,465.962731918489));
#57841=CARTESIAN_POINT('Origin',(422.639749681993,0.527992731209945,438.918335257657));
#57842=CARTESIAN_POINT('',(423.894137103373,0.527992731209959,464.062404437003));
#57843=CARTESIAN_POINT('Origin',(375.115917770968,0.527992731209963,445.000000551893));
#57844=CARTESIAN_POINT('',(419.411620886875,0.527992731209959,460.334807706448));
#57845=CARTESIAN_POINT('Origin',(404.459062049017,0.527992731209972,482.874545250622));
#57846=CARTESIAN_POINT('',(419.97951220867,0.527992731209956,458.583943982627));
#57847=CARTESIAN_POINT('Origin',(375.115917770968,0.527992731209963,445.000000551893));
#57848=CARTESIAN_POINT('',(425.796574118354,0.527992731209954,458.197007610973));
#57849=CARTESIAN_POINT('Origin',(421.103270393033,0.527992731209941,431.558845427711));
#57850=CARTESIAN_POINT('',(426.275613234725,0.527992731209952,456.197119966052));
#57851=CARTESIAN_POINT('Origin',(375.115917770968,0.527992731209963,445.000000551893));
#57852=CARTESIAN_POINT('',(421.265159630731,0.527992731209952,453.216636163204));
#57853=CARTESIAN_POINT('Origin',(410.022683389386,0.527992731209967,477.817967678442));
#57854=CARTESIAN_POINT('',(421.552163837999,0.527992731209952,451.39849070209));
#57855=CARTESIAN_POINT('Origin',(375.115917770968,0.527992731209963,445.000000551893));
#57856=CARTESIAN_POINT('',(427.23707787841,0.52799273120995,450.106329191307));
#57857=CARTESIAN_POINT('Origin',(418.434429859244,0.527992731209939,424.530321445559));
#57858=CARTESIAN_POINT('',(427.397367874464,0.527992731209947,448.056125254016));
#57859=CARTESIAN_POINT('Origin',(375.115917770968,0.527992731209963,445.000000551893));
#57860=CARTESIAN_POINT('',(421.982350879447,0.52799273120995,445.896143781759));
#57861=CARTESIAN_POINT('Origin',(414.726784311316,0.527992731209963,471.953302839018));
#57862=CARTESIAN_POINT('',(421.981400976092,0.527992731209947,444.055485358683));
#57863=CARTESIAN_POINT('Origin',(375.115917770968,0.527992731209963,445.000000551893));
#57864=CARTESIAN_POINT('',(427.394185696407,0.527992731209945,441.889916013605));
#57865=CARTESIAN_POINT('Origin',(414.698943791944,0.527992731209936,418.005828897974));
#57866=CARTESIAN_POINT('',(427.23177970047,0.527992731209943,439.839878609116));
#57867=CARTESIAN_POINT('Origin',(375.115917770968,0.527992731209963,445.000000551893));
#57868=CARTESIAN_POINT('',(421.545535004259,0.527992731209945,438.553585379867));
#57869=CARTESIAN_POINT('Origin',(418.455534238094,0.527992731209961,465.424958244404));
#57870=CARTESIAN_POINT('',(421.256654380055,0.527992731209943,436.735737113998));
#57871=CARTESIAN_POINT('Origin',(375.115917770968,0.527992731209963,445.000000551893));
#57872=CARTESIAN_POINT('',(426.264029056456,0.527992731209941,433.750083439015));
#57873=CARTESIAN_POINT('Origin',(409.988792255475,0.527992731209934,412.146022445029));
#57874=CARTESIAN_POINT('',(425.782926043143,0.527992731209939,431.750691291911));
#57875=CARTESIAN_POINT('Origin',(375.115917770968,0.527992731209963,445.000000551893));
#57876=CARTESIAN_POINT('',(419.965467861721,0.527992731209941,431.369759113934));
#57877=CARTESIAN_POINT('Origin',(421.117118971511,0.527992731209956,458.393683404851));
#57878=CARTESIAN_POINT('',(419.395769716376,0.527992731209941,429.619482462673));
#57879=CARTESIAN_POINT('Origin',(375.115917770968,0.527992731209963,445.000000551893));
#57880=CARTESIAN_POINT('',(423.874436165807,0.527992731209936,425.887261160078));
#57881=CARTESIAN_POINT('Origin',(404.419954812762,0.527992731209934,407.095189969177));
#57882=CARTESIAN_POINT('',(423.086482487995,0.527992731209936,423.987745940623));
#57883=CARTESIAN_POINT('Origin',(375.115917770968,0.527992731209963,445.000000551893));
#57884=CARTESIAN_POINT('',(417.281055948826,0.527992731209939,424.521554628383));
#57885=CARTESIAN_POINT('Origin',(422.646001462136,0.527992731209952,451.032611642374));
#57886=CARTESIAN_POINT('',(416.444568141397,0.527992731209939,422.881947211718));
#57887=CARTESIAN_POINT('Origin',(375.115917770968,0.527992731209963,445.000000551893));
#57888=CARTESIAN_POINT('',(420.284246732032,0.527992731209934,418.495057956513));
#57889=CARTESIAN_POINT('Origin',(398.129554723558,0.527992731209932,402.977699728725));
#57890=CARTESIAN_POINT('',(419.208844424337,0.527992731209934,416.742192033539));
#57891=CARTESIAN_POINT('Origin',(375.115917770968,0.527992731209963,445.000000551893));
#57892=CARTESIAN_POINT('',(413.558398395922,0.527992731209936,418.177597445533));
#57893=CARTESIAN_POINT('Origin',(423.004535548981,0.527992731209947,443.522996973761));
#57894=CARTESIAN_POINT('',(412.475718032372,0.527992731209936,416.689031839608));
#57895=CARTESIAN_POINT('Origin',(375.115917770968,0.527992731209963,445.000000551893));
#57896=CARTESIAN_POINT('',(415.581863134147,0.527992731209932,411.755494404508));
#57897=CARTESIAN_POINT('Origin',(391.272482514698,0.527992731209934,399.89493799856));
#57898=CARTESIAN_POINT('',(414.245492170439,0.527992731209932,410.192439154467));
#57899=CARTESIAN_POINT('Origin',(375.115917770968,0.527992731209963,445.000000551893));
#57900=CARTESIAN_POINT('',(408.889159386753,0.527992731209934,412.494096845614));
#57901=CARTESIAN_POINT('Origin',(422.183892932921,0.527992731209943,436.049751035135));
#57902=CARTESIAN_POINT('',(407.586945650843,0.527992731209934,411.193226475912));
#57903=CARTESIAN_POINT('Origin',(375.115917770968,0.527992731209963,445.000000551893));
#57904=CARTESIAN_POINT('',(409.883073662646,0.52799273120993,405.834520926041));
#57905=CARTESIAN_POINT('Origin',(384.017582061284,0.527992731209936,397.922812603578));
#57906=CARTESIAN_POINT('',(408.318639931215,0.52799273120993,404.499763956673));
#57907=CARTESIAN_POINT('Origin',(375.115917770968,0.527992731209963,445.000000551893));
#57908=CARTESIAN_POINT('',(403.38831108204,0.527992731209934,407.610999475854));
#57909=CARTESIAN_POINT('Origin',(420.20428055872,0.527992731209939,428.796889943787));
#57910=CARTESIAN_POINT('',(401.898628797749,0.527992731209934,406.529856088218));
#57911=CARTESIAN_POINT('Origin',(375.115917770968,0.527992731209963,445.000000551893));
#57912=CARTESIAN_POINT('',(403.328201427518,0.52799273120993,400.877931538737));
#57913=CARTESIAN_POINT('Origin',(376.543493090113,0.527992731209939,397.109883816113));
#57914=CARTESIAN_POINT('',(401.574226478887,0.52799273120993,399.804338996432));
#57915=CARTESIAN_POINT('Origin',(375.115917770968,0.527992731209963,445.000000551893));
#57916=CARTESIAN_POINT('',(397.191302623315,0.527992731209934,403.648543399565));
#57917=CARTESIAN_POINT('Origin',(417.114443052987,0.527992731209936,421.943003210651));
#57918=CARTESIAN_POINT('',(395.550832712453,0.527992731209934,402.813748332309));
#57919=CARTESIAN_POINT('Origin',(375.115917770968,0.527992731209963,445.000000551893));
#57920=CARTESIAN_POINT('',(396.078649137564,0.52799273120993,397.00777392329));
#57921=CARTESIAN_POINT('Origin',(369.034252476732,0.527992731209941,397.476168640868));
#57922=CARTESIAN_POINT('',(394.178321656079,0.52799273120993,396.221781219488));
#57923=CARTESIAN_POINT('Origin',(375.115917770968,0.527992731209963,445.000000551893));
#57924=CARTESIAN_POINT('',(390.450724925524,0.527992731209934,400.704297435985));
#57925=CARTESIAN_POINT('Origin',(412.990462469698,0.527992731209934,415.656856273844));
#57926=CARTESIAN_POINT('',(388.699861201703,0.527992731209934,400.136406114191));
#57927=CARTESIAN_POINT('Origin',(375.115917770968,0.527992731209963,445.000000551893));
#57928=CARTESIAN_POINT('',(388.312924830048,0.527992731209932,394.319344204506));
#57929=CARTESIAN_POINT('Origin',(361.674762646786,0.527992731209943,399.012647929828));
#57930=CARTESIAN_POINT('',(386.313037185128,0.527992731209932,393.840305088136));
#57931=CARTESIAN_POINT('Origin',(375.115917770968,0.527992731209963,445.000000551893));
#57932=CARTESIAN_POINT('',(383.33255338228,0.527992731209936,398.850758692129));
#57933=CARTESIAN_POINT('Origin',(407.933884897518,0.527992731209934,410.093234933475));
#57934=CARTESIAN_POINT('',(381.514407921165,0.527992731209936,398.563754484862));
#57935=CARTESIAN_POINT('Origin',(375.115917770968,0.527992731209963,445.000000551893));
#57936=CARTESIAN_POINT('',(380.222246410382,0.527992731209934,392.878840444451));
#57937=CARTESIAN_POINT('Origin',(354.646238664634,0.527992731209947,401.681488463616));
#57938=CARTESIAN_POINT('',(378.172042473091,0.527992731209934,392.718550448397));
#57939=CARTESIAN_POINT('Origin',(375.115917770968,0.527992731209963,445.000000551893));
#57940=CARTESIAN_POINT('',(376.012061000835,0.527992731209939,398.133567443413));
#57941=CARTESIAN_POINT('Origin',(402.069220058094,0.527992731209932,405.389134011545));
#57942=CARTESIAN_POINT('',(374.171402577758,0.527992731209939,398.134517346768));
#57943=CARTESIAN_POINT('Origin',(375.115917770968,0.527992731209963,445.000000551893));
#57944=CARTESIAN_POINT('',(372.005833232681,0.527992731209936,392.721732626454));
#57945=CARTESIAN_POINT('Origin',(348.12174611705,0.527992731209952,405.416974530917));
#57946=CARTESIAN_POINT('Origin',(375.115917770968,0.527992731209963,445.000000551893));
#57947=CARTESIAN_POINT('Origin',(370.61511919622,0.527992731209956,425.590136765932));
#57948=CARTESIAN_POINT('',(382.578611489874,-19.4720072687901,426.525472074613));
#57949=CARTESIAN_POINT('',(370.61511919622,-19.47200726879,425.590136765932));
#57950=CARTESIAN_POINT('',(373.605992269633,-19.47200726879,425.823970593102));
#57951=CARTESIAN_POINT('',(382.578611489874,0.527992731209952,426.525472074613));
#57952=CARTESIAN_POINT('',(370.61511919622,0.527992731209956,425.590136765932));
#57953=CARTESIAN_POINT('Origin',(369.991562323765,0.527992731209961,433.565798295035));
#57954=CARTESIAN_POINT('',(370.20573283719,-19.47200726879,430.826430644628));
#57955=CARTESIAN_POINT('',(369.562866973953,-19.47200726879,439.049065596293));
#57956=CARTESIAN_POINT('',(370.20573283719,0.527992731209959,430.826430644628));
#57957=CARTESIAN_POINT('Origin',(375.115917770968,0.527992731209963,445.000000551893));
#57958=CARTESIAN_POINT('',(382.169225130845,-19.47200726879,431.76176595331));
#57959=CARTESIAN_POINT('Origin',(375.115917770968,-19.47200726879,445.000000551893));
#57960=CARTESIAN_POINT('',(382.169225130845,0.527992731209954,431.76176595331));
#57961=CARTESIAN_POINT('Origin',(382.578611489874,0.527992731209952,426.525472074613));
#57962=CARTESIAN_POINT('',(381.838137703835,-19.47200726879,435.996570140423));
#57963=CARTESIAN_POINT('Origin',(375.115917770968,-19.47200726879,445.000000551893));
#57964=CARTESIAN_POINT('',(368.669502598942,-19.4720072687901,398.570383318602));
#57965=CARTESIAN_POINT('',(368.669502598942,-19.4720072687901,398.570383318602));
#57966=CARTESIAN_POINT('',(366.851654333074,-19.4720072687901,398.859263942806));
#57967=CARTESIAN_POINT('Origin',(375.115917770968,-19.47200726879,445.000000551893));
#57968=CARTESIAN_POINT('',(366.851654333074,-19.4720072687901,398.859263942806));
#57969=CARTESIAN_POINT('Origin',(342.261939664104,-19.47200726879,410.127126067386));
#57970=CARTESIAN_POINT('',(363.86600065809,-19.4720072687901,393.851889266405));
#57971=CARTESIAN_POINT('Origin',(342.261939664104,-19.47200726879,410.127126067386));
#57972=CARTESIAN_POINT('',(363.86600065809,-19.4720072687901,393.851889266405));
#57973=CARTESIAN_POINT('Origin',(395.540875463479,-19.4720072687901,401.660384084767));
#57974=CARTESIAN_POINT('',(369.955795828192,-19.4720072687901,392.88413862239));
#57975=CARTESIAN_POINT('',(369.955795828192,-19.4720072687901,392.88413862239));
#57976=CARTESIAN_POINT('Origin',(395.540875463479,-19.4720072687901,401.660384084767));
#57977=CARTESIAN_POINT('Origin',(375.115917770968,-19.47200726879,445.000000551893));
#57978=CARTESIAN_POINT('',(361.48567633301,-19.4720072687901,400.150450461139));
#57979=CARTESIAN_POINT('',(361.48567633301,-19.4720072687901,400.150450461139));
#57980=CARTESIAN_POINT('',(359.735399681749,-19.4720072687901,400.720148606485));
#57981=CARTESIAN_POINT('Origin',(375.115917770968,-19.47200726879,445.000000551893));
#57982=CARTESIAN_POINT('',(359.735399681749,-19.4720072687901,400.720148606485));
#57983=CARTESIAN_POINT('Origin',(337.211107188252,-19.47200726879,415.695963510098));
#57984=CARTESIAN_POINT('',(356.003178379154,-19.4720072687901,396.241482157054));
#57985=CARTESIAN_POINT('Origin',(337.211107188252,-19.47200726879,415.695963510098));
#57986=CARTESIAN_POINT('',(356.003178379154,-19.4720072687901,396.241482157054));
#57987=CARTESIAN_POINT('Origin',(388.509600623927,-19.4720072687901,398.99879935135));
#57988=CARTESIAN_POINT('',(361.866608510987,-19.4720072687901,394.332992279718));
#57989=CARTESIAN_POINT('',(361.866608510987,-19.4720072687901,394.332992279718));
#57990=CARTESIAN_POINT('Origin',(388.509600623927,-19.4720072687901,398.99879935135));
#57991=CARTESIAN_POINT('Origin',(375.115917770968,-19.47200726879,445.000000551893));
#57992=CARTESIAN_POINT('',(354.637471847458,-19.4720072687901,402.834862374034));
#57993=CARTESIAN_POINT('',(354.637471847458,-19.4720072687901,402.834862374034));
#57994=CARTESIAN_POINT('',(352.997864430793,-19.4720072687901,403.671350181463));
#57995=CARTESIAN_POINT('Origin',(375.115917770968,-19.47200726879,445.000000551893));
#57996=CARTESIAN_POINT('',(352.997864430793,-19.4720072687901,403.671350181463));
#57997=CARTESIAN_POINT('Origin',(333.0936169478,-19.47200726879,421.986363599303));
#57998=CARTESIAN_POINT('',(348.610975175589,-19.4720072687901,399.831671590828));
#57999=CARTESIAN_POINT('Origin',(333.0936169478,-19.47200726879,421.986363599303));
#58000=CARTESIAN_POINT('',(348.610975175589,-19.4720072687901,399.831671590828));
#58001=CARTESIAN_POINT('Origin',(381.148528861449,-19.4720072687901,397.469916860725));
#58002=CARTESIAN_POINT('',(354.103663159699,-19.4720072687901,397.029435834866));
#58003=CARTESIAN_POINT('',(354.103663159699,-19.4720072687901,397.029435834866));
#58004=CARTESIAN_POINT('Origin',(381.148528861449,-19.4720072687901,397.469916860725));
#58005=CARTESIAN_POINT('Origin',(375.115917770968,-19.47200726879,445.000000551893));
#58006=CARTESIAN_POINT('',(348.293514664609,-19.47200726879,406.557519926939));
#58007=CARTESIAN_POINT('',(348.293514664609,-19.47200726879,406.557519926939));
#58008=CARTESIAN_POINT('',(346.804949058683,-19.47200726879,407.640200290488));
#58009=CARTESIAN_POINT('Origin',(375.115917770968,-19.47200726879,445.000000551893));
#58010=CARTESIAN_POINT('',(346.804949058683,-19.47200726879,407.640200290488));
#58011=CARTESIAN_POINT('Origin',(330.010855217635,-19.47200726879,428.843435808162));
#58012=CARTESIAN_POINT('',(341.871411623583,-19.47200726879,404.534055188714));
#58013=CARTESIAN_POINT('Origin',(330.010855217635,-19.47200726879,428.843435808162));
#58014=CARTESIAN_POINT('',(341.871411623583,-19.47200726879,404.534055188714));
#58015=CARTESIAN_POINT('Origin',(373.638914192836,-19.4720072687901,397.11138277388));
#58016=CARTESIAN_POINT('',(346.858109252615,-19.4720072687901,400.907073898524));
#58017=CARTESIAN_POINT('',(346.858109252615,-19.4720072687901,400.907073898524));
#58018=CARTESIAN_POINT('Origin',(373.638914192836,-19.4720072687901,397.11138277388));
#58019=CARTESIAN_POINT('Origin',(375.115917770968,-19.47200726879,445.000000551893));
#58020=CARTESIAN_POINT('',(342.61001406469,-19.47200726879,411.226758936108));
#58021=CARTESIAN_POINT('',(342.61001406469,-19.47200726879,411.226758936108));
#58022=CARTESIAN_POINT('',(341.309143694988,-19.47200726879,412.528972672017));
#58023=CARTESIAN_POINT('Origin',(375.115917770968,-19.47200726879,445.000000551893));
#58024=CARTESIAN_POINT('',(341.309143694988,-19.47200726879,412.528972672017));
#58025=CARTESIAN_POINT('Origin',(328.038729822654,-19.47200726879,436.098336261576));
#58026=CARTESIAN_POINT('',(335.950438145117,-19.47200726879,410.232844660214));
#58027=CARTESIAN_POINT('Origin',(328.038729822654,-19.47200726879,436.098336261576));
#58028=CARTESIAN_POINT('',(335.950438145117,-19.47200726879,410.232844660214));
#58029=CARTESIAN_POINT('Origin',(366.16566825421,-19.4720072687901,397.93202538994));
#58030=CARTESIAN_POINT('',(340.308356373543,-19.47200726879,405.870426152421));
#58031=CARTESIAN_POINT('',(340.308356373543,-19.47200726879,405.870426152421));
#58032=CARTESIAN_POINT('Origin',(366.16566825421,-19.4720072687901,397.93202538994));
#58033=CARTESIAN_POINT('Origin',(375.115917770968,-19.47200726879,445.000000551893));
#58034=CARTESIAN_POINT('',(337.726916694929,-19.47200726879,416.72760724082));
#58035=CARTESIAN_POINT('',(337.726916694929,-19.47200726879,416.72760724082));
#58036=CARTESIAN_POINT('',(336.645773307294,-19.47200726879,418.217289525112));
#58037=CARTESIAN_POINT('Origin',(375.115917770968,-19.47200726879,445.000000551893));
#58038=CARTESIAN_POINT('',(336.645773307294,-19.47200726879,418.217289525112));
#58039=CARTESIAN_POINT('Origin',(327.225801035189,-19.47200726879,443.572425232748));
#58040=CARTESIAN_POINT('',(330.993848757813,-19.47200726879,416.787716895342));
#58041=CARTESIAN_POINT('Origin',(327.225801035189,-19.47200726879,443.572425232748));
#58042=CARTESIAN_POINT('',(330.993848757813,-19.47200726879,416.787716895342));
#58043=CARTESIAN_POINT('Origin',(358.912807162862,-19.4720072687901,399.911637764141));
#58044=CARTESIAN_POINT('',(334.615681175749,-19.47200726879,411.797278391646));
#58045=CARTESIAN_POINT('',(334.615681175749,-19.47200726879,411.797278391646));
#58046=CARTESIAN_POINT('Origin',(358.912807162862,-19.4720072687901,399.911637764141));
#58047=CARTESIAN_POINT('Origin',(375.115917770968,-19.47200726879,445.000000551893));
#58048=CARTESIAN_POINT('',(333.764460618641,-19.47200726879,422.924615699545));
#58049=CARTESIAN_POINT('',(333.764460618641,-19.47200726879,422.924615699545));
#58050=CARTESIAN_POINT('',(332.929665551385,-19.47200726879,424.565085610408));
#58051=CARTESIAN_POINT('Origin',(375.115917770968,-19.47200726879,445.000000551893));
#58052=CARTESIAN_POINT('',(332.929665551385,-19.47200726879,424.565085610408));
#58053=CARTESIAN_POINT('Origin',(327.592085859944,-19.47200726879,451.081665846128));
#58054=CARTESIAN_POINT('',(327.123691142365,-19.47200726879,424.037269185296));
#58055=CARTESIAN_POINT('Origin',(327.592085859944,-19.47200726879,451.081665846128));
#58056=CARTESIAN_POINT('',(327.123691142365,-19.47200726879,424.037269185296));
#58057=CARTESIAN_POINT('Origin',(352.058920429727,-19.4720072687901,403.001475269873));
#58058=CARTESIAN_POINT('',(329.920256215508,-19.47200726879,418.541691843973));
#58059=CARTESIAN_POINT('',(329.920256215508,-19.47200726879,418.541691843973));
#58060=CARTESIAN_POINT('Origin',(352.058920429727,-19.4720072687901,403.001475269873));
#58061=CARTESIAN_POINT('Origin',(375.115917770968,-19.47200726879,445.000000551893));
#58062=CARTESIAN_POINT('',(330.820214655061,-19.47200726879,429.665193397337));
#58063=CARTESIAN_POINT('',(330.820214655061,-19.47200726879,429.665193397337));
#58064=CARTESIAN_POINT('',(330.252323333266,-19.47200726879,431.416057121158));
#58065=CARTESIAN_POINT('Origin',(375.115917770968,-19.47200726879,445.000000551893));
#58066=CARTESIAN_POINT('',(330.252323333266,-19.47200726879,431.416057121158));
#58067=CARTESIAN_POINT('Origin',(329.128565148903,-19.47200726879,458.441155676074));
#58068=CARTESIAN_POINT('',(324.435261423582,-19.47200726879,431.802993492812));
#58069=CARTESIAN_POINT('Origin',(329.128565148903,-19.47200726879,458.441155676074));
#58070=CARTESIAN_POINT('',(324.435261423582,-19.47200726879,431.802993492812));
#58071=CARTESIAN_POINT('Origin',(345.77277349292,-19.47200726879,407.125455853163));
#58072=CARTESIAN_POINT('',(326.337698438563,-19.47200726879,425.937596666782));
#58073=CARTESIAN_POINT('',(326.337698438563,-19.47200726879,425.937596666782));
#58074=CARTESIAN_POINT('Origin',(345.77277349292,-19.47200726879,407.125455853163));
#58075=CARTESIAN_POINT('Origin',(375.115917770968,-19.47200726879,445.000000551893));
#58076=CARTESIAN_POINT('',(328.966675911205,-19.47200726879,436.783364940581));
#58077=CARTESIAN_POINT('',(328.966675911205,-19.47200726879,436.783364940581));
#58078=CARTESIAN_POINT('',(328.679671703937,-19.47200726879,438.601510401696));
#58079=CARTESIAN_POINT('Origin',(375.115917770968,-19.47200726879,445.000000551893));
#58080=CARTESIAN_POINT('',(328.679671703937,-19.47200726879,438.601510401696));
#58081=CARTESIAN_POINT('Origin',(331.797405682692,-19.47200726879,465.469679658226));
#58082=CARTESIAN_POINT('',(322.994757663527,-19.47200726879,439.893671912479));
#58083=CARTESIAN_POINT('Origin',(331.797405682692,-19.47200726879,465.469679658226));
#58084=CARTESIAN_POINT('',(322.994757663527,-19.47200726879,439.893671912479));
#58085=CARTESIAN_POINT('Origin',(340.209152152551,-19.47200726879,412.182033425343));
#58086=CARTESIAN_POINT('',(323.956222307212,-19.47200726879,433.802881137733));
#58087=CARTESIAN_POINT('',(323.956222307212,-19.47200726879,433.802881137733));
#58088=CARTESIAN_POINT('Origin',(340.209152152551,-19.47200726879,412.182033425343));
#58089=CARTESIAN_POINT('Origin',(375.115917770968,-19.47200726879,445.000000551893));
#58090=CARTESIAN_POINT('',(328.249484662489,-19.47200726879,444.103857322026));
#58091=CARTESIAN_POINT('',(328.249484662489,-19.47200726879,444.103857322026));
#58092=CARTESIAN_POINT('',(328.250434565844,-19.47200726879,445.944515745103));
#58093=CARTESIAN_POINT('Origin',(375.115917770968,-19.47200726879,445.000000551893));
#58094=CARTESIAN_POINT('',(328.250434565844,-19.47200726879,445.944515745103));
#58095=CARTESIAN_POINT('Origin',(335.532891749993,-19.47200726879,471.994172205811));
#58096=CARTESIAN_POINT('',(322.837649845529,-19.47200726879,448.11008509018));
#58097=CARTESIAN_POINT('Origin',(335.532891749993,-19.47200726879,471.994172205811));
#58098=CARTESIAN_POINT('',(322.837649845529,-19.47200726879,448.11008509018));
#58099=CARTESIAN_POINT('Origin',(335.50505123062,-19.47200726879,418.046698264767));
#58100=CARTESIAN_POINT('',(322.834467667472,-19.47200726879,441.943875849769));
#58101=CARTESIAN_POINT('',(322.834467667472,-19.47200726879,441.943875849769));
#58102=CARTESIAN_POINT('Origin',(335.50505123062,-19.47200726879,418.046698264767));
#58103=CARTESIAN_POINT('Origin',(375.115917770968,-19.47200726879,445.000000551893));
#58104=CARTESIAN_POINT('',(328.686300537678,-19.47200726879,451.446415723918));
#58105=CARTESIAN_POINT('',(328.686300537678,-19.47200726879,451.446415723918));
#58106=CARTESIAN_POINT('',(328.975181161882,-19.47200726879,453.264263989787));
#58107=CARTESIAN_POINT('Origin',(375.115917770968,-19.47200726879,445.000000551893));
#58108=CARTESIAN_POINT('',(328.975181161882,-19.47200726879,453.264263989787));
#58109=CARTESIAN_POINT('Origin',(340.243043286461,-19.47200726879,477.853978658756));
#58110=CARTESIAN_POINT('',(323.96780648548,-19.47200726879,456.24991766477));
#58111=CARTESIAN_POINT('Origin',(340.243043286461,-19.47200726879,477.853978658756));
#58112=CARTESIAN_POINT('',(323.96780648548,-19.47200726879,456.24991766477));
#58113=CARTESIAN_POINT('Origin',(331.776301303842,-19.47200726879,424.575042859381));
#58114=CARTESIAN_POINT('',(323.000055841466,-19.47200726879,450.160122494669));
#58115=CARTESIAN_POINT('',(323.000055841466,-19.47200726879,450.160122494669));
#58116=CARTESIAN_POINT('Origin',(331.776301303842,-19.47200726879,424.575042859381));
#58117=CARTESIAN_POINT('Origin',(375.115917770968,-19.47200726879,445.000000551893));
#58118=CARTESIAN_POINT('',(330.266367680215,-19.47200726879,458.630241989851));
#58119=CARTESIAN_POINT('',(330.266367680215,-19.47200726879,458.630241989851));
#58120=CARTESIAN_POINT('',(330.836065825561,-19.47200726879,460.380518641112));
#58121=CARTESIAN_POINT('Origin',(375.115917770968,-19.47200726879,445.000000551893));
#58122=CARTESIAN_POINT('',(330.836065825561,-19.47200726879,460.380518641112));
#58123=CARTESIAN_POINT('Origin',(345.811880729174,-19.47200726879,482.904811134609));
#58124=CARTESIAN_POINT('',(326.357399376129,-19.47200726879,464.112739943707));
#58125=CARTESIAN_POINT('Origin',(345.811880729174,-19.47200726879,482.904811134609));
#58126=CARTESIAN_POINT('',(326.357399376129,-19.47200726879,464.112739943707));
#58127=CARTESIAN_POINT('Origin',(329.114716570426,-19.47200726879,431.606317698934));
#58128=CARTESIAN_POINT('',(324.448909498793,-19.47200726879,458.249309811874));
#58129=CARTESIAN_POINT('',(324.448909498793,-19.47200726879,458.249309811874));
#58130=CARTESIAN_POINT('Origin',(329.114716570426,-19.47200726879,431.606317698934));
#58131=CARTESIAN_POINT('Origin',(375.115917770968,-19.47200726879,445.000000551893));
#58132=CARTESIAN_POINT('',(332.95077959311,-19.47200726879,465.478446475402));
#58133=CARTESIAN_POINT('',(332.95077959311,-19.47200726879,465.478446475402));
#58134=CARTESIAN_POINT('',(333.787267400539,-19.47200726879,467.118053892068));
#58135=CARTESIAN_POINT('Origin',(375.115917770968,-19.47200726879,445.000000551893));
#58136=CARTESIAN_POINT('',(333.787267400539,-19.47200726879,467.118053892068));
#58137=CARTESIAN_POINT('Origin',(352.102280818378,-19.47200726879,487.022301375061));
#58138=CARTESIAN_POINT('',(329.947588809904,-19.47200726879,471.504943147272));
#58139=CARTESIAN_POINT('Origin',(352.102280818378,-19.47200726879,487.022301375061));
#58140=CARTESIAN_POINT('',(329.947588809904,-19.47200726879,471.504943147272));
#58141=CARTESIAN_POINT('Origin',(327.5858340798,-19.47200726879,438.967389461411));
#58142=CARTESIAN_POINT('',(327.145353053941,-19.47200726879,466.012255163162));
#58143=CARTESIAN_POINT('',(327.145353053941,-19.47200726879,466.012255163162));
#58144=CARTESIAN_POINT('Origin',(327.5858340798,-19.47200726879,438.967389461411));
#58145=CARTESIAN_POINT('Origin',(375.115917770968,-19.47200726879,445.000000551893));
#58146=CARTESIAN_POINT('',(336.673437146014,-19.47200726879,471.822403658252));
#58147=CARTESIAN_POINT('',(336.673437146014,-19.47200726879,471.822403658252));
#58148=CARTESIAN_POINT('',(337.756117509564,-19.47200726879,473.310969264178));
#58149=CARTESIAN_POINT('Origin',(375.115917770968,-19.47200726879,445.000000551893));
#58150=CARTESIAN_POINT('',(337.756117509564,-19.47200726879,473.310969264178));
#58151=CARTESIAN_POINT('Origin',(358.959353027238,-19.47200726879,490.105063105225));
#58152=CARTESIAN_POINT('',(334.64997240779,-19.47200726879,478.244506699278));
#58153=CARTESIAN_POINT('Origin',(358.959353027238,-19.47200726879,490.105063105225));
#58154=CARTESIAN_POINT('',(334.64997240779,-19.47200726879,478.244506699278));
#58155=CARTESIAN_POINT('Origin',(327.227299992955,-19.47200726879,446.477004130025));
#58156=CARTESIAN_POINT('',(331.022991117599,-19.47200726879,473.257809070246));
#58157=CARTESIAN_POINT('',(331.022991117599,-19.47200726879,473.257809070246));
#58158=CARTESIAN_POINT('Origin',(327.227299992955,-19.47200726879,446.477004130025));
#58159=CARTESIAN_POINT('Origin',(375.115917770968,-19.47200726879,445.000000551893));
#58160=CARTESIAN_POINT('',(341.342676155183,-19.47200726879,477.505904258171));
#58161=CARTESIAN_POINT('',(341.342676155183,-19.47200726879,477.505904258171));
#58162=CARTESIAN_POINT('',(342.644889891093,-19.47200726879,478.806774627873));
#58163=CARTESIAN_POINT('Origin',(375.115917770968,-19.47200726879,445.000000551893));
#58164=CARTESIAN_POINT('',(342.644889891093,-19.47200726879,478.806774627873));
#58165=CARTESIAN_POINT('Origin',(366.214253480652,-19.47200726879,492.077188500207));
#58166=CARTESIAN_POINT('',(340.34876187929,-19.47200726879,484.165480177744));
#58167=CARTESIAN_POINT('Origin',(366.214253480652,-19.47200726879,492.077188500207));
#58168=CARTESIAN_POINT('',(340.34876187929,-19.47200726879,484.165480177744));
#58169=CARTESIAN_POINT('Origin',(328.047942609015,-19.47200726879,453.95025006865));
#58170=CARTESIAN_POINT('',(335.986343371497,-19.47200726879,479.807561949318));
#58171=CARTESIAN_POINT('',(335.986343371497,-19.47200726879,479.807561949318));
#58172=CARTESIAN_POINT('Origin',(328.047942609015,-19.47200726879,453.95025006865));
#58173=CARTESIAN_POINT('Origin',(375.115917770968,-19.47200726879,445.000000551893));
#58174=CARTESIAN_POINT('',(346.843524459896,-19.47200726879,482.389001627931));
#58175=CARTESIAN_POINT('',(346.843524459896,-19.47200726879,482.389001627931));
#58176=CARTESIAN_POINT('',(348.333206744188,-19.47200726879,483.470145015567));
#58177=CARTESIAN_POINT('Origin',(375.115917770968,-19.47200726879,445.000000551893));
#58178=CARTESIAN_POINT('',(348.333206744188,-19.47200726879,483.470145015567));
#58179=CARTESIAN_POINT('Origin',(373.688342451824,-19.47200726879,492.890117287672));
#58180=CARTESIAN_POINT('',(346.903634114418,-19.47200726879,489.122069565048));
#58181=CARTESIAN_POINT('Origin',(373.688342451824,-19.47200726879,492.890117287672));
#58182=CARTESIAN_POINT('',(346.903634114418,-19.47200726879,489.122069565048));
#58183=CARTESIAN_POINT('Origin',(330.027554983216,-19.47200726879,461.203111159998));
#58184=CARTESIAN_POINT('',(341.913195610722,-19.47200726879,485.500237147112));
#58185=CARTESIAN_POINT('',(341.913195610722,-19.47200726879,485.500237147112));
#58186=CARTESIAN_POINT('Origin',(330.027554983216,-19.47200726879,461.203111159998));
#58187=CARTESIAN_POINT('Origin',(375.115917770968,-19.47200726879,445.000000551893));
#58188=CARTESIAN_POINT('',(353.040532918621,-19.47200726879,486.35145770422));
#58189=CARTESIAN_POINT('',(353.040532918621,-19.47200726879,486.35145770422));
#58190=CARTESIAN_POINT('',(354.681002829484,-19.47200726879,487.186252771476));
#58191=CARTESIAN_POINT('Origin',(375.115917770968,-19.47200726879,445.000000551893));
#58192=CARTESIAN_POINT('',(354.681002829484,-19.47200726879,487.186252771476));
#58193=CARTESIAN_POINT('Origin',(381.197583065204,-19.47200726879,492.523832462917));
#58194=CARTESIAN_POINT('',(354.153186404372,-19.47200726879,492.992227180495));
#58195=CARTESIAN_POINT('Origin',(381.197583065204,-19.47200726879,492.523832462917));
#58196=CARTESIAN_POINT('',(354.153186404372,-19.47200726879,492.992227180495));
#58197=CARTESIAN_POINT('Origin',(333.117392488949,-19.47200726879,468.056997893134));
#58198=CARTESIAN_POINT('',(348.657609063049,-19.47200726879,490.195662107353));
#58199=CARTESIAN_POINT('',(348.657609063049,-19.47200726879,490.195662107353));
#58200=CARTESIAN_POINT('Origin',(333.117392488949,-19.47200726879,468.056997893134));
#58201=CARTESIAN_POINT('Origin',(375.115917770968,-19.47200726879,445.000000551893));
#58202=CARTESIAN_POINT('',(359.781110616413,-19.47200726879,489.2957036678));
#58203=CARTESIAN_POINT('',(359.781110616413,-19.47200726879,489.2957036678));
#58204=CARTESIAN_POINT('',(361.531974340233,-19.47200726879,489.863594989594));
#58205=CARTESIAN_POINT('Origin',(375.115917770968,-19.47200726879,445.000000551893));
#58206=CARTESIAN_POINT('',(361.531974340233,-19.47200726879,489.863594989594));
#58207=CARTESIAN_POINT('Origin',(388.55707289515,-19.47200726879,490.987353173957));
#58208=CARTESIAN_POINT('',(361.918910711888,-19.47200726879,495.680656899279));
#58209=CARTESIAN_POINT('Origin',(388.55707289515,-19.47200726879,490.987353173957));
#58210=CARTESIAN_POINT('',(361.918910711888,-19.47200726879,495.680656899279));
#58211=CARTESIAN_POINT('Origin',(337.241373072239,-19.47200726879,474.343144829941));
#58212=CARTESIAN_POINT('',(356.053513885857,-19.47200726879,493.778219884297));
#58213=CARTESIAN_POINT('',(356.053513885857,-19.47200726879,493.778219884297));
#58214=CARTESIAN_POINT('Origin',(337.241373072239,-19.47200726879,474.343144829941));
#58215=CARTESIAN_POINT('Origin',(375.115917770968,-19.47200726879,445.000000551893));
#58216=CARTESIAN_POINT('',(366.899282159657,-19.47200726879,491.149242411656));
#58217=CARTESIAN_POINT('',(366.899282159657,-19.47200726879,491.149242411656));
#58218=CARTESIAN_POINT('',(368.717427620771,-19.47200726879,491.436246618923));
#58219=CARTESIAN_POINT('Origin',(375.115917770968,-19.47200726879,445.000000551893));
#58220=CARTESIAN_POINT('',(368.717427620771,-19.47200726879,491.436246618923));
#58221=CARTESIAN_POINT('Origin',(395.585596877302,-19.47200726879,488.318512640169));
#58222=CARTESIAN_POINT('',(370.009589131554,-19.47200726879,497.121160659334));
#58223=CARTESIAN_POINT('Origin',(395.585596877302,-19.47200726879,488.318512640169));
#58224=CARTESIAN_POINT('',(370.009589131554,-19.47200726879,497.121160659334));
#58225=CARTESIAN_POINT('Origin',(342.297950644419,-19.47200726879,479.90676617031));
#58226=CARTESIAN_POINT('',(363.918798356808,-19.47200726879,496.159696015649));
#58227=CARTESIAN_POINT('',(363.918798356808,-19.47200726879,496.159696015649));
#58228=CARTESIAN_POINT('Origin',(342.297950644419,-19.47200726879,479.90676617031));
#58229=CARTESIAN_POINT('Origin',(375.115917770968,-19.47200726879,445.000000551893));
#58230=CARTESIAN_POINT('',(374.219774541101,-19.47200726879,491.866433660372));
#58231=CARTESIAN_POINT('',(374.219774541101,-19.47200726879,491.866433660372));
#58232=CARTESIAN_POINT('',(376.060432964178,-19.47200726879,491.865483757017));
#58233=CARTESIAN_POINT('Origin',(375.115917770968,-19.47200726879,445.000000551893));
#58234=CARTESIAN_POINT('',(376.060432964178,-19.47200726879,491.865483757017));
#58235=CARTESIAN_POINT('Origin',(402.110089424886,-19.47200726879,484.583026572868));
#58236=CARTESIAN_POINT('',(378.226002309256,-19.47200726879,497.278268477331));
#58237=CARTESIAN_POINT('Origin',(402.110089424886,-19.47200726879,484.583026572868));
#58238=CARTESIAN_POINT('',(378.226002309256,-19.47200726879,497.278268477331));
#58239=CARTESIAN_POINT('Origin',(348.162615483842,-19.47200726879,484.61086709224));
#58240=CARTESIAN_POINT('',(372.059793068845,-19.47200726879,497.281450655388));
#58241=CARTESIAN_POINT('',(372.059793068845,-19.47200726879,497.281450655388));
#58242=CARTESIAN_POINT('Origin',(348.162615483842,-19.47200726879,484.61086709224));
#58243=CARTESIAN_POINT('Origin',(375.115917770968,-19.47200726879,445.000000551893));
#58244=CARTESIAN_POINT('',(381.562332942994,-19.47200726879,491.429617785183));
#58245=CARTESIAN_POINT('',(381.562332942994,-19.47200726879,491.429617785183));
#58246=CARTESIAN_POINT('',(383.380181208862,-19.47200726879,491.140737160979));
#58247=CARTESIAN_POINT('Origin',(375.115917770968,-19.47200726879,445.000000551893));
#58248=CARTESIAN_POINT('',(383.380181208862,-19.47200726879,491.140737160979));
#58249=CARTESIAN_POINT('Origin',(407.969895877832,-19.47200726879,479.872875036399));
#58250=CARTESIAN_POINT('',(386.365834883846,-19.47200726879,496.14811183738));
#58251=CARTESIAN_POINT('Origin',(407.969895877832,-19.47200726879,479.872875036399));
#58252=CARTESIAN_POINT('',(386.365834883846,-19.47200726879,496.14811183738));
#58253=CARTESIAN_POINT('Origin',(354.690960078457,-19.47200726879,488.339617019018));
#58254=CARTESIAN_POINT('',(380.276039713744,-19.47200726879,497.115862481395));
#58255=CARTESIAN_POINT('',(380.276039713744,-19.47200726879,497.115862481395));
#58256=CARTESIAN_POINT('Origin',(354.690960078457,-19.47200726879,488.339617019018));
#58257=CARTESIAN_POINT('Origin',(375.115917770968,-19.47200726879,445.000000551893));
#58258=CARTESIAN_POINT('',(388.746159208926,-19.47200726879,489.849550642646));
#58259=CARTESIAN_POINT('',(388.746159208926,-19.47200726879,489.849550642646));
#58260=CARTESIAN_POINT('',(390.496435860187,-19.47200726879,489.2798524973));
#58261=CARTESIAN_POINT('Origin',(375.115917770968,-19.47200726879,445.000000551893));
#58262=CARTESIAN_POINT('',(390.496435860187,-19.47200726879,489.2798524973));
#58263=CARTESIAN_POINT('Origin',(413.020728353684,-19.47200726879,474.304037593687));
#58264=CARTESIAN_POINT('',(394.228657162783,-19.47200726879,493.758518946731));
#58265=CARTESIAN_POINT('Origin',(413.020728353684,-19.47200726879,474.304037593687));
#58266=CARTESIAN_POINT('',(394.228657162783,-19.47200726879,493.758518946731));
#58267=CARTESIAN_POINT('Origin',(361.72223491801,-19.47200726879,491.001201752435));
#58268=CARTESIAN_POINT('',(388.365227030949,-19.47200726879,495.667008824067));
#58269=CARTESIAN_POINT('',(388.365227030949,-19.47200726879,495.667008824067));
#58270=CARTESIAN_POINT('Origin',(361.72223491801,-19.47200726879,491.001201752435));
#58271=CARTESIAN_POINT('Origin',(375.115917770968,-19.47200726879,445.000000551893));
#58272=CARTESIAN_POINT('',(395.594363694478,-19.47200726879,487.165138729751));
#58273=CARTESIAN_POINT('',(395.594363694478,-19.47200726879,487.165138729751));
#58274=CARTESIAN_POINT('',(397.233971111143,-19.47200726879,486.328650922322));
#58275=CARTESIAN_POINT('Origin',(375.115917770968,-19.47200726879,445.000000551893));
#58276=CARTESIAN_POINT('',(397.233971111143,-19.47200726879,486.328650922322));
#58277=CARTESIAN_POINT('Origin',(417.138218594136,-19.47200726879,468.013637504482));
#58278=CARTESIAN_POINT('',(401.620860366348,-19.47200726879,490.168329512957));
#58279=CARTESIAN_POINT('Origin',(417.138218594136,-19.47200726879,468.013637504482));
#58280=CARTESIAN_POINT('',(401.620860366348,-19.47200726879,490.168329512957));
#58281=CARTESIAN_POINT('Origin',(369.083306680487,-19.47200726879,492.53008424306));
#58282=CARTESIAN_POINT('',(396.128172382238,-19.47200726879,492.970565268919));
#58283=CARTESIAN_POINT('',(396.128172382238,-19.47200726879,492.970565268919));
#58284=CARTESIAN_POINT('Origin',(369.083306680487,-19.47200726879,492.53008424306));
#58285=CARTESIAN_POINT('Origin',(375.115917770968,-19.47200726879,445.000000551893));
#58286=CARTESIAN_POINT('',(401.938320877327,-19.47200726879,483.442481176847));
#58287=CARTESIAN_POINT('',(401.938320877327,-19.47200726879,483.442481176847));
#58288=CARTESIAN_POINT('',(403.426886483253,-19.47200726879,482.359800813297));
#58289=CARTESIAN_POINT('Origin',(375.115917770968,-19.47200726879,445.000000551893));
#58290=CARTESIAN_POINT('',(403.426886483253,-19.47200726879,482.359800813297));
#58291=CARTESIAN_POINT('Origin',(420.220980324301,-19.47200726879,461.156565295623));
#58292=CARTESIAN_POINT('',(408.360423918353,-19.47200726879,485.465945915071));
#58293=CARTESIAN_POINT('Origin',(420.220980324301,-19.47200726879,461.156565295623));
#58294=CARTESIAN_POINT('',(408.360423918353,-19.47200726879,485.465945915071));
#58295=CARTESIAN_POINT('Origin',(376.5929213491,-19.47200726879,492.888618329905));
#58296=CARTESIAN_POINT('',(403.373726289321,-19.47200726879,489.092927205261));
#58297=CARTESIAN_POINT('',(403.373726289321,-19.47200726879,489.092927205261));
#58298=CARTESIAN_POINT('Origin',(376.5929213491,-19.47200726879,492.888618329905));
#58299=CARTESIAN_POINT('Origin',(375.115917770968,-19.47200726879,445.000000551893));
#58300=CARTESIAN_POINT('',(407.621821477246,-19.47200726879,478.773242167677));
#58301=CARTESIAN_POINT('',(407.621821477246,-19.47200726879,478.773242167677));
#58302=CARTESIAN_POINT('',(408.922691846948,-19.47200726879,477.471028431768));
#58303=CARTESIAN_POINT('Origin',(375.115917770968,-19.47200726879,445.000000551893));
#58304=CARTESIAN_POINT('',(408.922691846948,-19.47200726879,477.471028431768));
#58305=CARTESIAN_POINT('Origin',(422.193105719283,-19.47200726879,453.901664842209));
#58306=CARTESIAN_POINT('',(414.28139739682,-19.47200726879,479.767156443571));
#58307=CARTESIAN_POINT('Origin',(422.193105719283,-19.47200726879,453.901664842209));
#58308=CARTESIAN_POINT('',(414.28139739682,-19.47200726879,479.767156443571));
#58309=CARTESIAN_POINT('Origin',(384.066167287726,-19.47200726879,492.067975713845));
#58310=CARTESIAN_POINT('',(409.923479168393,-19.47200726879,484.129574951364));
#58311=CARTESIAN_POINT('',(409.923479168393,-19.47200726879,484.129574951364));
#58312=CARTESIAN_POINT('Origin',(384.066167287726,-19.47200726879,492.067975713845));
#58313=CARTESIAN_POINT('Origin',(375.115917770968,-19.47200726879,445.000000551893));
#58314=CARTESIAN_POINT('',(412.504918847007,-19.47200726879,473.272393862965));
#58315=CARTESIAN_POINT('',(412.504918847007,-19.47200726879,473.272393862965));
#58316=CARTESIAN_POINT('',(413.586062234642,-19.47200726879,471.782711578673));
#58317=CARTESIAN_POINT('Origin',(375.115917770968,-19.47200726879,445.000000551893));
#58318=CARTESIAN_POINT('',(413.586062234642,-19.47200726879,471.782711578673));
#58319=CARTESIAN_POINT('Origin',(423.006034506748,-19.4720072687901,446.427575871037));
#58320=CARTESIAN_POINT('',(419.237986784123,-19.47200726879,473.212284208443));
#58321=CARTESIAN_POINT('Origin',(423.006034506748,-19.4720072687901,446.427575871037));
#58322=CARTESIAN_POINT('',(419.237986784123,-19.47200726879,473.212284208443));
#58323=CARTESIAN_POINT('Origin',(391.319028379074,-19.47200726879,490.088363339644));
#58324=CARTESIAN_POINT('',(415.616154366188,-19.47200726879,478.202722712139));
#58325=CARTESIAN_POINT('',(415.616154366188,-19.47200726879,478.202722712139));
#58326=CARTESIAN_POINT('Origin',(391.319028379074,-19.47200726879,490.088363339644));
#58327=CARTESIAN_POINT('Origin',(375.115917770968,-19.47200726879,445.000000551893));
#58328=CARTESIAN_POINT('',(416.467374923295,-19.47200726879,467.07538540424));
#58329=CARTESIAN_POINT('',(416.467374923295,-19.47200726879,467.07538540424));
#58330=CARTESIAN_POINT('',(417.302169990551,-19.47200726879,465.434915493377));
#58331=CARTESIAN_POINT('Origin',(375.115917770968,-19.47200726879,445.000000551893));
#58332=CARTESIAN_POINT('',(417.302169990551,-19.47200726879,465.434915493377));
#58333=CARTESIAN_POINT('Origin',(422.639749681993,-19.4720072687901,438.918335257657));
#58334=CARTESIAN_POINT('',(423.108144399571,-19.47200726879,465.962731918489));
#58335=CARTESIAN_POINT('Origin',(422.639749681993,-19.4720072687901,438.918335257657));
#58336=CARTESIAN_POINT('',(423.108144399571,-19.47200726879,465.962731918489));
#58337=CARTESIAN_POINT('Origin',(398.17291511221,-19.47200726879,486.998525833912));
#58338=CARTESIAN_POINT('',(420.311579326428,-19.47200726879,471.458309259812));
#58339=CARTESIAN_POINT('',(420.311579326428,-19.47200726879,471.458309259812));
#58340=CARTESIAN_POINT('Origin',(398.17291511221,-19.47200726879,486.998525833912));
#58341=CARTESIAN_POINT('Origin',(375.115917770968,-19.47200726879,445.000000551893));
#58342=CARTESIAN_POINT('',(419.411620886875,-19.47200726879,460.334807706448));
#58343=CARTESIAN_POINT('',(419.411620886875,-19.47200726879,460.334807706448));
#58344=CARTESIAN_POINT('',(419.97951220867,-19.47200726879,458.583943982627));
#58345=CARTESIAN_POINT('Origin',(375.115917770968,-19.47200726879,445.000000551893));
#58346=CARTESIAN_POINT('',(419.97951220867,-19.47200726879,458.583943982627));
#58347=CARTESIAN_POINT('Origin',(421.103270393033,-19.4720072687901,431.558845427711));
#58348=CARTESIAN_POINT('',(425.796574118354,-19.47200726879,458.197007610973));
#58349=CARTESIAN_POINT('Origin',(421.103270393033,-19.4720072687901,431.558845427711));
#58350=CARTESIAN_POINT('',(425.796574118354,-19.47200726879,458.197007610973));
#58351=CARTESIAN_POINT('Origin',(404.459062049017,-19.47200726879,482.874545250622));
#58352=CARTESIAN_POINT('',(423.894137103373,-19.47200726879,464.062404437003));
#58353=CARTESIAN_POINT('',(423.894137103373,-19.47200726879,464.062404437003));
#58354=CARTESIAN_POINT('Origin',(404.459062049017,-19.47200726879,482.874545250622));
#58355=CARTESIAN_POINT('Origin',(375.115917770968,-19.47200726879,445.000000551893));
#58356=CARTESIAN_POINT('',(421.265159630731,-19.4720072687901,453.216636163204));
#58357=CARTESIAN_POINT('',(421.265159630731,-19.4720072687901,453.216636163204));
#58358=CARTESIAN_POINT('',(421.552163837999,-19.4720072687901,451.39849070209));
#58359=CARTESIAN_POINT('Origin',(375.115917770968,-19.47200726879,445.000000551893));
#58360=CARTESIAN_POINT('',(421.552163837999,-19.4720072687901,451.39849070209));
#58361=CARTESIAN_POINT('Origin',(418.434429859244,-19.4720072687901,424.530321445559));
#58362=CARTESIAN_POINT('',(427.23707787841,-19.4720072687901,450.106329191307));
#58363=CARTESIAN_POINT('Origin',(418.434429859244,-19.4720072687901,424.530321445559));
#58364=CARTESIAN_POINT('',(427.23707787841,-19.4720072687901,450.106329191307));
#58365=CARTESIAN_POINT('Origin',(410.022683389386,-19.47200726879,477.817967678442));
#58366=CARTESIAN_POINT('',(426.275613234725,-19.4720072687901,456.197119966052));
#58367=CARTESIAN_POINT('',(426.275613234725,-19.4720072687901,456.197119966052));
#58368=CARTESIAN_POINT('Origin',(410.022683389386,-19.47200726879,477.817967678442));
#58369=CARTESIAN_POINT('Origin',(375.115917770968,-19.47200726879,445.000000551893));
#58370=CARTESIAN_POINT('',(421.982350879447,-19.4720072687901,445.896143781759));
#58371=CARTESIAN_POINT('',(421.982350879447,-19.4720072687901,445.896143781759));
#58372=CARTESIAN_POINT('',(421.981400976092,-19.4720072687901,444.055485358683));
#58373=CARTESIAN_POINT('Origin',(375.115917770968,-19.47200726879,445.000000551893));
#58374=CARTESIAN_POINT('',(421.981400976092,-19.4720072687901,444.055485358683));
#58375=CARTESIAN_POINT('Origin',(414.698943791944,-19.4720072687901,418.005828897974));
#58376=CARTESIAN_POINT('',(427.394185696407,-19.4720072687901,441.889916013605));
#58377=CARTESIAN_POINT('Origin',(414.698943791944,-19.4720072687901,418.005828897974));
#58378=CARTESIAN_POINT('',(427.394185696407,-19.4720072687901,441.889916013605));
#58379=CARTESIAN_POINT('Origin',(414.726784311316,-19.47200726879,471.953302839018));
#58380=CARTESIAN_POINT('',(427.397367874464,-19.4720072687901,448.056125254016));
#58381=CARTESIAN_POINT('',(427.397367874464,-19.4720072687901,448.056125254016));
#58382=CARTESIAN_POINT('Origin',(414.726784311316,-19.47200726879,471.953302839018));
#58383=CARTESIAN_POINT('Origin',(375.115917770968,-19.47200726879,445.000000551893));
#58384=CARTESIAN_POINT('',(421.545535004259,-19.4720072687901,438.553585379867));
#58385=CARTESIAN_POINT('',(421.545535004259,-19.4720072687901,438.553585379867));
#58386=CARTESIAN_POINT('',(421.256654380055,-19.4720072687901,436.735737113998));
#58387=CARTESIAN_POINT('Origin',(375.115917770968,-19.47200726879,445.000000551893));
#58388=CARTESIAN_POINT('',(421.256654380055,-19.4720072687901,436.735737113998));
#58389=CARTESIAN_POINT('Origin',(409.988792255475,-19.4720072687901,412.146022445029));
#58390=CARTESIAN_POINT('',(426.264029056456,-19.4720072687901,433.750083439015));
#58391=CARTESIAN_POINT('Origin',(409.988792255475,-19.4720072687901,412.146022445029));
#58392=CARTESIAN_POINT('',(426.264029056456,-19.4720072687901,433.750083439015));
#58393=CARTESIAN_POINT('Origin',(418.455534238094,-19.47200726879,465.424958244404));
#58394=CARTESIAN_POINT('',(427.23177970047,-19.4720072687901,439.839878609116));
#58395=CARTESIAN_POINT('',(427.23177970047,-19.4720072687901,439.839878609116));
#58396=CARTESIAN_POINT('Origin',(418.455534238094,-19.47200726879,465.424958244404));
#58397=CARTESIAN_POINT('Origin',(375.115917770968,-19.47200726879,445.000000551893));
#58398=CARTESIAN_POINT('',(419.965467861721,-19.4720072687901,431.369759113934));
#58399=CARTESIAN_POINT('',(419.965467861721,-19.4720072687901,431.369759113934));
#58400=CARTESIAN_POINT('',(419.395769716375,-19.4720072687901,429.619482462673));
#58401=CARTESIAN_POINT('Origin',(375.115917770968,-19.47200726879,445.000000551893));
#58402=CARTESIAN_POINT('',(419.395769716375,-19.4720072687901,429.619482462673));
#58403=CARTESIAN_POINT('Origin',(404.419954812762,-19.4720072687901,407.095189969177));
#58404=CARTESIAN_POINT('',(423.874436165807,-19.4720072687901,425.887261160078));
#58405=CARTESIAN_POINT('Origin',(404.419954812762,-19.4720072687901,407.095189969177));
#58406=CARTESIAN_POINT('',(423.874436165807,-19.4720072687901,425.887261160078));
#58407=CARTESIAN_POINT('Origin',(421.117118971511,-19.47200726879,458.393683404851));
#58408=CARTESIAN_POINT('',(425.782926043143,-19.4720072687901,431.750691291911));
#58409=CARTESIAN_POINT('',(425.782926043143,-19.4720072687901,431.750691291911));
#58410=CARTESIAN_POINT('Origin',(421.117118971511,-19.47200726879,458.393683404851));
#58411=CARTESIAN_POINT('Origin',(375.115917770968,-19.47200726879,445.000000551893));
#58412=CARTESIAN_POINT('',(417.281055948826,-19.4720072687901,424.521554628383));
#58413=CARTESIAN_POINT('',(417.281055948826,-19.4720072687901,424.521554628383));
#58414=CARTESIAN_POINT('',(416.444568141397,-19.4720072687901,422.881947211718));
#58415=CARTESIAN_POINT('Origin',(375.115917770968,-19.47200726879,445.000000551893));
#58416=CARTESIAN_POINT('',(416.444568141397,-19.4720072687901,422.881947211718));
#58417=CARTESIAN_POINT('Origin',(398.129554723558,-19.4720072687901,402.977699728725));
#58418=CARTESIAN_POINT('',(420.284246732032,-19.4720072687901,418.495057956513));
#58419=CARTESIAN_POINT('Origin',(398.129554723558,-19.4720072687901,402.977699728725));
#58420=CARTESIAN_POINT('',(420.284246732032,-19.4720072687901,418.495057956513));
#58421=CARTESIAN_POINT('Origin',(422.646001462136,-19.4720072687901,451.032611642374));
#58422=CARTESIAN_POINT('',(423.086482487995,-19.4720072687901,423.987745940623));
#58423=CARTESIAN_POINT('',(423.086482487995,-19.4720072687901,423.987745940623));
#58424=CARTESIAN_POINT('Origin',(422.646001462136,-19.4720072687901,451.032611642374));
#58425=CARTESIAN_POINT('Origin',(375.115917770968,-19.47200726879,445.000000551893));
#58426=CARTESIAN_POINT('',(413.558398395922,-19.4720072687901,418.177597445533));
#58427=CARTESIAN_POINT('',(413.558398395922,-19.4720072687901,418.177597445533));
#58428=CARTESIAN_POINT('',(412.475718032372,-19.4720072687901,416.689031839608));
#58429=CARTESIAN_POINT('Origin',(375.115917770968,-19.47200726879,445.000000551893));
#58430=CARTESIAN_POINT('',(412.475718032372,-19.4720072687901,416.689031839608));
#58431=CARTESIAN_POINT('Origin',(391.272482514698,-19.4720072687901,399.89493799856));
#58432=CARTESIAN_POINT('',(415.581863134147,-19.4720072687901,411.755494404508));
#58433=CARTESIAN_POINT('Origin',(391.272482514698,-19.4720072687901,399.89493799856));
#58434=CARTESIAN_POINT('',(415.581863134147,-19.4720072687901,411.755494404508));
#58435=CARTESIAN_POINT('Origin',(423.004535548981,-19.4720072687901,443.522996973761));
#58436=CARTESIAN_POINT('',(419.208844424337,-19.4720072687901,416.742192033539));
#58437=CARTESIAN_POINT('',(419.208844424337,-19.4720072687901,416.742192033539));
#58438=CARTESIAN_POINT('Origin',(423.004535548981,-19.4720072687901,443.522996973761));
#58439=CARTESIAN_POINT('Origin',(375.115917770968,-19.47200726879,445.000000551893));
#58440=CARTESIAN_POINT('',(408.889159386753,-19.4720072687901,412.494096845614));
#58441=CARTESIAN_POINT('',(408.889159386753,-19.4720072687901,412.494096845614));
#58442=CARTESIAN_POINT('',(407.586945650843,-19.4720072687901,411.193226475912));
#58443=CARTESIAN_POINT('Origin',(375.115917770968,-19.47200726879,445.000000551893));
#58444=CARTESIAN_POINT('',(407.586945650843,-19.4720072687901,411.193226475912));
#58445=CARTESIAN_POINT('Origin',(384.017582061284,-19.4720072687901,397.922812603578));
#58446=CARTESIAN_POINT('',(409.883073662646,-19.4720072687901,405.834520926041));
#58447=CARTESIAN_POINT('Origin',(384.017582061284,-19.4720072687901,397.922812603578));
#58448=CARTESIAN_POINT('',(409.883073662646,-19.4720072687901,405.834520926041));
#58449=CARTESIAN_POINT('Origin',(422.183892932921,-19.4720072687901,436.049751035135));
#58450=CARTESIAN_POINT('',(414.245492170439,-19.4720072687901,410.192439154467));
#58451=CARTESIAN_POINT('',(414.245492170439,-19.4720072687901,410.192439154467));
#58452=CARTESIAN_POINT('Origin',(422.183892932921,-19.4720072687901,436.049751035135));
#58453=CARTESIAN_POINT('Origin',(375.115917770968,-19.47200726879,445.000000551893));
#58454=CARTESIAN_POINT('',(403.38831108204,-19.4720072687901,407.610999475854));
#58455=CARTESIAN_POINT('',(403.38831108204,-19.4720072687901,407.610999475854));
#58456=CARTESIAN_POINT('',(401.898628797749,-19.4720072687901,406.529856088218));
#58457=CARTESIAN_POINT('Origin',(375.115917770968,-19.47200726879,445.000000551893));
#58458=CARTESIAN_POINT('',(401.898628797749,-19.4720072687901,406.529856088218));
#58459=CARTESIAN_POINT('Origin',(376.543493090113,-19.4720072687901,397.109883816113));
#58460=CARTESIAN_POINT('',(403.328201427518,-19.4720072687901,400.877931538737));
#58461=CARTESIAN_POINT('Origin',(376.543493090113,-19.4720072687901,397.109883816113));
#58462=CARTESIAN_POINT('',(403.328201427518,-19.4720072687901,400.877931538737));
#58463=CARTESIAN_POINT('Origin',(420.20428055872,-19.4720072687901,428.796889943787));
#58464=CARTESIAN_POINT('',(408.318639931214,-19.4720072687901,404.499763956673));
#58465=CARTESIAN_POINT('',(408.318639931214,-19.4720072687901,404.499763956673));
#58466=CARTESIAN_POINT('Origin',(420.20428055872,-19.4720072687901,428.796889943787));
#58467=CARTESIAN_POINT('Origin',(375.115917770968,-19.47200726879,445.000000551893));
#58468=CARTESIAN_POINT('',(397.191302623315,-19.4720072687901,403.648543399565));
#58469=CARTESIAN_POINT('',(397.191302623315,-19.4720072687901,403.648543399565));
#58470=CARTESIAN_POINT('',(395.550832712453,-19.4720072687901,402.813748332309));
#58471=CARTESIAN_POINT('Origin',(375.115917770968,-19.47200726879,445.000000551893));
#58472=CARTESIAN_POINT('',(395.550832712453,-19.4720072687901,402.813748332309));
#58473=CARTESIAN_POINT('Origin',(369.034252476732,-19.4720072687901,397.476168640868));
#58474=CARTESIAN_POINT('',(396.078649137564,-19.4720072687901,397.00777392329));
#58475=CARTESIAN_POINT('Origin',(369.034252476732,-19.4720072687901,397.476168640868));
#58476=CARTESIAN_POINT('',(396.078649137564,-19.4720072687901,397.00777392329));
#58477=CARTESIAN_POINT('Origin',(417.114443052987,-19.4720072687901,421.943003210651));
#58478=CARTESIAN_POINT('',(401.574226478887,-19.4720072687901,399.804338996432));
#58479=CARTESIAN_POINT('',(401.574226478887,-19.4720072687901,399.804338996432));
#58480=CARTESIAN_POINT('Origin',(417.114443052987,-19.4720072687901,421.943003210651));
#58481=CARTESIAN_POINT('Origin',(375.115917770968,-19.47200726879,445.000000551893));
#58482=CARTESIAN_POINT('',(390.450724925524,-19.4720072687901,400.704297435985));
#58483=CARTESIAN_POINT('',(390.450724925524,-19.4720072687901,400.704297435985));
#58484=CARTESIAN_POINT('',(388.699861201703,-19.4720072687901,400.136406114191));
#58485=CARTESIAN_POINT('Origin',(375.115917770968,-19.47200726879,445.000000551893));
#58486=CARTESIAN_POINT('',(388.699861201703,-19.4720072687901,400.136406114191));
#58487=CARTESIAN_POINT('Origin',(361.674762646786,-19.4720072687901,399.012647929828));
#58488=CARTESIAN_POINT('',(388.312924830048,-19.4720072687901,394.319344204506));
#58489=CARTESIAN_POINT('Origin',(361.674762646786,-19.4720072687901,399.012647929828));
#58490=CARTESIAN_POINT('',(388.312924830048,-19.4720072687901,394.319344204506));
#58491=CARTESIAN_POINT('Origin',(412.990462469698,-19.4720072687901,415.656856273844));
#58492=CARTESIAN_POINT('',(394.178321656079,-19.4720072687901,396.221781219488));
#58493=CARTESIAN_POINT('',(394.178321656079,-19.4720072687901,396.221781219488));
#58494=CARTESIAN_POINT('Origin',(412.990462469698,-19.4720072687901,415.656856273844));
#58495=CARTESIAN_POINT('Origin',(375.115917770968,-19.47200726879,445.000000551893));
#58496=CARTESIAN_POINT('',(383.33255338228,-19.4720072687901,398.850758692129));
#58497=CARTESIAN_POINT('',(383.33255338228,-19.4720072687901,398.850758692129));
#58498=CARTESIAN_POINT('',(381.514407921165,-19.4720072687901,398.563754484862));
#58499=CARTESIAN_POINT('Origin',(375.115917770968,-19.47200726879,445.000000551893));
#58500=CARTESIAN_POINT('',(381.514407921165,-19.4720072687901,398.563754484862));
#58501=CARTESIAN_POINT('Origin',(354.646238664634,-19.4720072687901,401.681488463616));
#58502=CARTESIAN_POINT('',(380.222246410382,-19.4720072687901,392.878840444451));
#58503=CARTESIAN_POINT('Origin',(354.646238664634,-19.4720072687901,401.681488463616));
#58504=CARTESIAN_POINT('',(380.222246410382,-19.4720072687901,392.878840444451));
#58505=CARTESIAN_POINT('Origin',(407.933884897518,-19.4720072687901,410.093234933475));
#58506=CARTESIAN_POINT('',(386.313037185128,-19.4720072687901,393.840305088136));
#58507=CARTESIAN_POINT('',(386.313037185128,-19.4720072687901,393.840305088136));
#58508=CARTESIAN_POINT('Origin',(407.933884897518,-19.4720072687901,410.093234933475));
#58509=CARTESIAN_POINT('Origin',(375.115917770968,-19.47200726879,445.000000551893));
#58510=CARTESIAN_POINT('',(378.172042473091,-19.4720072687901,392.718550448397));
#58511=CARTESIAN_POINT('Origin',(375.115917770968,-19.47200726879,445.000000551893));
#58512=CARTESIAN_POINT('',(378.172042473091,-19.4720072687901,392.718550448397));
#58513=CARTESIAN_POINT('Origin',(375.115917770968,-19.47200726879,445.000000551893));
#58514=CARTESIAN_POINT('Origin',(375.115917770968,-19.47200726879,445.000000551893));
#58515=CARTESIAN_POINT('Origin',(375.115917770968,-19.47200726879,445.000000551893));
#58516=CARTESIAN_POINT('Origin',(375.115917770968,-19.47200726879,445.000000551893));
#58517=CARTESIAN_POINT('Origin',(375.115917770968,-19.47200726879,445.000000551893));
#58518=CARTESIAN_POINT('Origin',(375.115917770968,-19.47200726879,445.000000551893));
#58519=CARTESIAN_POINT('Origin',(375.115917770968,-19.47200726879,445.000000551893));
#58520=CARTESIAN_POINT('Origin',(375.115917770968,-19.47200726879,445.000000551893));
#58521=CARTESIAN_POINT('Origin',(375.115917770968,-19.47200726879,445.000000551893));
#58522=CARTESIAN_POINT('Origin',(375.115917770968,-19.47200726879,445.000000551893));
#58523=CARTESIAN_POINT('Origin',(375.115917770968,-19.47200726879,445.000000551893));
#58524=CARTESIAN_POINT('Origin',(375.115917770968,-19.47200726879,445.000000551893));
#58525=CARTESIAN_POINT('Origin',(375.115917770968,-19.47200726879,445.000000551893));
#58526=CARTESIAN_POINT('Origin',(375.115917770968,-19.47200726879,445.000000551893));
#58527=CARTESIAN_POINT('Origin',(375.115917770968,-19.47200726879,445.000000551893));
#58528=CARTESIAN_POINT('Origin',(375.115917770968,-19.47200726879,445.000000551893));
#58529=CARTESIAN_POINT('Origin',(375.115917770968,-19.47200726879,445.000000551893));
#58530=CARTESIAN_POINT('Origin',(375.115917770968,-19.47200726879,445.000000551893));
#58531=CARTESIAN_POINT('Origin',(375.115917770968,-19.47200726879,445.000000551893));
#58532=CARTESIAN_POINT('Origin',(375.115917770968,-19.47200726879,445.000000551893));
#58533=CARTESIAN_POINT('Origin',(375.115917770968,-19.47200726879,445.000000551893));
#58534=CARTESIAN_POINT('Origin',(375.115917770968,-19.47200726879,445.000000551893));
#58535=CARTESIAN_POINT('Origin',(375.115917770968,-19.47200726879,445.000000551893));
#58536=CARTESIAN_POINT('Origin',(375.115917770968,-19.47200726879,445.000000551893));
#58537=CARTESIAN_POINT('Origin',(375.115917770968,-19.47200726879,445.000000551893));
#58538=CARTESIAN_POINT('Origin',(375.115917770968,-19.47200726879,445.000000551893));
#58539=CARTESIAN_POINT('Origin',(375.115917770968,-19.47200726879,445.000000551893));
#58540=CARTESIAN_POINT('Origin',(375.115917770968,-19.47200726879,445.000000551893));
#58541=CARTESIAN_POINT('Origin',(375.115917770968,-19.47200726879,445.000000551893));
#58542=CARTESIAN_POINT('Origin',(375.115917770968,-19.47200726879,445.000000551893));
#58543=CARTESIAN_POINT('Origin',(375.115917770968,-19.47200726879,445.000000551893));
#58544=CARTESIAN_POINT('Origin',(375.115917770968,-19.47200726879,445.000000551893));
#58545=CARTESIAN_POINT('Origin',(375.115917770968,-19.47200726879,445.000000551893));
#58546=CARTESIAN_POINT('Origin',(375.115917770968,-19.47200726879,445.000000551893));
#58547=CARTESIAN_POINT('Origin',(375.115917770968,-19.47200726879,445.000000551893));
#58548=CARTESIAN_POINT('Origin',(375.115917770968,-19.47200726879,445.000000551893));
#58549=CARTESIAN_POINT('Origin',(375.115917770968,-19.47200726879,445.000000551893));
#58550=CARTESIAN_POINT('Origin',(375.115917770968,-19.47200726879,445.000000551893));
#58551=CARTESIAN_POINT('Origin',(375.115917770968,-19.47200726879,445.000000551893));
#58552=CARTESIAN_POINT('Origin',(375.115917770968,-19.47200726879,445.000000551893));
#58553=CARTESIAN_POINT('Origin',(375.115917770968,-19.47200726879,445.000000551893));
#58554=CARTESIAN_POINT('Origin',(375.115917770968,-19.47200726879,445.000000551893));
#58555=CARTESIAN_POINT('Origin',(375.115917770968,-19.47200726879,445.000000551893));
#58556=CARTESIAN_POINT('Origin',(375.115917770968,-19.47200726879,445.000000551893));
#58557=CARTESIAN_POINT('Origin',(375.115917770968,-19.47200726879,445.000000551893));
#58558=CARTESIAN_POINT('Origin',(375.115917770968,-19.47200726879,445.000000551893));
#58559=CARTESIAN_POINT('Origin',(375.115917770968,-19.47200726879,445.000000551893));
#58560=CARTESIAN_POINT('Origin',(375.115917770968,-19.47200726879,445.000000551893));
#58561=CARTESIAN_POINT('Origin',(375.115917770968,-19.47200726879,445.000000551893));
#58562=CARTESIAN_POINT('Origin',(375.115917770968,-19.47200726879,445.000000551893));
#58563=CARTESIAN_POINT('Origin',(375.115917770968,-19.47200726879,445.000000551893));
#58564=CARTESIAN_POINT('Origin',(375.115917770968,-19.47200726879,445.000000551893));
#58565=CARTESIAN_POINT('Origin',(375.115917770968,-19.47200726879,445.000000551893));
#58566=CARTESIAN_POINT('Origin',(375.115917770968,-19.47200726879,445.000000551893));
#58567=CARTESIAN_POINT('Origin',(375.115917770968,-19.47200726879,445.000000551893));
#58568=CARTESIAN_POINT('Origin',(375.115917770968,-19.47200726879,445.000000551893));
#58569=CARTESIAN_POINT('Origin',(375.115917770968,-19.47200726879,445.000000551893));
#58570=CARTESIAN_POINT('Origin',(375.115917770968,-19.47200726879,445.000000551893));
#58571=CARTESIAN_POINT('Origin',(375.115917770968,-19.47200726879,445.000000551893));
#58572=CARTESIAN_POINT('Origin',(375.115917770968,-19.47200726879,445.000000551893));
#58573=CARTESIAN_POINT('Origin',(375.115917770968,-19.47200726879,445.000000551893));
#58574=CARTESIAN_POINT('Origin',(375.115917770968,-19.47200726879,445.000000551893));
#58575=CARTESIAN_POINT('Origin',(375.115917770968,-19.47200726879,445.000000551893));
#58576=CARTESIAN_POINT('Origin',(375.115917770968,-19.47200726879,445.000000551893));
#58577=CARTESIAN_POINT('Origin',(375.115917770968,-19.47200726879,445.000000551893));
#58578=CARTESIAN_POINT('Origin',(375.115917770968,-19.47200726879,445.000000551893));
#58579=CARTESIAN_POINT('Origin',(375.115917770968,-19.47200726879,445.000000551893));
#58580=CARTESIAN_POINT('Origin',(375.115917770968,-19.47200726879,445.000000551893));
#58581=CARTESIAN_POINT('Origin',(375.115917770968,-19.47200726879,445.000000551893));
#58582=CARTESIAN_POINT('Origin',(375.115917770968,-19.47200726879,445.000000551893));
#58583=CARTESIAN_POINT('Origin',(375.115917770968,-19.47200726879,445.000000551893));
#58584=CARTESIAN_POINT('Origin',(375.115917770968,-19.47200726879,445.000000551893));
#58585=CARTESIAN_POINT('Origin',(375.115917770968,-19.47200726879,445.000000551893));
#58586=CARTESIAN_POINT('Origin',(375.115917770968,-19.47200726879,445.000000551893));
#58587=CARTESIAN_POINT('Origin',(375.115917770968,-19.47200726879,445.000000551893));
#58588=CARTESIAN_POINT('Origin',(375.115917770968,-19.47200726879,445.000000551893));
#58589=CARTESIAN_POINT('Origin',(375.115917770968,-19.47200726879,445.000000551893));
#58590=CARTESIAN_POINT('',(376.012061000835,-19.4720072687901,398.133567443413));
#58591=CARTESIAN_POINT('',(376.012061000835,-19.4720072687901,398.133567443413));
#58592=CARTESIAN_POINT('',(374.171402577758,-19.4720072687901,398.134517346768));
#58593=CARTESIAN_POINT('Origin',(375.115917770968,-19.47200726879,445.000000551893));
#58594=CARTESIAN_POINT('',(374.171402577758,-19.4720072687901,398.134517346768));
#58595=CARTESIAN_POINT('Origin',(348.12174611705,-19.4720072687901,405.416974530917));
#58596=CARTESIAN_POINT('',(372.005833232681,-19.4720072687901,392.721732626454));
#58597=CARTESIAN_POINT('Origin',(348.12174611705,-19.4720072687901,405.416974530917));
#58598=CARTESIAN_POINT('',(372.005833232681,-19.4720072687901,392.721732626454));
#58599=CARTESIAN_POINT('Origin',(402.069220058094,-19.4720072687901,405.389134011545));
#58600=CARTESIAN_POINT('Origin',(402.069220058094,-19.4720072687901,405.389134011545));
#58601=CARTESIAN_POINT('Origin',(375.115917770968,-19.47200726879,445.000000551893));
#58602=CARTESIAN_POINT('Origin',(375.115917770968,-19.47200726879,445.000000551893));
#58603=CARTESIAN_POINT('Origin',(375.115917770968,-19.47200726879,445.000000551893));
#58604=CARTESIAN_POINT('',(0.,0.,0.));
#58605=CARTESIAN_POINT('',(0.,0.,0.));
#58606=CARTESIAN_POINT('',(0.,0.,0.));
#58607=CARTESIAN_POINT('',(0.,0.,0.));
#58608=CARTESIAN_POINT('Origin',(322.566620000606,298.539939847208,392.450702781549));
#58609=CARTESIAN_POINT('',(322.566620000606,298.546824263208,395.671178941549));
#58610=CARTESIAN_POINT('',(320.695173668754,298.546824263208,389.829795434059));
#58611=CARTESIAN_POINT('Origin',(322.566620000606,298.546824263208,392.450702781549));
#58612=CARTESIAN_POINT('Origin',(322.566620000606,298.546824263208,392.450702781549));
#58613=CARTESIAN_POINT('',(320.73517960089,298.477980103208,389.885822603897));
#58614=CARTESIAN_POINT('',(320.699174261967,298.539939847208,389.835398151043));
#58615=CARTESIAN_POINT('Origin',(322.566620000606,298.477980103208,392.450702781549));
#58616=CARTESIAN_POINT('Origin',(325.736133600606,298.477980103208,392.450702781549));
#58617=CARTESIAN_POINT('Origin',(322.566620000606,291.082459603103,392.450702781549));
#58618=CARTESIAN_POINT('',(322.566620000606,290.896525325314,392.450702781549));
#58619=CARTESIAN_POINT('',(320.695173668754,292.755868103209,389.829795434059));
#58620=CARTESIAN_POINT('',(322.379475367421,291.082459603103,392.1886120468));
#58621=CARTESIAN_POINT('',(322.566620000606,292.755868103209,395.671178941549));
#58622=CARTESIAN_POINT('Origin',(322.566620000606,292.755868103209,392.450702781549));
#58623=CARTESIAN_POINT('Origin',(322.566620000606,292.755868103209,392.450702781549));
#58624=CARTESIAN_POINT('Origin',(322.566620000606,295.651346183209,392.450702781549));
#58625=CARTESIAN_POINT('',(322.566620000606,295.651346183209,395.671178941549));
#58626=CARTESIAN_POINT('Origin',(322.566620000605,317.432476103209,392.450702781549));
#58627=CARTESIAN_POINT('',(322.566620000604,320.829980103208,396.362302781548));
#58628=CARTESIAN_POINT('Origin',(322.566620000604,320.829980103208,392.450702781549));
#58629=CARTESIAN_POINT('',(322.566620000605,314.034972103209,396.362302781549));
#58630=CARTESIAN_POINT('',(322.566620000605,317.432476103209,396.362302781548));
#58631=CARTESIAN_POINT('Origin',(322.566620000605,314.034972103209,392.450702781549));
#58632=CARTESIAN_POINT('Origin',(326.775501600604,320.829980103209,392.450702781549));
#58633=CARTESIAN_POINT('',(322.566620000604,320.829980103208,388.259702781549));
#58634=CARTESIAN_POINT('Origin',(322.566620000604,320.829980103208,392.450702781549));
#58635=CARTESIAN_POINT('Origin',(326.775501600605,314.034972103209,392.450702781549));
#58636=CARTESIAN_POINT('',(322.566620000605,314.034972103209,388.259702781549));
#58637=CARTESIAN_POINT('Origin',(322.566620000605,314.034972103209,392.450702781549));
#58638=CARTESIAN_POINT('Origin',(322.566620000605,317.432476103209,392.450702781549));
#58639=CARTESIAN_POINT('',(322.566620000605,317.432476103209,388.259702781549));
#58640=CARTESIAN_POINT('Origin',(427.66521554129,298.539939847217,497.549298322233));
#58641=CARTESIAN_POINT('',(427.66521554129,298.546824263216,500.769774482233));
#58642=CARTESIAN_POINT('',(425.793769209438,298.546824263216,494.928390974743));
#58643=CARTESIAN_POINT('Origin',(427.66521554129,298.546824263216,497.549298322233));
#58644=CARTESIAN_POINT('Origin',(427.66521554129,298.546824263216,497.549298322233));
#58645=CARTESIAN_POINT('',(425.833775141574,298.477980103216,494.984418144581));
#58646=CARTESIAN_POINT('',(425.797769802652,298.539939847217,494.933993691727));
#58647=CARTESIAN_POINT('Origin',(427.66521554129,298.477980103217,497.549298322233));
#58648=CARTESIAN_POINT('Origin',(430.83472914129,298.477980103217,497.549298322233));
#58649=CARTESIAN_POINT('Origin',(427.665215541291,291.082459603111,497.549298322233));
#58650=CARTESIAN_POINT('',(427.665215541291,290.896525325322,497.549298322233));
#58651=CARTESIAN_POINT('',(425.793769209439,292.755868103217,494.928390974743));
#58652=CARTESIAN_POINT('',(427.478070908106,291.082459603111,497.287207587484));
#58653=CARTESIAN_POINT('',(427.665215541291,292.755868103217,500.769774482233));
#58654=CARTESIAN_POINT('Origin',(427.665215541291,292.755868103217,497.549298322233));
#58655=CARTESIAN_POINT('Origin',(427.665215541291,292.755868103217,497.549298322233));
#58656=CARTESIAN_POINT('Origin',(427.66521554129,295.651346183217,497.549298322233));
#58657=CARTESIAN_POINT('',(427.66521554129,295.651346183217,500.769774482233));
#58658=CARTESIAN_POINT('Origin',(427.665215541289,317.432476103217,497.549298322232));
#58659=CARTESIAN_POINT('',(427.665215541289,320.829980103216,501.460898322232));
#58660=CARTESIAN_POINT('Origin',(427.665215541289,320.829980103217,497.549298322232));
#58661=CARTESIAN_POINT('',(427.665215541289,314.034972103217,501.460898322232));
#58662=CARTESIAN_POINT('',(427.665215541289,317.432476103217,501.460898322232));
#58663=CARTESIAN_POINT('Origin',(427.665215541289,314.034972103217,497.549298322232));
#58664=CARTESIAN_POINT('Origin',(431.874097141289,320.829980103217,497.549298322232));
#58665=CARTESIAN_POINT('',(427.665215541289,320.829980103216,493.358298322232));
#58666=CARTESIAN_POINT('Origin',(427.665215541289,320.829980103216,497.549298322232));
#58667=CARTESIAN_POINT('Origin',(431.874097141289,314.034972103217,497.549298322232));
#58668=CARTESIAN_POINT('',(427.665215541289,314.034972103217,493.358298322232));
#58669=CARTESIAN_POINT('Origin',(427.665215541289,314.034972103217,497.549298322232));
#58670=CARTESIAN_POINT('Origin',(427.665215541289,317.432476103217,497.549298322232));
#58671=CARTESIAN_POINT('',(427.665215541289,317.432476103217,493.358298322232));
#58672=CARTESIAN_POINT('Origin',(319.69547489095,274.10535930321,526.415998247891));
#58673=CARTESIAN_POINT('',(321.292075273455,271.869365888763,526.422077991891));
#58674=CARTESIAN_POINT('',(319.69547489095,271.35785146321,526.422077991891));
#58675=CARTESIAN_POINT('Origin',(319.69547489095,274.10535930321,526.422077991891));
#58676=CARTESIAN_POINT('',(321.256745359361,271.918844428361,526.361280551891));
#58677=CARTESIAN_POINT('',(321.288542282045,271.874313742723,526.415998247891));
#58678=CARTESIAN_POINT('Origin',(319.69547489095,274.10535930321,526.361280551891));
#58679=CARTESIAN_POINT('Origin',(319.69547489095,274.10535930321,526.422077991891));
#58680=CARTESIAN_POINT('Origin',(316.99088289095,274.105359303209,526.361280551891));
#58681=CARTESIAN_POINT('Origin',(319.69547489095,274.10535930321,523.709439271891));
#58682=CARTESIAN_POINT('',(319.69547489095,271.35785146321,520.996800551891));
#58683=CARTESIAN_POINT('',(318.098874508445,276.341352717656,520.996800551891));
#58684=CARTESIAN_POINT('Origin',(319.69547489095,274.10535930321,520.996800551891));
#58685=CARTESIAN_POINT('Origin',(319.69547489095,274.10535930321,520.996800551891));
#58686=CARTESIAN_POINT('',(319.69547489095,271.35785146321,523.709439271891));
#58687=CARTESIAN_POINT('Origin',(319.69547489095,274.10535930321,519.569153599969));
#58688=CARTESIAN_POINT('',(319.69547489095,274.10535930321,519.410526160866));
#58689=CARTESIAN_POINT('',(319.535814852699,274.328958644654,519.569153599969));
#58690=CARTESIAN_POINT('Origin',(319.69547489095,274.10535930321,543.795840551891));
#58691=CARTESIAN_POINT('',(319.69547489095,277.45815930321,548.713280551891));
#58692=CARTESIAN_POINT('Origin',(319.69547489095,274.10535930321,548.713280551891));
#58693=CARTESIAN_POINT('',(319.69547489095,277.45815930321,538.878400551891));
#58694=CARTESIAN_POINT('',(319.69547489095,277.45815930321,543.795840551891));
#58695=CARTESIAN_POINT('Origin',(319.69547489095,274.10535930321,538.878400551891));
#58696=CARTESIAN_POINT('Origin',(316.04539329095,274.10535930321,548.713280551891));
#58697=CARTESIAN_POINT('',(319.69547489095,270.47315930321,548.713280551891));
#58698=CARTESIAN_POINT('Origin',(319.69547489095,274.10535930321,548.713280551891));
#58699=CARTESIAN_POINT('Origin',(319.69547489095,274.10535930321,543.795840551891));
#58700=CARTESIAN_POINT('',(319.69547489095,270.47315930321,538.878400551891));
#58701=CARTESIAN_POINT('Origin',(319.69547489095,274.10535930321,538.878400551891));
#58702=CARTESIAN_POINT('',(319.69547489095,270.47315930321,543.795840551891));
#58703=CARTESIAN_POINT('Origin',(323.34555649095,274.10535930321,538.878400551891));
#58704=CARTESIAN_POINT('Origin',(427.665215541289,317.432476103216,392.450702781548));
#58705=CARTESIAN_POINT('',(427.665215541289,320.829980103215,396.362302781548));
#58706=CARTESIAN_POINT('Origin',(427.665215541289,320.829980103215,392.450702781548));
#58707=CARTESIAN_POINT('',(427.665215541289,314.034972103216,396.362302781548));
#58708=CARTESIAN_POINT('',(427.665215541289,317.432476103216,396.362302781548));
#58709=CARTESIAN_POINT('Origin',(427.665215541289,314.034972103216,392.450702781548));
#58710=CARTESIAN_POINT('Origin',(431.874097141288,320.829980103216,392.450702781548));
#58711=CARTESIAN_POINT('',(427.665215541288,320.829980103216,388.259702781548));
#58712=CARTESIAN_POINT('Origin',(427.665215541288,320.829980103216,392.450702781548));
#58713=CARTESIAN_POINT('Origin',(427.665215541289,317.432476103216,392.450702781548));
#58714=CARTESIAN_POINT('',(427.665215541289,314.034972103216,388.259702781548));
#58715=CARTESIAN_POINT('',(427.665215541289,317.432476103216,388.259702781548));
#58716=CARTESIAN_POINT('Origin',(427.665215541289,314.034972103216,392.450702781548));
#58717=CARTESIAN_POINT('Origin',(431.874097141289,314.034972103216,392.450702781548));
#58718=CARTESIAN_POINT('Origin',(427.66521554129,298.539939847216,392.450702781548));
#58719=CARTESIAN_POINT('',(427.66521554129,298.546824263215,395.671178941548));
#58720=CARTESIAN_POINT('',(425.793769209438,298.546824263215,389.829795434059));
#58721=CARTESIAN_POINT('Origin',(427.66521554129,298.546824263215,392.450702781548));
#58722=CARTESIAN_POINT('Origin',(427.66521554129,298.546824263215,392.450702781548));
#58723=CARTESIAN_POINT('',(425.833775141574,298.477980103215,389.885822603897));
#58724=CARTESIAN_POINT('',(425.797769802652,298.539939847215,389.835398151042));
#58725=CARTESIAN_POINT('Origin',(427.66521554129,298.477980103215,392.450702781548));
#58726=CARTESIAN_POINT('Origin',(430.83472914129,298.477980103216,392.450702781548));
#58727=CARTESIAN_POINT('Origin',(427.66521554129,295.651346183216,392.450702781548));
#58728=CARTESIAN_POINT('',(427.66521554129,292.755868103216,395.671178941548));
#58729=CARTESIAN_POINT('',(425.793769209438,292.755868103216,389.829795434059));
#58730=CARTESIAN_POINT('Origin',(427.66521554129,292.755868103216,392.450702781548));
#58731=CARTESIAN_POINT('Origin',(427.66521554129,292.755868103216,392.450702781548));
#58732=CARTESIAN_POINT('',(427.66521554129,295.651346183216,395.671178941548));
#58733=CARTESIAN_POINT('Origin',(427.66521554129,291.082459603111,392.450702781548));
#58734=CARTESIAN_POINT('',(427.66521554129,290.896525325321,392.450702781548));
#58735=CARTESIAN_POINT('',(427.478070908105,291.082459603111,392.188612046799));
#58736=CARTESIAN_POINT('Origin',(322.566620000605,317.43247610321,497.549298322233));
#58737=CARTESIAN_POINT('',(322.566620000605,320.829980103209,501.460898322233));
#58738=CARTESIAN_POINT('Origin',(322.566620000605,320.829980103209,497.549298322233));
#58739=CARTESIAN_POINT('',(322.566620000605,314.03497210321,501.460898322233));
#58740=CARTESIAN_POINT('',(322.566620000605,317.43247610321,501.460898322233));
#58741=CARTESIAN_POINT('Origin',(322.566620000605,314.03497210321,497.549298322233));
#58742=CARTESIAN_POINT('Origin',(326.775501600605,320.82998010321,497.549298322233));
#58743=CARTESIAN_POINT('',(322.566620000605,320.829980103209,493.358298322233));
#58744=CARTESIAN_POINT('Origin',(322.566620000605,320.829980103209,497.549298322233));
#58745=CARTESIAN_POINT('Origin',(322.566620000605,317.43247610321,497.549298322233));
#58746=CARTESIAN_POINT('',(322.566620000605,314.03497210321,493.358298322233));
#58747=CARTESIAN_POINT('',(322.566620000605,317.432476103209,493.358298322233));
#58748=CARTESIAN_POINT('Origin',(322.566620000605,314.03497210321,497.549298322233));
#58749=CARTESIAN_POINT('Origin',(326.775501600605,314.03497210321,497.549298322233));
#58750=CARTESIAN_POINT('Origin',(322.566620000606,298.539939847209,497.549298322233));
#58751=CARTESIAN_POINT('',(322.566620000606,298.546824263209,500.769774482233));
#58752=CARTESIAN_POINT('',(320.695173668754,298.546824263209,494.928390974743));
#58753=CARTESIAN_POINT('Origin',(322.566620000606,298.546824263209,497.549298322233));
#58754=CARTESIAN_POINT('Origin',(322.566620000606,298.546824263209,497.549298322233));
#58755=CARTESIAN_POINT('',(320.73517960089,298.477980103209,494.984418144581));
#58756=CARTESIAN_POINT('',(320.699174261968,298.539939847209,494.933993691727));
#58757=CARTESIAN_POINT('Origin',(322.566620000606,298.477980103209,497.549298322233));
#58758=CARTESIAN_POINT('Origin',(325.736133600606,298.47798010321,497.549298322233));
#58759=CARTESIAN_POINT('Origin',(322.566620000606,295.65134618321,497.549298322233));
#58760=CARTESIAN_POINT('',(322.566620000607,292.75586810321,500.769774482233));
#58761=CARTESIAN_POINT('',(320.695173668754,292.75586810321,494.928390974743));
#58762=CARTESIAN_POINT('Origin',(322.566620000607,292.75586810321,497.549298322233));
#58763=CARTESIAN_POINT('Origin',(322.566620000607,292.75586810321,497.549298322233));
#58764=CARTESIAN_POINT('',(322.566620000606,295.65134618321,500.769774482233));
#58765=CARTESIAN_POINT('Origin',(322.566620000607,291.082459603104,497.549298322233));
#58766=CARTESIAN_POINT('',(322.566620000607,290.896525325315,497.549298322233));
#58767=CARTESIAN_POINT('',(322.379475367421,291.082459603104,497.287207587484));
#58768=CARTESIAN_POINT('Origin',(464.492340170948,302.000655303219,445.000000551888));
#58769=CARTESIAN_POINT('',(271.071258570948,302.000655303206,530.262016502755));
#58770=CARTESIAN_POINT('',(271.071258570948,302.000655303205,359.737984601026));
#58771=CARTESIAN_POINT('',(271.071258570948,302.000655303206,530.262016502755));
#58772=CARTESIAN_POINT('',(464.474458570948,302.00065530322,530.262016502755));
#58773=CARTESIAN_POINT('',(271.071258570948,302.000655303206,530.262016502755));
#58774=CARTESIAN_POINT('',(464.474458570947,302.000655303218,359.737984601026));
#58775=CARTESIAN_POINT('',(464.474458570948,302.00065530322,530.262016502755));
#58776=CARTESIAN_POINT('',(407.733894628553,302.000655303214,359.737984601026));
#58777=CARTESIAN_POINT('',(407.733894628553,302.000655303214,359.737984601026));
#58778=CARTESIAN_POINT('',(404.706788582958,302.000655303214,373.473600551891));
#58779=CARTESIAN_POINT('Ctrl Pts',(404.706788582958,302.000655303214,373.473600551891));
#58780=CARTESIAN_POINT('Ctrl Pts',(406.157952436569,302.000655303214,368.402118484692));
#58781=CARTESIAN_POINT('Ctrl Pts',(407.733894628554,302.000655303214,359.737984601022));
#58782=CARTESIAN_POINT('',(426.614925770948,302.000655303216,373.47360055189));
#58783=CARTESIAN_POINT('',(426.614925770948,302.000655303216,373.47360055189));
#58784=CARTESIAN_POINT('',(446.642317770948,302.000655303217,393.50099255189));
#58785=CARTESIAN_POINT('',(446.642317770948,302.000655303217,393.50099255189));
#58786=CARTESIAN_POINT('',(446.642317770948,302.000655303218,496.49900855189));
#58787=CARTESIAN_POINT('',(446.642317770948,302.000655303218,496.499008551891));
#58788=CARTESIAN_POINT('',(426.614925770948,302.000655303217,516.52640055189));
#58789=CARTESIAN_POINT('',(426.614925770948,302.000655303217,516.52640055189));
#58790=CARTESIAN_POINT('',(323.616909770948,302.00065530321,516.526400551891));
#58791=CARTESIAN_POINT('',(323.616909770948,302.00065530321,516.526400551891));
#58792=CARTESIAN_POINT('',(303.589517770948,302.000655303208,496.499008551891));
#58793=CARTESIAN_POINT('',(303.589517770948,302.000655303208,496.499008551891));
#58794=CARTESIAN_POINT('',(303.589517770948,302.000655303208,393.500992551891));
#58795=CARTESIAN_POINT('',(303.589517770948,302.000655303208,393.500992551891));
#58796=CARTESIAN_POINT('',(316.405264128415,302.000655303208,380.685246194424));
#58797=CARTESIAN_POINT('',(316.405264128415,302.000655303208,380.685246194424));
#58798=CARTESIAN_POINT('',(315.741199156673,302.000655303208,379.6288809737));
#58799=CARTESIAN_POINT('',(315.741199156673,302.000655303208,379.6288809737));
#58800=CARTESIAN_POINT('',(310.311060913343,302.000655303208,359.737984601026));
#58801=CARTESIAN_POINT('Ctrl Pts',(310.311060913342,302.000655303208,359.737984601022));
#58802=CARTESIAN_POINT('Ctrl Pts',(313.19124860752,302.000655303208,375.572532288989));
#58803=CARTESIAN_POINT('Ctrl Pts',(315.741199156672,302.000655303208,379.628880973699));
#58804=CARTESIAN_POINT('',(271.071258570948,302.000655303205,359.737984601026));
#58805=CARTESIAN_POINT('Origin',(359.02247777095,249.071311553972,331.655798731546));
#58806=CARTESIAN_POINT('',(367.706500485028,311.19711150173,330.571673357733));
#58807=CARTESIAN_POINT('',(350.338455056865,311.197111501729,330.571673357734));
#58808=CARTESIAN_POINT('Origin',(359.022477770949,249.407877716595,330.571673357734));
#58809=CARTESIAN_POINT('',(350.556449206845,307.437429180769,373.473600551891));
#58810=CARTESIAN_POINT('',(350.338455056865,311.197111501729,330.571673357734));
#58811=CARTESIAN_POINT('',(367.488506335048,307.43742918077,373.473600551891));
#58812=CARTESIAN_POINT('Origin',(359.02247777095,247.199284325311,373.473600551891));
#58813=CARTESIAN_POINT('',(367.488506335048,307.43742918077,373.473600551891));
#58814=CARTESIAN_POINT('Origin',(385.304007296866,308.72551700596,330.55385980262));
#58815=CARTESIAN_POINT('',(402.378703501902,302.533931748012,373.473600551891));
#58816=CARTESIAN_POINT('',(367.488506335048,307.43742918077,373.473600551891));
#58817=CARTESIAN_POINT('',(402.901080310565,306.250835876051,330.571673357733));
#58818=CARTESIAN_POINT('',(402.378703501902,302.533931748012,373.473600551891));
#58819=CARTESIAN_POINT('',(402.901080310565,306.250835876051,330.571673357733));
#58820=CARTESIAN_POINT('Origin',(359.022477770951,245.494607052455,331.655798731566));
#58821=CARTESIAN_POINT('',(350.338455056874,183.368807104691,330.571673357735));
#58822=CARTESIAN_POINT('',(367.706500485037,183.368807104693,330.571673357735));
#58823=CARTESIAN_POINT('Origin',(359.022477770951,245.158040889847,330.571673357734));
#58824=CARTESIAN_POINT('',(367.488506335057,187.128489425653,373.473600551892));
#58825=CARTESIAN_POINT('',(367.706500485037,183.368807104693,330.571673357735));
#58826=CARTESIAN_POINT('',(350.556449206854,187.128489425652,373.473600551892));
#58827=CARTESIAN_POINT('Origin',(359.022477770951,247.366634281122,373.473600551892));
#58828=CARTESIAN_POINT('',(350.556449206854,187.128489425652,373.473600551892));
#58829=CARTESIAN_POINT('Origin',(332.740948245037,185.840401600462,330.553859802622));
#58830=CARTESIAN_POINT('',(323.616909770955,190.91459478447,373.473600551892));
#58831=CARTESIAN_POINT('',(350.556449206854,187.128489425652,373.473600551892));
#58832=CARTESIAN_POINT('',(316.405264128422,192.565263303208,380.685246194425));
#58833=CARTESIAN_POINT('',(323.616909770955,190.91459478447,373.473600551892));
#58834=CARTESIAN_POINT('',(315.74119915668,192.565263303208,379.628880973701));
#58835=CARTESIAN_POINT('',(316.405264128422,192.565263303208,380.685246194425));
#58836=CARTESIAN_POINT('',(315.143875231337,188.31508273037,330.571673357735));
#58837=CARTESIAN_POINT('',(315.74119915668,192.565263303208,379.628880973701));
#58838=CARTESIAN_POINT('',(315.143875231337,188.31508273037,330.571673357735));
#58839=CARTESIAN_POINT('Origin',(332.740948245028,308.725517005956,330.553859802621));
#58840=CARTESIAN_POINT('',(315.143875231329,306.250835876046,330.571673357734));
#58841=CARTESIAN_POINT('',(350.338455056865,311.197111501729,330.571673357734));
#58842=CARTESIAN_POINT('',(315.741199156673,302.000655303208,379.6288809737));
#58843=CARTESIAN_POINT('',(323.616909770947,303.651323821948,373.473600551891));
#58844=CARTESIAN_POINT('',(316.405264128415,302.000655303208,380.685246194424));
#58845=CARTESIAN_POINT('',(323.616909770947,303.651323821948,373.473600551891));
#58846=CARTESIAN_POINT('Origin',(426.632807370947,311.415317703215,373.47360055189));
#58847=CARTESIAN_POINT('',(323.616909770946,320.829980103208,373.473600551891));
#58848=CARTESIAN_POINT('',(323.616909770947,303.651323821948,373.473600551891));
#58849=CARTESIAN_POINT('',(426.614925770946,320.829980103215,373.47360055189));
#58850=CARTESIAN_POINT('',(323.616909770946,320.829980103208,373.473600551891));
#58851=CARTESIAN_POINT('',(426.614925770948,302.000655303215,373.47360055189));
#58852=CARTESIAN_POINT('Origin',(400.433645843278,288.694127375541,373.473600551888));
#58853=CARTESIAN_POINT('Origin',(426.632807370956,183.088015303216,373.473600551891));
#58854=CARTESIAN_POINT('',(402.378703501909,192.031986858416,373.473600551891));
#58855=CARTESIAN_POINT('',(402.378703501909,192.031986858416,373.473600551891));
#58856=CARTESIAN_POINT('',(404.706788582966,192.565263303214,373.473600551891));
#58857=CARTESIAN_POINT('Origin',(400.433645843284,205.871791230884,373.473600551894));
#58858=CARTESIAN_POINT('',(426.614925770955,192.565263303216,373.473600551891));
#58859=CARTESIAN_POINT('',(404.706788582966,192.565263303214,373.473600551891));
#58860=CARTESIAN_POINT('',(426.614925770956,173.610767303216,373.473600551892));
#58861=CARTESIAN_POINT('',(426.614925770956,173.610767303216,373.473600551892));
#58862=CARTESIAN_POINT('',(323.616909770956,173.610767303209,373.473600551892));
#58863=CARTESIAN_POINT('',(323.616909770956,173.610767303209,373.473600551892));
#58864=CARTESIAN_POINT('',(323.616909770956,173.610767303209,373.473600551892));
#58865=CARTESIAN_POINT('Origin',(385.304007296874,185.840401600465,330.553859802621));
#58866=CARTESIAN_POINT('',(402.901080310573,188.315082730376,330.571673357734));
#58867=CARTESIAN_POINT('',(367.706500485037,183.368807104693,330.571673357735));
#58868=CARTESIAN_POINT('',(402.378703501909,192.031986858416,373.473600551891));
#58869=CARTESIAN_POINT('Origin',(367.772858570951,182.141307303882,330.571673357735));
#58870=CARTESIAN_POINT('',(410.104986828528,273.835075933065,330.571673357763));
#58871=CARTESIAN_POINT('Origin',(400.433645843278,288.694127375543,330.571673357734));
#58872=CARTESIAN_POINT('',(464.474458570949,273.835075933041,330.571673357734));
#58873=CARTESIAN_POINT('',(464.474458570949,273.835075933041,330.571673357734));
#58874=CARTESIAN_POINT('',(464.474458570953,220.730842673395,330.571673357734));
#58875=CARTESIAN_POINT('',(464.474458570953,220.730842673395,330.571673357734));
#58876=CARTESIAN_POINT('',(410.104986828532,220.730842673363,330.571673357763));
#58877=CARTESIAN_POINT('',(410.104986828532,220.730842673391,330.571673357734));
#58878=CARTESIAN_POINT('Origin',(400.433645843284,205.871791230884,330.571673357734));
#58879=CARTESIAN_POINT('',(307.939968713374,220.730842673356,330.571673357763));
#58880=CARTESIAN_POINT('Origin',(317.611309698625,205.871791230878,330.571673357734));
#58881=CARTESIAN_POINT('',(271.071258570953,220.730842673381,330.571673357734));
#58882=CARTESIAN_POINT('',(271.071258570953,220.730842673381,330.571673357734));
#58883=CARTESIAN_POINT('',(271.071258570949,273.835075933028,330.571673357734));
#58884=CARTESIAN_POINT('',(271.071258570949,273.835075933028,330.571673357734));
#58885=CARTESIAN_POINT('',(307.93996871337,273.835075933058,330.571673357763));
#58886=CARTESIAN_POINT('',(307.93996871337,273.83507593303,330.571673357734));
#58887=CARTESIAN_POINT('Origin',(317.611309698619,288.694127375538,330.571673357734));
#58888=CARTESIAN_POINT('',(359.022477770953,217.089877703211,330.571673357734));
#58889=CARTESIAN_POINT('Origin',(359.022477770951,247.282959303211,330.571673357734));
#58890=CARTESIAN_POINT('Origin',(447.762010570948,291.986959303217,369.00320055189));
#58891=CARTESIAN_POINT('',(464.474458570948,296.695184583218,369.00320055189));
#58892=CARTESIAN_POINT('Origin',(464.474458570948,291.986959303218,369.00320055189));
#58893=CARTESIAN_POINT('',(431.049562570948,296.695184583216,369.00320055189));
#58894=CARTESIAN_POINT('',(447.762010570948,296.695184583217,369.00320055189));
#58895=CARTESIAN_POINT('',(431.049562570947,295.818635619674,371.739190663921));
#58896=CARTESIAN_POINT('Origin',(431.049562570948,291.986959303216,369.003200551891));
#58897=CARTESIAN_POINT('Origin',(431.049562570948,291.986959303216,369.003200551891));
#58898=CARTESIAN_POINT('Origin',(464.492340170949,287.917865618129,345.15482897938));
#58899=CARTESIAN_POINT('Origin',(400.433645843277,287.197585189467,344.408956761074));
#58900=CARTESIAN_POINT('',(464.474458570949,273.835075933041,330.571673357734));
#58901=CARTESIAN_POINT('Origin',(464.474458570951,247.282959303218,330.553791757734));
#58902=CARTESIAN_POINT('',(464.474458570948,297.532978550114,534.888431212814));
#58903=CARTESIAN_POINT('',(464.474458570948,302.00065530322,530.262016502755));
#58904=CARTESIAN_POINT('',(464.474458570952,247.28295930322,536.643200551891));
#58905=CARTESIAN_POINT('',(464.474458570952,247.28295930322,536.643200551891));
#58906=CARTESIAN_POINT('',(464.474458570955,197.032940056326,534.888431212815));
#58907=CARTESIAN_POINT('',(464.474458570955,197.032940056326,534.888431212815));
#58908=CARTESIAN_POINT('',(464.474458570955,192.56526330322,530.262016502756));
#58909=CARTESIAN_POINT('',(464.474458570955,197.032940056326,534.888431212815));
#58910=CARTESIAN_POINT('',(464.474458570955,192.565263303218,359.737984601027));
#58911=CARTESIAN_POINT('',(464.474458570955,192.565263303218,359.737984601027));
#58912=CARTESIAN_POINT('',(464.474458570953,220.730842673395,330.571673357734));
#58913=CARTESIAN_POINT('',(464.474458570954,207.287184583218,369.003200551891));
#58914=CARTESIAN_POINT('Origin',(464.474458570954,202.578959303218,369.003200551891));
#58915=CARTESIAN_POINT('',(464.474458570949,296.695184583219,520.99680055189));
#58916=CARTESIAN_POINT('Origin',(464.474458570949,291.98695930322,520.99680055189));
#58917=CARTESIAN_POINT('',(464.474458570955,207.287184583219,520.996800551891));
#58918=CARTESIAN_POINT('Origin',(464.474458570955,202.578959303219,520.996800551891));
#58919=CARTESIAN_POINT('Origin',(447.762010570954,202.578959303217,369.003200551891));
#58920=CARTESIAN_POINT('',(431.049562570954,207.287184583216,369.003200551891));
#58921=CARTESIAN_POINT('',(447.762010570954,207.287184583217,369.003200551891));
#58922=CARTESIAN_POINT('',(431.049562570953,206.410635619674,371.739190663922));
#58923=CARTESIAN_POINT('Origin',(431.049562570954,202.578959303216,369.003200551891));
#58924=CARTESIAN_POINT('Origin',(431.049562570954,202.578959303216,369.003200551891));
#58925=CARTESIAN_POINT('Origin',(464.492340170954,206.648052988306,345.15482897938));
#58926=CARTESIAN_POINT('',(407.73389462856,192.565263303214,359.737984601027));
#58927=CARTESIAN_POINT('',(407.73389462856,192.565263303214,359.737984601027));
#58928=CARTESIAN_POINT('Origin',(400.433645843283,207.36833341696,344.408956761074));
#58929=CARTESIAN_POINT('Origin',(464.492340170953,222.157949679773,535.765815882353));
#58930=CARTESIAN_POINT('',(271.071258570955,197.032940056313,534.888431212815));
#58931=CARTESIAN_POINT('',(271.071258570955,197.032940056313,534.888431212815));
#58932=CARTESIAN_POINT('',(445.915945087977,247.282959303218,536.643200551891));
#58933=CARTESIAN_POINT('',(445.915945087977,247.282959303218,536.643200551891));
#58934=CARTESIAN_POINT('',(438.427890453927,247.282959303217,536.643200551891));
#58935=CARTESIAN_POINT('Origin',(442.171917770952,250.687930181368,536.762104755053));
#58936=CARTESIAN_POINT('',(367.594537087977,247.282959303213,536.643200551891));
#58937=CARTESIAN_POINT('',(367.594537087977,247.282959303213,536.643200551891));
#58938=CARTESIAN_POINT('',(360.106482453926,247.282959303212,536.643200551891));
#58939=CARTESIAN_POINT('Origin',(363.850509770952,243.527086301937,536.512042576573));
#58940=CARTESIAN_POINT('',(333.509010890952,247.282959303211,536.643200551891));
#58941=CARTESIAN_POINT('',(333.509010890952,247.282959303211,536.643200551891));
#58942=CARTESIAN_POINT('',(332.869141902422,210.624889501466,535.363072546332));
#58943=CARTESIAN_POINT('',(332.869141902422,210.624889501466,535.363072546333));
#58944=CARTESIAN_POINT('',(327.592975586647,205.44001530321,535.182012749611));
#58945=CARTESIAN_POINT('',(327.592975586647,205.44001530321,535.182012749612));
#58946=CARTESIAN_POINT('',(271.071258570955,205.440015303207,535.182012749612));
#58947=CARTESIAN_POINT('',(271.071258570955,205.440015303207,535.182012749612));
#58948=CARTESIAN_POINT('',(271.071258570955,197.032940056313,534.888431212815));
#58949=CARTESIAN_POINT('Origin',(447.762010570955,202.578959303218,520.996800551891));
#58950=CARTESIAN_POINT('',(431.049562570954,207.287184583217,520.996800551891));
#58951=CARTESIAN_POINT('',(447.762010570954,207.287184583218,520.996800551891));
#58952=CARTESIAN_POINT('',(431.049562570954,206.410635619676,523.732790663922));
#58953=CARTESIAN_POINT('Origin',(431.049562570955,202.578959303217,520.996800551891));
#58954=CARTESIAN_POINT('Origin',(431.049562570955,202.578959303217,520.996800551891));
#58955=CARTESIAN_POINT('Origin',(464.492340170955,194.799101679773,532.575223857785));
#58956=CARTESIAN_POINT('',(271.071258570955,192.565263303206,530.262016502756));
#58957=CARTESIAN_POINT('',(271.071258570955,192.565263303207,530.262016502756));
#58958=CARTESIAN_POINT('',(271.071258570955,192.565263303207,530.262016502756));
#58959=CARTESIAN_POINT('Origin',(464.492340170948,299.766816926667,532.575223857784));
#58960=CARTESIAN_POINT('',(271.071258570948,297.5329785501,534.888431212814));
#58961=CARTESIAN_POINT('',(271.071258570948,297.5329785501,534.888431212814));
#58962=CARTESIAN_POINT('',(271.071258570948,297.5329785501,534.888431212814));
#58963=CARTESIAN_POINT('Origin',(447.762010570949,291.986959303218,520.99680055189));
#58964=CARTESIAN_POINT('',(431.049562570948,296.695184583217,520.99680055189));
#58965=CARTESIAN_POINT('',(447.762010570948,296.695184583218,520.99680055189));
#58966=CARTESIAN_POINT('',(431.049562570948,295.818635619675,523.732790663921));
#58967=CARTESIAN_POINT('Origin',(431.049562570949,291.986959303217,520.996800551891));
#58968=CARTESIAN_POINT('Origin',(431.049562570949,291.986959303217,520.996800551891));
#58969=CARTESIAN_POINT('Origin',(464.49234017095,272.407968926666,535.765815882352));
#58970=CARTESIAN_POINT('',(271.071258570949,289.125903303207,535.182012749611));
#58971=CARTESIAN_POINT('',(271.071258570949,289.125903303207,535.182012749611));
#58972=CARTESIAN_POINT('',(327.592975586641,289.12590330321,535.182012749611));
#58973=CARTESIAN_POINT('',(327.592975586641,289.12590330321,535.182012749611));
#58974=CARTESIAN_POINT('',(332.869141902417,283.941029104955,535.363072546332));
#58975=CARTESIAN_POINT('',(332.869141902417,283.941029104955,535.363072546332));
#58976=CARTESIAN_POINT('',(333.509010890952,247.282959303211,536.643200551891));
#58977=CARTESIAN_POINT('Origin',(363.850509770952,243.877988425064,536.762104755053));
#58978=CARTESIAN_POINT('Origin',(442.171917770952,251.038832304494,536.512042576573));
#58979=CARTESIAN_POINT('Origin',(464.492340170955,192.565263303219,445.000000551889));
#58980=CARTESIAN_POINT('',(271.071258570955,192.565263303205,413.628947618471));
#58981=CARTESIAN_POINT('',(271.071258570955,192.565263303205,413.628947618471));
#58982=CARTESIAN_POINT('',(271.071258570955,192.565263303205,404.844653485312));
#58983=CARTESIAN_POINT('Origin',(267.168274890955,192.565263303205,409.236800551892));
#58984=CARTESIAN_POINT('',(271.071258570955,192.565263303205,359.737984601027));
#58985=CARTESIAN_POINT('',(271.071258570955,192.565263303205,359.737984601027));
#58986=CARTESIAN_POINT('',(310.31106091335,192.565263303208,359.737984601027));
#58987=CARTESIAN_POINT('',(271.071258570955,192.565263303205,359.737984601027));
#58988=CARTESIAN_POINT('Ctrl Pts',(315.741199156679,192.565263303208,379.6288809737));
#58989=CARTESIAN_POINT('Ctrl Pts',(313.191248607527,192.565263303208,375.57253228899));
#58990=CARTESIAN_POINT('Ctrl Pts',(310.311060913349,192.565263303208,359.737984601023));
#58991=CARTESIAN_POINT('',(303.589517770955,192.565263303208,393.500992551892));
#58992=CARTESIAN_POINT('',(303.589517770955,192.565263303208,393.500992551892));
#58993=CARTESIAN_POINT('',(303.589517770955,192.565263303208,496.499008551892));
#58994=CARTESIAN_POINT('',(303.589517770955,192.565263303208,496.499008551892));
#58995=CARTESIAN_POINT('',(323.616909770955,192.56526330321,516.526400551892));
#58996=CARTESIAN_POINT('',(323.616909770955,192.56526330321,516.526400551892));
#58997=CARTESIAN_POINT('',(426.614925770955,192.565263303217,516.526400551891));
#58998=CARTESIAN_POINT('',(426.614925770955,192.565263303217,516.526400551891));
#58999=CARTESIAN_POINT('',(446.642317770955,192.565263303218,496.499008551891));
#59000=CARTESIAN_POINT('',(446.642317770955,192.565263303218,496.499008551891));
#59001=CARTESIAN_POINT('',(446.642317770955,192.565263303217,393.500992551891));
#59002=CARTESIAN_POINT('',(446.642317770955,192.565263303217,393.500992551891));
#59003=CARTESIAN_POINT('',(426.614925770955,192.565263303216,373.473600551891));
#59004=CARTESIAN_POINT('Ctrl Pts',(407.733894628561,192.565263303214,359.737984601023));
#59005=CARTESIAN_POINT('Ctrl Pts',(406.157952436577,192.565263303214,368.402118484693));
#59006=CARTESIAN_POINT('Ctrl Pts',(404.706788582965,192.565263303214,373.473600551892));
#59007=CARTESIAN_POINT('Origin',(298.461074890952,247.282959303208,530.301894951891));
#59008=CARTESIAN_POINT('',(271.071258570951,256.407969349735,522.619469351891));
#59009=CARTESIAN_POINT('',(298.461074890954,218.413116103208,522.619469351891));
#59010=CARTESIAN_POINT('Origin',(298.461074890952,247.282959303208,522.619469351891));
#59011=CARTESIAN_POINT('',(298.461074890954,218.413116103208,537.984320551892));
#59012=CARTESIAN_POINT('',(298.461074890954,218.413116103208,530.301894951892));
#59013=CARTESIAN_POINT('',(281.684561271989,270.777989356079,537.984320551891));
#59014=CARTESIAN_POINT('Origin',(298.461074890952,247.282959303208,537.984320551891));
#59015=CARTESIAN_POINT('Origin',(298.461074890952,247.282959303208,537.984320551891));
#59016=CARTESIAN_POINT('',(271.071258570952,238.157949256678,522.619469351891));
#59017=CARTESIAN_POINT('Origin',(298.461074890952,247.282959303208,522.619469351891));
#59018=CARTESIAN_POINT('',(271.071258570952,238.157949256678,536.324548179447));
#59019=CARTESIAN_POINT('',(271.071258570952,238.157949256678,536.324548179447));
#59020=CARTESIAN_POINT('',(269.591231690952,247.282959303206,536.643200551891));
#59021=CARTESIAN_POINT('Origin',(298.461074890952,247.282959303208,536.643200551891));
#59022=CARTESIAN_POINT('',(271.071258570951,256.407969349735,536.324548179447));
#59023=CARTESIAN_POINT('Origin',(298.461074890952,247.282959303208,536.643200551891));
#59024=CARTESIAN_POINT('',(271.071258570951,256.407969349735,522.619469351891));
#59025=CARTESIAN_POINT('Origin',(298.461074890952,247.282959303208,536.911424551891));
#59026=CARTESIAN_POINT('',(271.071258570952,238.214682172211,534.944448551891));
#59027=CARTESIAN_POINT('',(298.46107489095,276.134920903208,534.944448551891));
#59028=CARTESIAN_POINT('Origin',(298.461074890952,247.282959303208,534.944448551891));
#59029=CARTESIAN_POINT('',(298.46107489095,276.134920903208,538.878400551891));
#59030=CARTESIAN_POINT('',(298.46107489095,276.134920903208,536.911424551891));
#59031=CARTESIAN_POINT('Origin',(298.461074890952,247.282959303208,538.878400551891));
#59032=CARTESIAN_POINT('',(271.071258570951,256.351236434202,534.944448551891));
#59033=CARTESIAN_POINT('Origin',(298.461074890952,247.282959303208,534.944448551891));
#59034=CARTESIAN_POINT('',(271.071258570951,256.351236434202,536.326529336513));
#59035=CARTESIAN_POINT('',(271.071258570951,256.351236434202,536.326529336513));
#59036=CARTESIAN_POINT('',(269.609113290952,247.282959303206,536.643200551891));
#59037=CARTESIAN_POINT('Origin',(298.461074890952,247.282959303208,536.643200551891));
#59038=CARTESIAN_POINT('',(271.071258570952,238.214682172211,536.326529336513));
#59039=CARTESIAN_POINT('Origin',(298.461074890952,247.282959303208,536.643200551891));
#59040=CARTESIAN_POINT('',(271.071258570952,238.214682172211,534.944448551891));
#59041=CARTESIAN_POINT('Origin',(271.089140170951,251.817097868704,536.484864944202));
#59042=CARTESIAN_POINT('',(271.071258570952,247.282959303207,536.643200551891));
#59043=CARTESIAN_POINT('',(271.071258570952,247.282959303207,536.643200551891));
#59044=CARTESIAN_POINT('',(271.071258570952,247.282959303207,536.643200551891));
#59045=CARTESIAN_POINT('Origin',(271.089140170952,242.748820737708,536.484864944202));
#59046=CARTESIAN_POINT('',(271.071258570952,238.214682172211,536.326529336513));
#59047=CARTESIAN_POINT('Origin',(265.827154890955,192.583144903205,406.913912572845));
#59048=CARTESIAN_POINT('',(264.486034890955,192.565263303205,407.688208565861));
#59049=CARTESIAN_POINT('',(267.168274890955,192.565263303205,406.139616579829));
#59050=CARTESIAN_POINT('',(264.486034890955,192.565263303205,407.688208565861));
#59051=CARTESIAN_POINT('',(264.486034890955,192.118223303205,407.688208565861));
#59052=CARTESIAN_POINT('',(264.486034890955,192.565263303205,407.688208565861));
#59053=CARTESIAN_POINT('',(267.168274890955,192.118223303205,406.139616579829));
#59054=CARTESIAN_POINT('',(264.486034890955,192.118223303205,407.688208565861));
#59055=CARTESIAN_POINT('',(267.168274890955,192.565263303205,406.139616579829));
#59056=CARTESIAN_POINT('Origin',(264.486034890955,192.341743303205,407.670326965861));
#59057=CARTESIAN_POINT('',(264.486034890955,192.565263303205,410.785392537923));
#59058=CARTESIAN_POINT('',(264.486034890955,192.565263303205,410.785392537923));
#59059=CARTESIAN_POINT('',(264.486034890955,192.118223303205,410.785392537923));
#59060=CARTESIAN_POINT('',(264.486034890955,192.565263303205,410.785392537923));
#59061=CARTESIAN_POINT('',(264.486034890955,192.118223303205,410.785392537923));
#59062=CARTESIAN_POINT('Origin',(265.827154890955,192.583144903205,411.559688530939));
#59063=CARTESIAN_POINT('',(267.168274890955,192.565263303205,412.333984523954));
#59064=CARTESIAN_POINT('',(267.168274890955,192.565263303205,412.333984523954));
#59065=CARTESIAN_POINT('',(267.168274890955,192.118223303205,412.333984523954));
#59066=CARTESIAN_POINT('',(267.168274890955,192.565263303205,412.333984523954));
#59067=CARTESIAN_POINT('',(267.168274890955,192.118223303205,412.333984523954));
#59068=CARTESIAN_POINT('Origin',(329.95734926431,244.855096103656,522.619469351891));
#59069=CARTESIAN_POINT('',(271.071258570952,238.157949256678,522.619469351891));
#59070=CARTESIAN_POINT('Origin',(298.46107489095,247.282959303208,534.85504055189));
#59071=CARTESIAN_POINT('',(271.071258570952,241.675722415372,534.050368551892));
#59072=CARTESIAN_POINT('Ctrl Pts',(271.071258570952,241.675722415372,534.050368551892));
#59073=CARTESIAN_POINT('Ctrl Pts',(271.071258570952,239.972437423184,534.391979643008));
#59074=CARTESIAN_POINT('Ctrl Pts',(271.071258570952,238.214682172211,534.944448551891));
#59075=CARTESIAN_POINT('',(271.071258570951,252.89019619104,534.050368551891));
#59076=CARTESIAN_POINT('Origin',(298.461074890952,247.282959303208,534.050368551891));
#59077=CARTESIAN_POINT('Ctrl Pts',(271.071258570951,256.351236434202,534.944448551891));
#59078=CARTESIAN_POINT('Ctrl Pts',(271.071258570951,254.593481183229,534.391979643008));
#59079=CARTESIAN_POINT('Ctrl Pts',(271.071258570951,252.89019619104,534.050368551891));
#59080=CARTESIAN_POINT('Origin',(326.436838090951,247.28295930321,534.050368551891));
#59081=CARTESIAN_POINT('',(271.071258570951,252.89019619104,534.050368551891));
#59082=CARTESIAN_POINT('',(298.46107489095,269.108793223208,534.050368551891));
#59083=CARTESIAN_POINT('Origin',(298.461074890952,247.282959303208,534.050368551891));
#59084=CARTESIAN_POINT('Origin',(272.783706570949,291.986959303207,520.996800551891));
#59085=CARTESIAN_POINT('',(274.496154570948,296.695184583207,520.996800551891));
#59086=CARTESIAN_POINT('',(274.496154570949,288.155282986749,523.732790663921));
#59087=CARTESIAN_POINT('Origin',(274.496154570949,291.986959303207,520.996800551891));
#59088=CARTESIAN_POINT('Origin',(274.496154570949,291.986959303207,520.996800551891));
#59089=CARTESIAN_POINT('',(271.071258570948,296.695184583206,520.996800551891));
#59090=CARTESIAN_POINT('',(272.783706570948,296.695184583207,520.996800551891));
#59091=CARTESIAN_POINT('Origin',(271.071258570949,291.986959303206,520.996800551891));
#59092=CARTESIAN_POINT('Origin',(272.783706570948,291.986959303205,369.003200551891));
#59093=CARTESIAN_POINT('',(274.496154570948,296.695184583205,369.003200551891));
#59094=CARTESIAN_POINT('',(274.496154570949,288.155282986747,371.739190663921));
#59095=CARTESIAN_POINT('Origin',(274.496154570948,291.986959303205,369.003200551891));
#59096=CARTESIAN_POINT('Origin',(274.496154570948,291.986959303205,369.003200551891));
#59097=CARTESIAN_POINT('',(271.071258570948,296.695184583205,369.003200551891));
#59098=CARTESIAN_POINT('',(272.783706570948,296.695184583205,369.003200551891));
#59099=CARTESIAN_POINT('Origin',(271.071258570948,291.986959303205,369.003200551891));
#59100=CARTESIAN_POINT('Origin',(272.783706570954,202.578959303205,369.003200551892));
#59101=CARTESIAN_POINT('',(274.496154570954,207.287184583205,369.003200551892));
#59102=CARTESIAN_POINT('',(274.496154570955,198.747282986747,371.739190663922));
#59103=CARTESIAN_POINT('Origin',(274.496154570954,202.578959303205,369.003200551892));
#59104=CARTESIAN_POINT('Origin',(274.496154570954,202.578959303205,369.003200551892));
#59105=CARTESIAN_POINT('',(271.071258570954,207.287184583205,369.003200551892));
#59106=CARTESIAN_POINT('',(272.783706570954,207.287184583205,369.003200551892));
#59107=CARTESIAN_POINT('Origin',(271.071258570954,202.578959303205,369.003200551892));
#59108=CARTESIAN_POINT('Origin',(272.783706570955,202.578959303207,520.996800551892));
#59109=CARTESIAN_POINT('',(274.496154570954,207.287184583207,520.996800551892));
#59110=CARTESIAN_POINT('',(274.496154570955,198.747282986749,523.732790663922));
#59111=CARTESIAN_POINT('Origin',(274.496154570955,202.578959303207,520.996800551892));
#59112=CARTESIAN_POINT('Origin',(274.496154570955,202.578959303207,520.996800551892));
#59113=CARTESIAN_POINT('',(271.071258570954,207.287184583206,520.996800551892));
#59114=CARTESIAN_POINT('',(272.783706570954,207.287184583207,520.996800551892));
#59115=CARTESIAN_POINT('Origin',(271.071258570955,202.578959303206,520.996800551892));
#59116=CARTESIAN_POINT('Origin',(271.071258570952,247.282959303206,534.032486951892));
#59117=CARTESIAN_POINT('Origin',(271.08914017095,268.204431303207,535.912606650751));
#59118=CARTESIAN_POINT('',(263.413138890952,247.282959303206,536.643200551891));
#59119=CARTESIAN_POINT('',(269.591231690952,247.282959303206,536.643200551891));
#59120=CARTESIAN_POINT('',(264.053007879482,283.941029104951,535.363072546332));
#59121=CARTESIAN_POINT('',(264.053007879482,283.941029104951,535.363072546332));
#59122=CARTESIAN_POINT('',(269.329174195257,289.125903303206,535.182012749611));
#59123=CARTESIAN_POINT('',(269.329174195257,289.125903303206,535.182012749611));
#59124=CARTESIAN_POINT('',(271.071258570949,289.125903303207,535.182012749611));
#59125=CARTESIAN_POINT('',(271.071258570951,256.407969349735,536.324548179447));
#59126=CARTESIAN_POINT('Origin',(271.089140170953,226.361487303207,535.912606650752));
#59127=CARTESIAN_POINT('',(271.071258570955,205.440015303207,535.182012749612));
#59128=CARTESIAN_POINT('',(269.329174195263,205.440015303206,535.182012749612));
#59129=CARTESIAN_POINT('',(269.329174195263,205.440015303206,535.182012749612));
#59130=CARTESIAN_POINT('',(264.053007879487,210.624889501461,535.363072546333));
#59131=CARTESIAN_POINT('',(264.053007879487,210.624889501461,535.363072546333));
#59132=CARTESIAN_POINT('',(263.413138890952,247.282959303206,536.643200551891));
#59133=CARTESIAN_POINT('Origin',(271.089140170955,192.565263303205,409.236800551892));
#59134=CARTESIAN_POINT('',(271.071258570955,192.565263303205,404.844653485312));
#59135=CARTESIAN_POINT('',(263.753836065183,192.565263303205,404.454976112844));
#59136=CARTESIAN_POINT('Origin',(267.168274890955,192.565263303205,409.236800551892));
#59137=CARTESIAN_POINT('Origin',(267.168274890955,192.565263303205,409.236800551892));
#59138=CARTESIAN_POINT('',(269.850514890955,192.565263303205,407.688208565861));
#59139=CARTESIAN_POINT('',(267.168274890955,192.565263303205,406.139616579829));
#59140=CARTESIAN_POINT('',(269.850514890955,192.565263303205,410.785392537923));
#59141=CARTESIAN_POINT('',(269.850514890955,192.565263303205,407.688208565861));
#59142=CARTESIAN_POINT('',(269.850514890955,192.565263303205,410.785392537923));
#59143=CARTESIAN_POINT('Origin',(376.045474576545,162.345359303212,428.915241806248));
#59144=CARTESIAN_POINT('',(391.640751370957,162.345359303214,448.361741351892));
#59145=CARTESIAN_POINT('',(391.640751370957,162.345359303214,441.638259751892));
#59146=CARTESIAN_POINT('',(391.640751370957,162.345359303214,448.361741351892));
#59147=CARTESIAN_POINT('',(389.391142518198,162.345359303214,441.638259751892));
#59148=CARTESIAN_POINT('',(391.640751370957,162.345359303214,441.638259751892));
#59149=CARTESIAN_POINT('',(389.391142518198,162.345359303214,448.361741351892));
#59150=CARTESIAN_POINT('Origin',(375.115917770957,162.345359303213,445.000000551892));
#59151=CARTESIAN_POINT('',(389.391142518198,162.345359303214,448.361741351892));
#59152=CARTESIAN_POINT('Origin',(375.11591777096,114.845359303212,445.000000551892));
#59153=CARTESIAN_POINT('',(397.615917770963,82.3453593032132,445.000000551892));
#59154=CARTESIAN_POINT('Origin',(375.115917770963,82.3453593032118,445.000000551893));
#59155=CARTESIAN_POINT('',(397.615917770958,147.345359303214,445.000000551892));
#59156=CARTESIAN_POINT('',(397.61591777096,114.845359303213,445.000000551892));
#59157=CARTESIAN_POINT('Origin',(375.115917770958,147.345359303212,445.000000551892));
#59158=CARTESIAN_POINT('Origin',(375.115917770963,82.3453593032116,422.490000551892));
#59159=CARTESIAN_POINT('Origin',(432.504565497636,326.498447303217,494.755298322232));
#59160=CARTESIAN_POINT('',(430.89144884552,326.016308993801,491.961298322232));
#59161=CARTESIAN_POINT('',(432.09282582224,326.480565703217,494.042144284955));
#59162=CARTESIAN_POINT('Ctrl Pts',(430.891448845508,326.016308993793,491.96129832221));
#59163=CARTESIAN_POINT('Ctrl Pts',(431.532053923755,326.386162508166,493.070858865322));
#59164=CARTESIAN_POINT('Ctrl Pts',(432.092825822243,326.480565703217,494.042144284959));
#59165=CARTESIAN_POINT('',(432.916305173032,326.480565703217,495.46845235951));
#59166=CARTESIAN_POINT('',(432.09282582224,326.480565703217,494.042144284955));
#59167=CARTESIAN_POINT('',(434.117682149752,326.016308993801,497.549298322232));
#59168=CARTESIAN_POINT('Ctrl Pts',(432.916305173029,326.480565703217,495.468452359506));
#59169=CARTESIAN_POINT('Ctrl Pts',(433.477077071517,326.386162508166,496.439737779143));
#59170=CARTESIAN_POINT('Ctrl Pts',(434.117682149765,326.016308993793,497.549298322255));
#59171=CARTESIAN_POINT('',(434.117682149752,320.829980103217,497.549298322232));
#59172=CARTESIAN_POINT('',(434.117682149752,326.016308993801,497.549298322232));
#59173=CARTESIAN_POINT('',(430.891448845521,320.829980103217,491.961298322232));
#59174=CARTESIAN_POINT('',(430.891448845521,320.829980103217,491.961298322232));
#59175=CARTESIAN_POINT('',(430.89144884552,326.016308993801,491.961298322232));
#59176=CARTESIAN_POINT('Origin',(430.909330445546,323.655272903217,491.961298322232));
#59177=CARTESIAN_POINT('',(424.438982237057,326.016308993801,491.961298322232));
#59178=CARTESIAN_POINT('',(426.841736190497,326.480565703217,491.961298322232));
#59179=CARTESIAN_POINT('Ctrl Pts',(424.438982237031,326.016308993793,491.961298322232));
#59180=CARTESIAN_POINT('Ctrl Pts',(425.720192393527,326.386162508166,491.961298322232));
#59181=CARTESIAN_POINT('Ctrl Pts',(426.841736190502,326.480565703217,491.961298322232));
#59182=CARTESIAN_POINT('',(428.48869489208,326.480565703217,491.961298322232));
#59183=CARTESIAN_POINT('',(426.841736190497,326.480565703217,491.961298322232));
#59184=CARTESIAN_POINT('Ctrl Pts',(428.488694892075,326.480565703217,491.961298322232));
#59185=CARTESIAN_POINT('Ctrl Pts',(429.61023868905,326.386162508166,491.961298322232));
#59186=CARTESIAN_POINT('Ctrl Pts',(430.891448845546,326.016308993793,491.961298322232));
#59187=CARTESIAN_POINT('',(424.438982237057,320.829980103216,491.961298322232));
#59188=CARTESIAN_POINT('',(424.438982237057,320.829980103216,491.961298322232));
#59189=CARTESIAN_POINT('',(424.438982237057,326.016308993801,491.961298322232));
#59190=CARTESIAN_POINT('Origin',(422.825865584941,326.498447303216,494.755298322232));
#59191=CARTESIAN_POINT('',(421.212748932825,326.0163089938,497.549298322232));
#59192=CARTESIAN_POINT('',(422.414125909545,326.480565703216,495.46845235951));
#59193=CARTESIAN_POINT('Ctrl Pts',(421.212748932813,326.016308993792,497.549298322255));
#59194=CARTESIAN_POINT('Ctrl Pts',(421.85335401106,326.386162508165,496.439737779143));
#59195=CARTESIAN_POINT('Ctrl Pts',(422.414125909548,326.480565703216,495.468452359506));
#59196=CARTESIAN_POINT('',(423.237605260337,326.480565703216,494.042144284955));
#59197=CARTESIAN_POINT('',(422.414125909545,326.480565703216,495.46845235951));
#59198=CARTESIAN_POINT('Ctrl Pts',(423.237605260335,326.480565703216,494.042144284959));
#59199=CARTESIAN_POINT('Ctrl Pts',(423.798377158822,326.386162508166,493.070858865322));
#59200=CARTESIAN_POINT('Ctrl Pts',(424.43898223707,326.016308993793,491.96129832221));
#59201=CARTESIAN_POINT('',(421.212748932826,320.829980103216,497.549298322232));
#59202=CARTESIAN_POINT('',(421.212748932826,320.829980103216,497.549298322232));
#59203=CARTESIAN_POINT('',(421.212748932825,326.0163089938,497.549298322232));
#59204=CARTESIAN_POINT('Origin',(422.825865584941,326.498447303216,500.343298322232));
#59205=CARTESIAN_POINT('',(424.438982237057,326.016308993801,503.137298322232));
#59206=CARTESIAN_POINT('',(423.237605260337,326.480565703217,501.05645235951));
#59207=CARTESIAN_POINT('Ctrl Pts',(424.43898223707,326.016308993793,503.137298322254));
#59208=CARTESIAN_POINT('Ctrl Pts',(423.798377158822,326.386162508166,502.027737779143));
#59209=CARTESIAN_POINT('Ctrl Pts',(423.237605260335,326.480565703217,501.056452359506));
#59210=CARTESIAN_POINT('',(422.414125909545,326.480565703216,499.630144284955));
#59211=CARTESIAN_POINT('',(423.237605260337,326.480565703217,501.05645235951));
#59212=CARTESIAN_POINT('Ctrl Pts',(422.414125909548,326.480565703216,499.630144284959));
#59213=CARTESIAN_POINT('Ctrl Pts',(421.85335401106,326.386162508165,498.658858865322));
#59214=CARTESIAN_POINT('Ctrl Pts',(421.212748932813,326.016308993792,497.54929832221));
#59215=CARTESIAN_POINT('',(424.438982237057,320.829980103216,503.137298322232));
#59216=CARTESIAN_POINT('',(424.438982237057,320.829980103216,503.137298322232));
#59217=CARTESIAN_POINT('',(424.438982237057,326.016308993801,503.137298322232));
#59218=CARTESIAN_POINT('Origin',(427.665215541289,326.062734664735,497.549298322232));
#59219=CARTESIAN_POINT('',(426.841736190497,326.480565703217,503.137298322232));
#59220=CARTESIAN_POINT('Ctrl Pts',(426.841736190502,326.480565703217,503.137298322232));
#59221=CARTESIAN_POINT('Ctrl Pts',(425.720192393527,326.386162508166,503.137298322232));
#59222=CARTESIAN_POINT('Ctrl Pts',(424.438982237031,326.016308993793,503.137298322232));
#59223=CARTESIAN_POINT('Origin',(427.665215541289,326.480565703217,497.549298322233));
#59224=CARTESIAN_POINT('Origin',(427.665215541288,326.062734664736,497.549298322232));
#59225=CARTESIAN_POINT('Origin',(427.665215541289,326.480565703217,497.549298322232));
#59226=CARTESIAN_POINT('Origin',(427.665215541288,326.062734664735,497.549298322232));
#59227=CARTESIAN_POINT('',(430.89144884552,326.016308993801,503.137298322232));
#59228=CARTESIAN_POINT('',(428.48869489208,326.480565703217,503.137298322232));
#59229=CARTESIAN_POINT('Ctrl Pts',(430.891448845546,326.016308993793,503.137298322232));
#59230=CARTESIAN_POINT('Ctrl Pts',(429.61023868905,326.386162508166,503.137298322232));
#59231=CARTESIAN_POINT('Ctrl Pts',(428.488694892075,326.480565703217,503.137298322232));
#59232=CARTESIAN_POINT('',(432.09282582224,326.480565703217,501.05645235951));
#59233=CARTESIAN_POINT('Ctrl Pts',(432.092825822243,326.480565703217,501.056452359506));
#59234=CARTESIAN_POINT('Ctrl Pts',(431.532053923755,326.386162508166,502.027737779143));
#59235=CARTESIAN_POINT('Ctrl Pts',(430.891448845508,326.016308993793,503.137298322254));
#59236=CARTESIAN_POINT('Origin',(427.665215541289,326.480565703217,497.549298322233));
#59237=CARTESIAN_POINT('Origin',(427.66521554129,326.062734664736,497.549298322232));
#59238=CARTESIAN_POINT('',(432.916305173032,326.480565703217,499.630144284955));
#59239=CARTESIAN_POINT('Ctrl Pts',(434.117682149765,326.016308993793,497.54929832221));
#59240=CARTESIAN_POINT('Ctrl Pts',(433.477077071517,326.386162508166,498.658858865322));
#59241=CARTESIAN_POINT('Ctrl Pts',(432.916305173029,326.480565703217,499.630144284959));
#59242=CARTESIAN_POINT('Origin',(427.665215541289,326.480565703217,497.549298322232));
#59243=CARTESIAN_POINT('Origin',(427.66521554129,326.062734664736,497.549298322231));
#59244=CARTESIAN_POINT('Origin',(427.665215541289,326.480565703217,497.549298322232));
#59245=CARTESIAN_POINT('Origin',(432.504565497636,326.498447303217,500.343298322232));
#59246=CARTESIAN_POINT('',(432.916305173032,326.480565703217,499.630144284955));
#59247=CARTESIAN_POINT('',(430.891448845521,320.829980103217,503.137298322232));
#59248=CARTESIAN_POINT('',(430.89144884552,326.016308993801,503.137298322232));
#59249=CARTESIAN_POINT('',(434.117682149752,320.829980103217,497.549298322232));
#59250=CARTESIAN_POINT('Origin',(430.909330445546,323.655272903217,503.137298322232));
#59251=CARTESIAN_POINT('',(428.48869489208,326.480565703217,503.137298322232));
#59252=CARTESIAN_POINT('',(430.891448845521,320.829980103217,503.137298322232));
#59253=CARTESIAN_POINT('Origin',(427.665215541289,326.062734664735,497.549298322233));
#59254=CARTESIAN_POINT('Origin',(427.665215541288,326.480565703217,497.549298322232));
#59255=CARTESIAN_POINT('Origin',(433.758762284827,326.480565703217,497.549298322232));
#59256=CARTESIAN_POINT('Origin',(327.405969956951,326.498447303209,389.656702781548));
#59257=CARTESIAN_POINT('',(325.792853304836,326.016308993793,386.862702781548));
#59258=CARTESIAN_POINT('',(326.994230281556,326.480565703209,388.943548744271));
#59259=CARTESIAN_POINT('Ctrl Pts',(325.792853304823,326.016308993785,386.862702781526));
#59260=CARTESIAN_POINT('Ctrl Pts',(326.433458383071,326.386162508158,387.972263324638));
#59261=CARTESIAN_POINT('Ctrl Pts',(326.994230281558,326.480565703209,388.943548744275));
#59262=CARTESIAN_POINT('',(327.817709632347,326.480565703209,390.369856818826));
#59263=CARTESIAN_POINT('',(326.994230281556,326.480565703209,388.943548744271));
#59264=CARTESIAN_POINT('',(329.019086609067,326.016308993793,392.450702781548));
#59265=CARTESIAN_POINT('Ctrl Pts',(327.817709632345,326.480565703209,390.369856818822));
#59266=CARTESIAN_POINT('Ctrl Pts',(328.378481530832,326.386162508158,391.341142238459));
#59267=CARTESIAN_POINT('Ctrl Pts',(329.01908660908,326.016308993785,392.450702781571));
#59268=CARTESIAN_POINT('',(329.019086609068,320.829980103209,392.450702781549));
#59269=CARTESIAN_POINT('',(329.019086609067,326.016308993792,392.450702781548));
#59270=CARTESIAN_POINT('',(325.792853304836,320.829980103209,386.862702781548));
#59271=CARTESIAN_POINT('',(325.792853304836,320.829980103209,386.862702781548));
#59272=CARTESIAN_POINT('',(325.792853304836,326.016308993792,386.862702781548));
#59273=CARTESIAN_POINT('Origin',(325.810734904861,323.655272903209,386.862702781548));
#59274=CARTESIAN_POINT('',(319.340386696372,326.016308993792,386.862702781548));
#59275=CARTESIAN_POINT('',(321.743140649812,326.480565703209,386.862702781548));
#59276=CARTESIAN_POINT('Ctrl Pts',(319.340386696347,326.016308993784,386.862702781548));
#59277=CARTESIAN_POINT('Ctrl Pts',(320.621596852842,326.386162508158,386.862702781548));
#59278=CARTESIAN_POINT('Ctrl Pts',(321.743140649817,326.480565703209,386.862702781548));
#59279=CARTESIAN_POINT('',(323.390099351396,326.480565703209,386.862702781548));
#59280=CARTESIAN_POINT('',(321.743140649812,326.480565703209,386.862702781548));
#59281=CARTESIAN_POINT('Ctrl Pts',(323.390099351391,326.480565703209,386.862702781548));
#59282=CARTESIAN_POINT('Ctrl Pts',(324.511643148366,326.386162508158,386.862702781548));
#59283=CARTESIAN_POINT('Ctrl Pts',(325.792853304861,326.016308993785,386.862702781548));
#59284=CARTESIAN_POINT('',(319.340386696372,320.829980103208,386.862702781548));
#59285=CARTESIAN_POINT('',(319.340386696372,320.829980103208,386.862702781548));
#59286=CARTESIAN_POINT('',(319.340386696372,326.016308993792,386.862702781548));
#59287=CARTESIAN_POINT('Origin',(317.727270044256,326.498447303208,389.656702781548));
#59288=CARTESIAN_POINT('',(316.114153392141,326.016308993792,392.450702781548));
#59289=CARTESIAN_POINT('',(317.315530368861,326.480565703208,390.369856818826));
#59290=CARTESIAN_POINT('Ctrl Pts',(316.114153392128,326.016308993784,392.450702781571));
#59291=CARTESIAN_POINT('Ctrl Pts',(316.754758470376,326.386162508157,391.341142238459));
#59292=CARTESIAN_POINT('Ctrl Pts',(317.315530368863,326.480565703209,390.369856818822));
#59293=CARTESIAN_POINT('',(318.139009719652,326.480565703208,388.943548744271));
#59294=CARTESIAN_POINT('',(317.315530368861,326.480565703208,390.369856818826));
#59295=CARTESIAN_POINT('Ctrl Pts',(318.13900971965,326.480565703209,388.943548744275));
#59296=CARTESIAN_POINT('Ctrl Pts',(318.699781618137,326.386162508157,387.972263324638));
#59297=CARTESIAN_POINT('Ctrl Pts',(319.340386696385,326.016308993784,386.862702781526));
#59298=CARTESIAN_POINT('',(316.114153392141,320.829980103208,392.450702781549));
#59299=CARTESIAN_POINT('',(316.114153392141,320.829980103208,392.450702781549));
#59300=CARTESIAN_POINT('',(316.114153392141,326.016308993791,392.450702781548));
#59301=CARTESIAN_POINT('Origin',(317.727270044256,326.498447303209,395.244702781548));
#59302=CARTESIAN_POINT('',(319.340386696372,326.016308993792,398.038702781548));
#59303=CARTESIAN_POINT('',(318.139009719652,326.480565703209,395.957856818826));
#59304=CARTESIAN_POINT('Ctrl Pts',(319.340386696385,326.016308993785,398.038702781571));
#59305=CARTESIAN_POINT('Ctrl Pts',(318.699781618137,326.386162508158,396.929142238459));
#59306=CARTESIAN_POINT('Ctrl Pts',(318.13900971965,326.480565703209,395.957856818822));
#59307=CARTESIAN_POINT('',(317.315530368861,326.480565703208,394.531548744271));
#59308=CARTESIAN_POINT('',(318.139009719652,326.480565703209,395.957856818826));
#59309=CARTESIAN_POINT('Ctrl Pts',(317.315530368863,326.480565703209,394.531548744275));
#59310=CARTESIAN_POINT('Ctrl Pts',(316.754758470376,326.386162508157,393.560263324638));
#59311=CARTESIAN_POINT('Ctrl Pts',(316.114153392128,326.016308993784,392.450702781526));
#59312=CARTESIAN_POINT('',(319.340386696372,320.829980103208,398.038702781548));
#59313=CARTESIAN_POINT('',(319.340386696372,320.829980103208,398.038702781548));
#59314=CARTESIAN_POINT('',(319.340386696372,326.016308993792,398.038702781548));
#59315=CARTESIAN_POINT('Origin',(322.566620000605,326.06273466473,392.450702781554));
#59316=CARTESIAN_POINT('',(321.743140649812,326.480565703209,398.038702781548));
#59317=CARTESIAN_POINT('Ctrl Pts',(321.743140649817,326.480565703209,398.038702781548));
#59318=CARTESIAN_POINT('Ctrl Pts',(320.621596852842,326.386162508158,398.038702781548));
#59319=CARTESIAN_POINT('Ctrl Pts',(319.340386696347,326.016308993785,398.038702781549));
#59320=CARTESIAN_POINT('Origin',(322.566620000605,326.480565703209,392.450702781546));
#59321=CARTESIAN_POINT('Origin',(322.5666200006,326.062734664731,392.450702781548));
#59322=CARTESIAN_POINT('Origin',(322.566620000601,326.480565703209,392.450702781548));
#59323=CARTESIAN_POINT('Origin',(322.566620000602,326.062734664725,392.450702781546));
#59324=CARTESIAN_POINT('',(325.792853304836,326.016308993793,398.038702781548));
#59325=CARTESIAN_POINT('',(323.390099351396,326.480565703209,398.038702781548));
#59326=CARTESIAN_POINT('Ctrl Pts',(325.792853304861,326.016308993785,398.038702781548));
#59327=CARTESIAN_POINT('Ctrl Pts',(324.511643148366,326.386162508158,398.038702781548));
#59328=CARTESIAN_POINT('Ctrl Pts',(323.390099351391,326.480565703209,398.038702781548));
#59329=CARTESIAN_POINT('',(326.994230281556,326.480565703209,395.957856818826));
#59330=CARTESIAN_POINT('Ctrl Pts',(326.994230281558,326.480565703209,395.957856818822));
#59331=CARTESIAN_POINT('Ctrl Pts',(326.433458383071,326.386162508158,396.929142238459));
#59332=CARTESIAN_POINT('Ctrl Pts',(325.792853304823,326.016308993785,398.03870278157));
#59333=CARTESIAN_POINT('Origin',(322.566620000604,326.480565703209,392.450702781548));
#59334=CARTESIAN_POINT('Origin',(322.566620000608,326.06273466473,392.450702781548));
#59335=CARTESIAN_POINT('',(327.817709632347,326.480565703209,394.531548744271));
#59336=CARTESIAN_POINT('Ctrl Pts',(329.01908660908,326.016308993785,392.450702781526));
#59337=CARTESIAN_POINT('Ctrl Pts',(328.378481530832,326.386162508158,393.560263324638));
#59338=CARTESIAN_POINT('Ctrl Pts',(327.817709632345,326.480565703209,394.531548744275));
#59339=CARTESIAN_POINT('Origin',(322.566620000604,326.480565703209,392.450702781548));
#59340=CARTESIAN_POINT('Origin',(322.566620000604,326.062734664727,392.450702781548));
#59341=CARTESIAN_POINT('Origin',(322.566620000604,326.480565703209,392.450702781549));
#59342=CARTESIAN_POINT('Origin',(327.405969956951,326.498447303209,395.244702781548));
#59343=CARTESIAN_POINT('',(327.817709632347,326.480565703209,394.531548744271));
#59344=CARTESIAN_POINT('',(325.792853304836,320.829980103209,398.038702781548));
#59345=CARTESIAN_POINT('',(325.792853304836,326.016308993792,398.038702781548));
#59346=CARTESIAN_POINT('',(329.019086609068,320.829980103209,392.450702781549));
#59347=CARTESIAN_POINT('Origin',(325.810734904861,323.655272903209,398.038702781548));
#59348=CARTESIAN_POINT('',(323.390099351396,326.480565703209,398.038702781548));
#59349=CARTESIAN_POINT('',(325.792853304836,320.829980103209,398.038702781548));
#59350=CARTESIAN_POINT('Origin',(322.56662000061,326.062734664723,392.450702781552));
#59351=CARTESIAN_POINT('Origin',(322.566620000605,326.480565703209,392.450702781551));
#59352=CARTESIAN_POINT('Origin',(328.660166744143,326.480565703209,392.450702781548));
#59353=CARTESIAN_POINT('Origin',(313.603213770955,192.583144903208,383.487296551892));
#59354=CARTESIAN_POINT('',(303.589517770956,173.610767303207,393.500992551892));
#59355=CARTESIAN_POINT('',(303.589517770956,173.610767303207,393.500992551892));
#59356=CARTESIAN_POINT('',(303.589517770956,173.610767303207,393.500992551892));
#59357=CARTESIAN_POINT('Origin',(303.589517770947,311.415317703207,393.483110951891));
#59358=CARTESIAN_POINT('',(303.589517770946,320.829980103207,393.500992551891));
#59359=CARTESIAN_POINT('',(303.589517770948,302.000655303207,393.500992551891));
#59360=CARTESIAN_POINT('',(303.589517770947,320.829980103208,496.499008551891));
#59361=CARTESIAN_POINT('',(303.589517770948,302.000655303208,496.499008551891));
#59362=CARTESIAN_POINT('',(303.589517770947,320.829980103208,496.499008551891));
#59363=CARTESIAN_POINT('Origin',(313.603213770947,320.847861703209,506.512704551891));
#59364=CARTESIAN_POINT('',(323.616909770947,320.82998010321,516.526400551891));
#59365=CARTESIAN_POINT('',(323.616909770948,302.000655303209,516.526400551891));
#59366=CARTESIAN_POINT('',(323.616909770947,320.82998010321,516.526400551891));
#59367=CARTESIAN_POINT('Origin',(426.632807370947,311.415317703216,516.52640055189));
#59368=CARTESIAN_POINT('',(426.614925770947,320.829980103217,516.52640055189));
#59369=CARTESIAN_POINT('',(426.614925770948,302.000655303216,516.52640055189));
#59370=CARTESIAN_POINT('',(426.614925770947,320.829980103217,516.52640055189));
#59371=CARTESIAN_POINT('Origin',(436.628621770947,320.847861703217,506.51270455189));
#59372=CARTESIAN_POINT('',(446.642317770947,320.829980103218,496.49900855189));
#59373=CARTESIAN_POINT('',(446.642317770948,302.000655303218,496.49900855189));
#59374=CARTESIAN_POINT('',(446.642317770947,320.829980103218,496.49900855189));
#59375=CARTESIAN_POINT('Origin',(446.642317770947,311.415317703217,393.48311095189));
#59376=CARTESIAN_POINT('',(446.642317770946,320.829980103217,393.50099255189));
#59377=CARTESIAN_POINT('',(446.642317770948,302.000655303217,393.50099255189));
#59378=CARTESIAN_POINT('',(446.642317770946,320.829980103217,393.50099255189));
#59379=CARTESIAN_POINT('Origin',(436.628621770946,320.847861703216,383.48729655189));
#59380=CARTESIAN_POINT('',(426.614925770946,320.829980103215,373.47360055189));
#59381=CARTESIAN_POINT('Origin',(310.328942513349,206.648052988296,345.154828979381));
#59382=CARTESIAN_POINT('Origin',(317.611309698626,207.368333416955,344.408956761074));
#59383=CARTESIAN_POINT('',(271.071258570953,220.730842673381,330.571673357734));
#59384=CARTESIAN_POINT('Origin',(310.328942513343,287.917865618119,345.15482897938));
#59385=CARTESIAN_POINT('',(271.071258570948,302.000655303205,359.737984601026));
#59386=CARTESIAN_POINT('Origin',(317.611309698621,287.197585189461,344.408956761074));
#59387=CARTESIAN_POINT('Origin',(317.611309698618,288.694127375538,335.477394119331));
#59388=CARTESIAN_POINT('Origin',(442.171917770952,250.859279303218,536.344095603207));
#59389=CARTESIAN_POINT('Origin',(442.171917770952,250.859279303218,536.643200551891));
#59390=CARTESIAN_POINT('Origin',(363.850509770952,243.706639303217,536.577811187259));
#59391=CARTESIAN_POINT('Origin',(363.850509770952,243.706639303213,536.643200551891));
#59392=CARTESIAN_POINT('Origin',(444.872039370952,250.859279303218,534.855040551891));
#59393=CARTESIAN_POINT('',(439.489677770952,252.407871289249,534.855040551891));
#59394=CARTESIAN_POINT('',(439.489677770952,249.310687317187,534.855040551891));
#59395=CARTESIAN_POINT('',(439.489677770952,252.407871289249,534.855040551891));
#59396=CARTESIAN_POINT('',(442.171917770952,247.762095331156,534.855040551891));
#59397=CARTESIAN_POINT('',(439.489677770952,249.310687317187,534.855040551891));
#59398=CARTESIAN_POINT('',(444.854157770952,249.310687317187,534.855040551891));
#59399=CARTESIAN_POINT('',(442.171917770952,247.762095331156,534.855040551891));
#59400=CARTESIAN_POINT('',(444.854157770951,252.407871289249,534.855040551891));
#59401=CARTESIAN_POINT('',(444.854157770952,249.310687317187,534.855040551891));
#59402=CARTESIAN_POINT('',(442.171917770951,253.95646327528,534.855040551891));
#59403=CARTESIAN_POINT('',(444.854157770951,252.407871289249,534.855040551891));
#59404=CARTESIAN_POINT('',(442.171917770951,253.95646327528,534.855040551891));
#59405=CARTESIAN_POINT('Origin',(440.830797770951,253.182167282265,534.837158951891));
#59406=CARTESIAN_POINT('',(442.171917770951,253.95646327528,536.643200551891));
#59407=CARTESIAN_POINT('',(439.489677770952,252.407871289249,536.643200551891));
#59408=CARTESIAN_POINT('',(442.171917770951,253.95646327528,536.643200551891));
#59409=CARTESIAN_POINT('',(439.489677770952,252.407871289249,534.855040551891));
#59410=CARTESIAN_POINT('',(442.171917770951,253.95646327528,534.855040551891));
#59411=CARTESIAN_POINT('Origin',(443.513037770951,253.182167282265,534.837158951891));
#59412=CARTESIAN_POINT('',(444.854157770951,252.407871289249,536.643200551891));
#59413=CARTESIAN_POINT('',(444.854157770951,252.407871289249,536.643200551891));
#59414=CARTESIAN_POINT('',(444.854157770951,252.407871289249,534.855040551891));
#59415=CARTESIAN_POINT('Origin',(444.854157770952,250.859279303218,534.837158951891));
#59416=CARTESIAN_POINT('',(444.854157770952,249.310687317187,536.643200551891));
#59417=CARTESIAN_POINT('',(444.854157770952,249.310687317187,534.855040551891));
#59418=CARTESIAN_POINT('',(444.854157770951,252.407871289249,536.643200551891));
#59419=CARTESIAN_POINT('Origin',(443.513037770952,248.536391324171,534.837158951891));
#59420=CARTESIAN_POINT('',(442.171917770952,247.762095331156,536.643200551891));
#59421=CARTESIAN_POINT('',(442.171917770952,247.762095331156,536.643200551891));
#59422=CARTESIAN_POINT('',(442.171917770952,247.762095331156,534.855040551891));
#59423=CARTESIAN_POINT('Origin',(440.830797770952,248.536391324171,534.837158951891));
#59424=CARTESIAN_POINT('',(439.489677770952,249.310687317187,536.643200551891));
#59425=CARTESIAN_POINT('',(439.489677770952,249.310687317187,536.643200551891));
#59426=CARTESIAN_POINT('',(439.489677770952,249.310687317187,534.855040551891));
#59427=CARTESIAN_POINT('Origin',(439.489677770952,250.859279303218,534.837158951891));
#59428=CARTESIAN_POINT('',(439.489677770952,252.407871289249,536.643200551891));
#59429=CARTESIAN_POINT('Origin',(442.17191777095,250.859279303222,536.577811187251));
#59430=CARTESIAN_POINT('Origin',(442.171917770952,250.859279303218,536.643200551891));
#59431=CARTESIAN_POINT('Origin',(449.455947285591,251.903964171691,536.643200551891));
#59432=CARTESIAN_POINT('Origin',(366.550631370952,243.706639303213,534.855040551891));
#59433=CARTESIAN_POINT('',(361.168269770952,245.255231289244,534.855040551891));
#59434=CARTESIAN_POINT('',(361.168269770952,242.158047317181,534.855040551891));
#59435=CARTESIAN_POINT('',(361.168269770952,245.255231289244,534.855040551891));
#59436=CARTESIAN_POINT('',(363.850509770952,240.60945533115,534.855040551891));
#59437=CARTESIAN_POINT('',(361.168269770952,242.158047317181,534.855040551891));
#59438=CARTESIAN_POINT('',(366.532749770952,242.158047317182,534.855040551891));
#59439=CARTESIAN_POINT('',(363.850509770952,240.60945533115,534.855040551891));
#59440=CARTESIAN_POINT('',(366.532749770952,245.255231289244,534.855040551891));
#59441=CARTESIAN_POINT('',(366.532749770952,242.158047317182,534.855040551891));
#59442=CARTESIAN_POINT('',(363.850509770952,246.803823275275,534.855040551891));
#59443=CARTESIAN_POINT('',(366.532749770952,245.255231289244,534.855040551891));
#59444=CARTESIAN_POINT('',(363.850509770952,246.803823275275,534.855040551891));
#59445=CARTESIAN_POINT('Origin',(362.509389770952,246.029527282259,534.837158951891));
#59446=CARTESIAN_POINT('',(363.850509770952,246.803823275275,536.643200551891));
#59447=CARTESIAN_POINT('',(361.168269770952,245.255231289244,536.643200551891));
#59448=CARTESIAN_POINT('',(363.850509770952,246.803823275275,536.643200551891));
#59449=CARTESIAN_POINT('',(361.168269770952,245.255231289244,534.855040551891));
#59450=CARTESIAN_POINT('',(363.850509770952,246.803823275275,534.855040551891));
#59451=CARTESIAN_POINT('Origin',(365.191629770952,246.02952728226,534.837158951891));
#59452=CARTESIAN_POINT('',(366.532749770952,245.255231289244,536.643200551891));
#59453=CARTESIAN_POINT('',(366.532749770952,245.255231289244,536.643200551891));
#59454=CARTESIAN_POINT('',(366.532749770952,245.255231289244,534.855040551891));
#59455=CARTESIAN_POINT('Origin',(366.532749770952,243.706639303213,534.837158951891));
#59456=CARTESIAN_POINT('',(366.532749770952,242.158047317182,536.643200551891));
#59457=CARTESIAN_POINT('',(366.532749770952,242.158047317182,534.855040551891));
#59458=CARTESIAN_POINT('',(366.532749770952,245.255231289244,536.643200551891));
#59459=CARTESIAN_POINT('Origin',(365.191629770952,241.383751324166,534.837158951891));
#59460=CARTESIAN_POINT('',(363.850509770952,240.60945533115,536.643200551891));
#59461=CARTESIAN_POINT('',(363.850509770952,240.60945533115,536.643200551891));
#59462=CARTESIAN_POINT('',(363.850509770952,240.60945533115,534.855040551891));
#59463=CARTESIAN_POINT('Origin',(362.509389770952,241.383751324166,534.837158951891));
#59464=CARTESIAN_POINT('',(361.168269770952,242.158047317181,536.643200551891));
#59465=CARTESIAN_POINT('',(361.168269770952,242.158047317181,536.643200551891));
#59466=CARTESIAN_POINT('',(361.168269770952,242.158047317181,534.855040551891));
#59467=CARTESIAN_POINT('Origin',(361.168269770952,243.706639303213,534.837158951891));
#59468=CARTESIAN_POINT('',(361.168269770952,245.255231289244,536.643200551891));
#59469=CARTESIAN_POINT('Origin',(363.850509770952,243.706639303213,536.344095603207));
#59470=CARTESIAN_POINT('Origin',(363.850509770952,243.706639303213,536.643200551891));
#59471=CARTESIAN_POINT('Origin',(371.134539285592,242.661954434742,536.643200551891));
#59472=CARTESIAN_POINT('Origin',(268.509394890955,192.583144903205,411.559688530939));
#59473=CARTESIAN_POINT('',(269.850514890955,192.118223303205,410.785392537923));
#59474=CARTESIAN_POINT('',(269.850514890955,192.565263303205,410.785392537923));
#59475=CARTESIAN_POINT('',(269.850514890955,192.118223303205,410.785392537923));
#59476=CARTESIAN_POINT('Origin',(269.850514890955,192.341743303205,407.670326965861));
#59477=CARTESIAN_POINT('',(269.850514890955,192.118223303205,407.688208565861));
#59478=CARTESIAN_POINT('',(269.850514890955,192.565263303205,407.688208565861));
#59479=CARTESIAN_POINT('',(269.850514890955,192.118223303205,410.785392537923));
#59480=CARTESIAN_POINT('Origin',(268.509394890955,192.583144903205,406.913912572845));
#59481=CARTESIAN_POINT('',(267.168274890955,192.118223303205,406.139616579829));
#59482=CARTESIAN_POINT('Origin',(272.628588001728,192.118223303206,409.236800551892));
#59483=CARTESIAN_POINT('',(264.005631237915,192.118223303203,404.807608089002));
#59484=CARTESIAN_POINT('Origin',(267.168274890955,192.118223303205,409.236800551892));
#59485=CARTESIAN_POINT('Origin',(267.168274890955,192.520559303204,409.236800551893));
#59486=CARTESIAN_POINT('',(263.779015582457,192.520559303203,404.490239310461));
#59487=CARTESIAN_POINT('Origin',(277.22667489095,274.105359303207,519.569153599969));
#59488=CARTESIAN_POINT('',(277.22667489095,274.105359303207,519.410526160866));
#59489=CARTESIAN_POINT('',(275.630074508445,276.341352717653,520.996800551891));
#59490=CARTESIAN_POINT('',(277.067014852699,274.328958644651,519.569153599969));
#59491=CARTESIAN_POINT('',(277.22667489095,271.357851463207,520.996800551891));
#59492=CARTESIAN_POINT('Origin',(277.22667489095,274.105359303207,520.996800551891));
#59493=CARTESIAN_POINT('Origin',(277.22667489095,274.105359303207,520.996800551891));
#59494=CARTESIAN_POINT('Origin',(277.22667489095,274.105359303207,529.634954471891));
#59495=CARTESIAN_POINT('',(277.22667489095,271.357851463207,538.273108391891));
#59496=CARTESIAN_POINT('',(277.22667489095,271.357851463207,529.634954471891));
#59497=CARTESIAN_POINT('',(275.630074508445,276.341352717653,538.273108391891));
#59498=CARTESIAN_POINT('Origin',(277.22667489095,274.105359303207,538.273108391891));
#59499=CARTESIAN_POINT('Origin',(277.22667489095,274.105359303207,538.273108391891));
#59500=CARTESIAN_POINT('Origin',(277.22667489095,274.105359303207,538.333637607891));
#59501=CARTESIAN_POINT('',(275.278334040188,276.833955236879,538.878400551891));
#59502=CARTESIAN_POINT('',(275.594900461619,276.390612969576,538.333637607891));
#59503=CARTESIAN_POINT('Origin',(277.22667489095,274.105359303207,538.878400551891));
#59504=CARTESIAN_POINT('Origin',(319.695474890954,220.46055930321,519.569153599969));
#59505=CARTESIAN_POINT('',(319.695474890954,220.46055930321,519.410526160867));
#59506=CARTESIAN_POINT('',(318.098874508449,222.696552717656,520.996800551892));
#59507=CARTESIAN_POINT('',(319.535814852703,220.684158644654,519.569153599969));
#59508=CARTESIAN_POINT('',(319.695474890954,217.71305146321,520.996800551892));
#59509=CARTESIAN_POINT('Origin',(319.695474890954,220.46055930321,520.996800551892));
#59510=CARTESIAN_POINT('Origin',(319.695474890954,220.46055930321,520.996800551892));
#59511=CARTESIAN_POINT('Origin',(319.695474890954,220.46055930321,529.634954471891));
#59512=CARTESIAN_POINT('',(319.695474890954,217.71305146321,538.273108391892));
#59513=CARTESIAN_POINT('',(319.695474890954,217.71305146321,529.634954471891));
#59514=CARTESIAN_POINT('',(318.098874508449,222.696552717656,538.273108391891));
#59515=CARTESIAN_POINT('Origin',(319.695474890954,220.46055930321,538.273108391891));
#59516=CARTESIAN_POINT('Origin',(319.695474890954,220.46055930321,538.273108391891));
#59517=CARTESIAN_POINT('Origin',(319.695474890954,220.46055930321,538.333637607891));
#59518=CARTESIAN_POINT('',(317.747134040191,223.189155236882,538.878400551892));
#59519=CARTESIAN_POINT('',(318.063700461623,222.745812969579,538.333637607891));
#59520=CARTESIAN_POINT('Origin',(319.695474890954,220.46055930321,538.878400551891));
#59521=CARTESIAN_POINT('Origin',(277.226674890954,220.460559303207,519.569153599969));
#59522=CARTESIAN_POINT('',(277.226674890954,220.460559303207,519.410526160867));
#59523=CARTESIAN_POINT('',(275.630074508449,222.696552717653,520.996800551892));
#59524=CARTESIAN_POINT('',(277.067014852703,220.684158644651,519.569153599969));
#59525=CARTESIAN_POINT('',(277.226674890954,217.713051463207,520.996800551892));
#59526=CARTESIAN_POINT('Origin',(277.226674890954,220.460559303207,520.996800551892));
#59527=CARTESIAN_POINT('Origin',(277.226674890954,220.460559303207,520.996800551892));
#59528=CARTESIAN_POINT('Origin',(277.226674890954,220.460559303207,529.634954471892));
#59529=CARTESIAN_POINT('',(277.226674890954,217.713051463207,538.273108391892));
#59530=CARTESIAN_POINT('',(277.226674890954,217.713051463207,529.634954471892));
#59531=CARTESIAN_POINT('',(275.630074508449,222.696552717653,538.273108391892));
#59532=CARTESIAN_POINT('Origin',(277.226674890954,220.460559303207,538.273108391892));
#59533=CARTESIAN_POINT('Origin',(277.226674890954,220.460559303207,538.273108391892));
#59534=CARTESIAN_POINT('Origin',(277.226674890954,220.460559303207,538.333637607892));
#59535=CARTESIAN_POINT('',(275.278334040191,223.189155236879,538.878400551892));
#59536=CARTESIAN_POINT('',(275.594900461623,222.745812969576,538.333637607892));
#59537=CARTESIAN_POINT('Origin',(277.226674890954,220.460559303207,538.878400551892));
#59538=CARTESIAN_POINT('Origin',(322.566620000615,174.23277875921,497.549298322234));
#59539=CARTESIAN_POINT('',(322.566620000615,174.30189114321,500.769774482234));
#59540=CARTESIAN_POINT('',(320.695173668762,174.30189114321,500.170205669723));
#59541=CARTESIAN_POINT('Origin',(322.566620000615,174.30189114321,497.549298322234));
#59542=CARTESIAN_POINT('Origin',(322.566620000615,174.30189114321,497.549298322234));
#59543=CARTESIAN_POINT('',(320.293555674725,173.610767303209,500.732660244851));
#59544=CARTESIAN_POINT('',(320.655011869359,174.23277875921,500.226451127236));
#59545=CARTESIAN_POINT('Origin',(322.566620000615,173.61076730321,497.549298322234));
#59546=CARTESIAN_POINT('Origin',(322.566620000614,184.59588122321,497.549298322234));
#59547=CARTESIAN_POINT('',(322.566620000613,194.88987130321,500.769774482234));
#59548=CARTESIAN_POINT('',(322.566620000614,184.59588122321,500.769774482234));
#59549=CARTESIAN_POINT('',(320.69517366876,194.889871303211,500.170205669724));
#59550=CARTESIAN_POINT('Origin',(322.566620000613,194.88987130321,497.549298322234));
#59551=CARTESIAN_POINT('Origin',(322.566620000613,194.88987130321,497.549298322234));
#59552=CARTESIAN_POINT('Origin',(322.566620000613,196.563279803317,497.549298322234));
#59553=CARTESIAN_POINT('',(322.566620000613,196.749214081107,497.549298322234));
#59554=CARTESIAN_POINT('',(322.379475367428,196.563279803317,497.811389056983));
#59555=CARTESIAN_POINT('Origin',(427.665215541298,174.232778759216,392.450702781549));
#59556=CARTESIAN_POINT('',(427.665215541298,174.301891143216,395.671178941549));
#59557=CARTESIAN_POINT('',(425.793769209446,174.301891143216,395.071610129039));
#59558=CARTESIAN_POINT('Origin',(427.665215541298,174.301891143216,392.450702781549));
#59559=CARTESIAN_POINT('Origin',(427.665215541298,174.301891143216,392.450702781549));
#59560=CARTESIAN_POINT('',(425.392151215409,173.610767303216,395.634064704167));
#59561=CARTESIAN_POINT('',(425.753607410043,174.232778759216,395.127855586552));
#59562=CARTESIAN_POINT('Origin',(427.665215541298,173.610767303216,392.450702781549));
#59563=CARTESIAN_POINT('Origin',(427.665215541298,184.595881223216,392.450702781549));
#59564=CARTESIAN_POINT('',(427.665215541297,194.889871303216,395.671178941549));
#59565=CARTESIAN_POINT('',(427.665215541298,184.595881223216,395.671178941549));
#59566=CARTESIAN_POINT('',(425.793769209445,194.889871303216,395.071610129039));
#59567=CARTESIAN_POINT('Origin',(427.665215541297,194.889871303216,392.450702781549));
#59568=CARTESIAN_POINT('Origin',(427.665215541297,194.889871303216,392.450702781549));
#59569=CARTESIAN_POINT('Origin',(427.665215541297,196.563279803322,392.450702781549));
#59570=CARTESIAN_POINT('',(427.665215541297,196.749214081111,392.450702781549));
#59571=CARTESIAN_POINT('',(427.478070908112,196.563279803322,392.712793516298));
#59572=CARTESIAN_POINT('Origin',(427.665215541299,174.232778759217,497.549298322234));
#59573=CARTESIAN_POINT('',(427.665215541299,174.301891143217,500.769774482234));
#59574=CARTESIAN_POINT('',(425.793769209447,174.301891143217,500.170205669723));
#59575=CARTESIAN_POINT('Origin',(427.665215541299,174.301891143217,497.549298322234));
#59576=CARTESIAN_POINT('Origin',(427.665215541299,174.301891143217,497.549298322234));
#59577=CARTESIAN_POINT('',(425.392151215409,173.610767303217,500.732660244851));
#59578=CARTESIAN_POINT('',(425.753607410043,174.232778759217,500.226451127236));
#59579=CARTESIAN_POINT('Origin',(427.665215541299,173.610767303217,497.549298322234));
#59580=CARTESIAN_POINT('Origin',(427.665215541298,184.595881223217,497.549298322234));
#59581=CARTESIAN_POINT('',(427.665215541297,194.889871303217,500.769774482233));
#59582=CARTESIAN_POINT('',(427.665215541298,184.595881223217,500.769774482234));
#59583=CARTESIAN_POINT('',(425.793769209445,194.889871303218,500.170205669724));
#59584=CARTESIAN_POINT('Origin',(427.665215541297,194.889871303217,497.549298322233));
#59585=CARTESIAN_POINT('Origin',(427.665215541297,194.889871303217,497.549298322233));
#59586=CARTESIAN_POINT('Origin',(427.665215541297,196.563279803324,497.549298322233));
#59587=CARTESIAN_POINT('',(427.665215541297,196.749214081114,497.549298322233));
#59588=CARTESIAN_POINT('',(427.478070908112,196.563279803324,497.811389056982));
#59589=CARTESIAN_POINT('Origin',(322.566620000614,174.232778759209,392.45070278155));
#59590=CARTESIAN_POINT('',(322.566620000614,174.301891143209,395.67117894155));
#59591=CARTESIAN_POINT('',(320.695173668762,174.301891143209,395.071610129039));
#59592=CARTESIAN_POINT('Origin',(322.566620000614,174.301891143209,392.45070278155));
#59593=CARTESIAN_POINT('Origin',(322.566620000614,174.301891143209,392.45070278155));
#59594=CARTESIAN_POINT('',(320.293555674725,173.610767303209,395.634064704167));
#59595=CARTESIAN_POINT('',(320.655011869358,174.232778759209,395.127855586552));
#59596=CARTESIAN_POINT('Origin',(322.566620000614,173.610767303209,392.45070278155));
#59597=CARTESIAN_POINT('Origin',(322.566620000614,184.595881223209,392.45070278155));
#59598=CARTESIAN_POINT('',(322.566620000613,194.889871303209,395.67117894155));
#59599=CARTESIAN_POINT('',(322.566620000614,184.595881223209,395.67117894155));
#59600=CARTESIAN_POINT('',(320.695173668761,194.889871303209,395.071610129039));
#59601=CARTESIAN_POINT('Origin',(322.566620000613,194.889871303209,392.45070278155));
#59602=CARTESIAN_POINT('Origin',(322.566620000613,194.889871303209,392.45070278155));
#59603=CARTESIAN_POINT('Origin',(322.566620000613,196.563279803315,392.45070278155));
#59604=CARTESIAN_POINT('',(322.566620000613,196.749214081104,392.45070278155));
#59605=CARTESIAN_POINT('',(322.379475367428,196.563279803315,392.712793516299));
#59606=CARTESIAN_POINT('Origin',(428.603096951416,291.986959303217,520.996800551891));
#59607=CARTESIAN_POINT('',(428.331267438134,291.986959303217,520.996800551891));
#59608=CARTESIAN_POINT('',(428.603096951416,292.370126934863,521.270399563094));
#59609=CARTESIAN_POINT('Origin',(428.603096951415,291.986959303216,369.003200551891));
#59610=CARTESIAN_POINT('',(428.331267438134,291.986959303216,369.003200551891));
#59611=CARTESIAN_POINT('',(428.603096951415,292.370126934862,369.276799563094));
#59612=CARTESIAN_POINT('Origin',(276.942620190481,291.986959303207,520.996800551891));
#59613=CARTESIAN_POINT('',(277.214449703762,291.986959303207,520.996800551891));
#59614=CARTESIAN_POINT('',(276.942620190481,291.603791671561,521.270399563094));
#59615=CARTESIAN_POINT('Origin',(276.94262019048,291.986959303205,369.003200551891));
#59616=CARTESIAN_POINT('',(277.214449703761,291.986959303206,369.003200551891));
#59617=CARTESIAN_POINT('',(276.94262019048,291.60379167156,369.276799563094));
#59618=CARTESIAN_POINT('Origin',(276.942620190486,202.578959303206,369.003200551892));
#59619=CARTESIAN_POINT('',(277.214449703768,202.578959303206,369.003200551892));
#59620=CARTESIAN_POINT('',(276.942620190486,202.19579167156,369.276799563095));
#59621=CARTESIAN_POINT('Origin',(276.942620190487,202.578959303207,520.996800551892));
#59622=CARTESIAN_POINT('',(277.214449703768,202.578959303207,520.996800551892));
#59623=CARTESIAN_POINT('',(276.942620190487,202.195791671561,521.270399563095));
#59624=CARTESIAN_POINT('Origin',(428.603096951421,202.578959303216,369.003200551891));
#59625=CARTESIAN_POINT('',(428.33126743814,202.578959303216,369.003200551891));
#59626=CARTESIAN_POINT('',(428.603096951421,202.962126934862,369.276799563094));
#59627=CARTESIAN_POINT('Origin',(428.603096951422,202.578959303217,520.996800551891));
#59628=CARTESIAN_POINT('',(428.33126743814,202.578959303217,520.996800551891));
#59629=CARTESIAN_POINT('',(428.603096951422,202.962126934863,521.270399563094));
#59630=CARTESIAN_POINT('Origin',(330.231058744534,208.032452402338,535.164131149611));
#59631=CARTESIAN_POINT('',(327.592975586647,205.44001530321,538.878400551892));
#59632=CARTESIAN_POINT('',(327.592975586647,205.44001530321,538.878400551892));
#59633=CARTESIAN_POINT('',(332.869141902422,210.624889501466,538.878400551892));
#59634=CARTESIAN_POINT('',(332.869141902422,210.624889501466,538.878400551892));
#59635=CARTESIAN_POINT('',(327.592975586647,205.44001530321,538.878400551892));
#59636=CARTESIAN_POINT('Origin',(333.189076396687,228.953924402338,535.345190946332));
#59637=CARTESIAN_POINT('',(333.509010890952,247.282959303211,538.878400551891));
#59638=CARTESIAN_POINT('',(333.509010890952,247.282959303211,538.878400551891));
#59639=CARTESIAN_POINT('',(332.869141902422,210.624889501466,538.878400551892));
#59640=CARTESIAN_POINT('Origin',(263.733073385219,228.953924402334,535.345190946332));
#59641=CARTESIAN_POINT('',(263.413138890952,247.282959303206,538.878400551891));
#59642=CARTESIAN_POINT('',(263.413138890952,247.282959303206,538.878400551891));
#59643=CARTESIAN_POINT('',(264.053007879487,210.624889501461,538.878400551892));
#59644=CARTESIAN_POINT('',(264.053007879487,210.624889501461,538.878400551892));
#59645=CARTESIAN_POINT('',(263.413138890952,247.282959303206,538.878400551891));
#59646=CARTESIAN_POINT('Origin',(333.189076396684,265.611994204083,535.345190946332));
#59647=CARTESIAN_POINT('',(332.869141902417,283.941029104955,538.878400551891));
#59648=CARTESIAN_POINT('',(332.869141902417,283.941029104955,538.878400551891));
#59649=CARTESIAN_POINT('',(333.509010890952,247.282959303211,538.878400551891));
#59650=CARTESIAN_POINT('Origin',(330.231058744529,286.533466204083,535.164131149611));
#59651=CARTESIAN_POINT('',(327.592975586641,289.12590330321,538.878400551891));
#59652=CARTESIAN_POINT('',(327.592975586641,289.12590330321,538.878400551891));
#59653=CARTESIAN_POINT('',(332.869141902417,283.941029104955,538.878400551891));
#59654=CARTESIAN_POINT('Origin',(327.610857186641,289.12590330321,537.030206650751));
#59655=CARTESIAN_POINT('',(269.329174195257,289.125903303206,538.878400551891));
#59656=CARTESIAN_POINT('',(269.329174195257,289.125903303206,538.878400551891));
#59657=CARTESIAN_POINT('',(327.592975586641,289.12590330321,538.878400551891));
#59658=CARTESIAN_POINT('Origin',(266.691091037369,286.533466204079,535.164131149611));
#59659=CARTESIAN_POINT('',(264.053007879482,283.941029104951,538.878400551891));
#59660=CARTESIAN_POINT('',(264.053007879482,283.941029104951,538.878400551891));
#59661=CARTESIAN_POINT('',(269.329174195257,289.125903303206,538.878400551891));
#59662=CARTESIAN_POINT('Origin',(263.733073385216,265.611994204078,535.345190946332));
#59663=CARTESIAN_POINT('',(264.053007879482,283.941029104951,538.878400551891));
#59664=CARTESIAN_POINT('Origin',(333.526892490952,247.282959303211,538.878400551891));
#59665=CARTESIAN_POINT('',(269.329174195263,205.440015303206,538.878400551892));
#59666=CARTESIAN_POINT('',(264.053007879487,210.624889501461,538.878400551892));
#59667=CARTESIAN_POINT('',(269.329174195263,205.440015303206,538.878400551892));
#59668=CARTESIAN_POINT('',(280.579474890949,288.053007303207,538.878400551891));
#59669=CARTESIAN_POINT('',(316.342674890949,288.053007303209,538.878400551891));
#59670=CARTESIAN_POINT('',(280.579474890949,288.053007303207,538.878400551891));
#59671=CARTESIAN_POINT('',(329.75387489095,274.64180730321,538.878400551891));
#59672=CARTESIAN_POINT('',(316.342674890949,288.053007303209,538.878400551891));
#59673=CARTESIAN_POINT('',(329.753874890953,219.92411130321,538.878400551892));
#59674=CARTESIAN_POINT('',(329.75387489095,274.64180730321,538.878400551891));
#59675=CARTESIAN_POINT('',(316.342674890955,206.512911303209,538.878400551892));
#59676=CARTESIAN_POINT('',(329.753874890953,219.92411130321,538.878400551891));
#59677=CARTESIAN_POINT('',(280.579474890954,206.512911303207,538.878400551892));
#59678=CARTESIAN_POINT('',(316.342674890955,206.512911303209,538.878400551892));
#59679=CARTESIAN_POINT('',(267.168274890954,219.924111303206,538.878400551892));
#59680=CARTESIAN_POINT('',(280.579474890954,206.512911303207,538.878400551892));
#59681=CARTESIAN_POINT('',(267.16827489095,274.641807303206,538.878400551891));
#59682=CARTESIAN_POINT('',(267.168274890954,219.924111303206,538.878400551892));
#59683=CARTESIAN_POINT('',(267.16827489095,274.641807303206,538.878400551891));
#59684=CARTESIAN_POINT('Origin',(442.189799370956,184.429135303217,445.000000551891));
#59685=CARTESIAN_POINT('',(375.115917770956,184.429135303212,377.944000551892));
#59686=CARTESIAN_POINT('Origin',(375.115917770956,184.429135303213,445.000000551892));
#59687=CARTESIAN_POINT('',(375.115917770956,184.429135303212,398.051859751892));
#59688=CARTESIAN_POINT('Origin',(375.115917770956,184.429135303213,445.000000551892));
#59689=CARTESIAN_POINT('Origin',(375.115917770956,183.937391303213,445.000000551892));
#59690=CARTESIAN_POINT('',(375.115917770956,183.445647303212,398.051859751892));
#59691=CARTESIAN_POINT('',(375.115917770956,183.937391303212,398.051859751892));
#59692=CARTESIAN_POINT('Origin',(375.115917770956,183.445647303212,445.000000551892));
#59693=CARTESIAN_POINT('Origin',(375.115917770956,174.415439303212,445.000000551892));
#59694=CARTESIAN_POINT('',(375.115917770957,174.504847303213,491.948141351892));
#59695=CARTESIAN_POINT('',(347.833950284685,174.504847303212,483.207619879123));
#59696=CARTESIAN_POINT('Origin',(375.115917770956,174.504847303213,445.000000551892));
#59697=CARTESIAN_POINT('',(347.533983587441,173.610767303209,483.627714704941));
#59698=CARTESIAN_POINT('',(347.80395361496,174.41543930321,483.249629361705));
#59699=CARTESIAN_POINT('Origin',(375.115917770956,173.610767303213,445.000000551892));
#59700=CARTESIAN_POINT('Origin',(375.115917770956,174.504847303213,445.000000551892));
#59701=CARTESIAN_POINT('Origin',(271.071258570951,247.282959303205,330.553791757734));
#59702=CARTESIAN_POINT('Origin',(313.603213770946,320.847861703208,383.487296551891));
#59703=CARTESIAN_POINT('',(303.589517770946,320.829980103207,393.500992551891));
#59704=CARTESIAN_POINT('Origin',(436.628621770955,192.583144903216,383.487296551891));
#59705=CARTESIAN_POINT('',(446.642317770956,173.610767303217,393.500992551891));
#59706=CARTESIAN_POINT('',(446.642317770956,173.610767303217,393.500992551891));
#59707=CARTESIAN_POINT('',(426.614925770956,173.610767303216,373.473600551892));
#59708=CARTESIAN_POINT('Origin',(446.642317770956,183.088015303217,393.483110951891));
#59709=CARTESIAN_POINT('',(446.642317770957,173.610767303218,496.499008551892));
#59710=CARTESIAN_POINT('',(446.642317770957,173.610767303218,496.499008551892));
#59711=CARTESIAN_POINT('',(446.642317770956,173.610767303217,393.500992551891));
#59712=CARTESIAN_POINT('Origin',(436.628621770955,192.583144903217,506.512704551891));
#59713=CARTESIAN_POINT('',(426.614925770957,173.610767303217,516.526400551892));
#59714=CARTESIAN_POINT('',(426.614925770957,173.610767303217,516.526400551892));
#59715=CARTESIAN_POINT('',(446.642317770957,173.610767303218,496.499008551892));
#59716=CARTESIAN_POINT('Origin',(426.632807370956,183.088015303217,516.526400551892));
#59717=CARTESIAN_POINT('',(323.616909770957,173.61076730321,516.526400551892));
#59718=CARTESIAN_POINT('',(323.616909770957,173.61076730321,516.526400551892));
#59719=CARTESIAN_POINT('',(426.614925770957,173.610767303217,516.526400551892));
#59720=CARTESIAN_POINT('Origin',(313.603213770955,192.583144903209,506.512704551892));
#59721=CARTESIAN_POINT('',(303.589517770957,173.610767303208,496.499008551892));
#59722=CARTESIAN_POINT('',(303.589517770957,173.610767303208,496.499008551892));
#59723=CARTESIAN_POINT('',(323.616909770957,173.61076730321,516.526400551892));
#59724=CARTESIAN_POINT('Origin',(303.589517770956,183.088015303207,393.483110951892));
#59725=CARTESIAN_POINT('',(303.589517770957,173.610767303208,496.499008551892));
#59726=CARTESIAN_POINT('Origin',(446.660199370957,173.610767303218,445.000000551892));
#59727=CARTESIAN_POINT('Origin',(327.610857186647,205.44001530321,537.030206650751));
#59728=CARTESIAN_POINT('',(269.329174195263,205.440015303206,538.878400551892));
#59729=CARTESIAN_POINT('Origin',(266.691091037374,208.032452402334,535.164131149612));
#59730=CARTESIAN_POINT('Origin',(317.611309698624,205.871791230878,335.477394119332));
#59731=CARTESIAN_POINT('Origin',(375.115917770952,313.069365703204,445.000000551892));
#59732=CARTESIAN_POINT('',(375.115917770947,312.962076103212,377.94400055189));
#59733=CARTESIAN_POINT('',(336.149100755717,312.962076103188,390.428081878454));
#59734=CARTESIAN_POINT('Origin',(375.115917770947,312.962076103213,445.00000055189));
#59735=CARTESIAN_POINT('Origin',(375.115917770947,312.962076103213,445.00000055189));
#59736=CARTESIAN_POINT('',(335.789140719017,314.034972103212,389.923968087461));
#59737=CARTESIAN_POINT('',(336.113104752046,313.069365703191,390.377670499354));
#59738=CARTESIAN_POINT('Origin',(375.115917770947,314.034972103213,445.00000055189));
#59739=CARTESIAN_POINT('Origin',(359.022477770951,247.282959303211,363.526482809593));
#59740=CARTESIAN_POINT('',(359.022477770953,217.089877703211,379.903853776783));
#59741=CARTESIAN_POINT('',(359.022477770953,217.089877703211,363.526482809593));
#59742=CARTESIAN_POINT('',(375.115917770953,221.736465111823,377.944000551891));
#59743=CARTESIAN_POINT('Ctrl Pts',(375.115917770953,221.736465111823,377.944000551891));
#59744=CARTESIAN_POINT('Ctrl Pts',(373.636790201116,220.804664034964,377.944000551891));
#59745=CARTESIAN_POINT('Ctrl Pts',(372.061821595824,219.993987408909,377.993721471897));
#59746=CARTESIAN_POINT('Ctrl Pts',(368.577472050991,218.571521074051,378.23758179025));
#59747=CARTESIAN_POINT('Ctrl Pts',(366.648020923175,218.002843790601,378.452212963473));
#59748=CARTESIAN_POINT('Ctrl Pts',(362.793307997576,217.262051385977,379.057096473175));
#59749=CARTESIAN_POINT('Ctrl Pts',(360.86809223922,217.089877703211,379.447570460802));
#59750=CARTESIAN_POINT('Ctrl Pts',(359.022477770953,217.089877703211,379.903853776783));
#59751=CARTESIAN_POINT('',(375.115917770927,272.829453494629,377.944000551891));
#59752=CARTESIAN_POINT('Ctrl Pts',(375.115917770905,272.829453494629,377.944000551891));
#59753=CARTESIAN_POINT('Ctrl Pts',(375.324314296131,272.698170628581,377.944000551891));
#59754=CARTESIAN_POINT('Ctrl Pts',(375.530826414793,272.564512070292,377.944972249753));
#59755=CARTESIAN_POINT('Ctrl Pts',(377.391519391247,271.327814419871,377.962161223403));
#59756=CARTESIAN_POINT('Ctrl Pts',(378.915731826797,270.075157816713,378.03807646561));
#59757=CARTESIAN_POINT('Ctrl Pts',(381.621934327401,267.395986355681,378.246486242121));
#59758=CARTESIAN_POINT('Ctrl Pts',(382.893971040304,265.877729518232,378.387027646642));
#59759=CARTESIAN_POINT('Ctrl Pts',(385.135941372981,262.570231420126,378.687215969435));
#59760=CARTESIAN_POINT('Ctrl Pts',(386.106062898885,260.781039831472,378.84600614933));
#59761=CARTESIAN_POINT('Ctrl Pts',(387.665333692241,257.045413463659,379.124007415217));
#59762=CARTESIAN_POINT('Ctrl Pts',(388.255709793393,255.095882880109,379.24279855252));
#59763=CARTESIAN_POINT('Ctrl Pts',(389.030925142045,251.170981356928,379.402467677427));
#59764=CARTESIAN_POINT('Ctrl Pts',(389.215559370951,249.195559926263,379.44309974998));
#59765=CARTESIAN_POINT('Ctrl Pts',(389.215559370951,245.370358680163,379.44309974998));
#59766=CARTESIAN_POINT('Ctrl Pts',(389.030925142045,243.394937249498,379.402467677427));
#59767=CARTESIAN_POINT('Ctrl Pts',(388.255709793394,239.470035726317,379.24279855252));
#59768=CARTESIAN_POINT('Ctrl Pts',(387.665333692242,237.520505142767,379.124007415217));
#59769=CARTESIAN_POINT('Ctrl Pts',(386.106062898887,233.784878774954,378.84600614933));
#59770=CARTESIAN_POINT('Ctrl Pts',(385.135941372983,231.9956871863,378.687215969435));
#59771=CARTESIAN_POINT('Ctrl Pts',(382.893971040307,228.688189088194,378.387027646642));
#59772=CARTESIAN_POINT('Ctrl Pts',(381.621934327403,227.169932250744,378.246486242122));
#59773=CARTESIAN_POINT('Ctrl Pts',(378.9157318268,224.490760789712,378.038076465611));
#59774=CARTESIAN_POINT('Ctrl Pts',(377.39151939125,223.238104186553,377.962161223404));
#59775=CARTESIAN_POINT('Ctrl Pts',(375.530826414811,222.001406536142,377.944972249754));
#59776=CARTESIAN_POINT('Ctrl Pts',(375.324314296163,221.867747977862,377.944000551891));
#59777=CARTESIAN_POINT('Ctrl Pts',(375.115917770953,221.736465111823,377.944000551891));
#59778=CARTESIAN_POINT('Ctrl Pts',(359.022477770953,217.089877703211,379.903853776783));
#59779=CARTESIAN_POINT('Ctrl Pts',(356.987690988922,217.089877703211,380.406905349138));
#59780=CARTESIAN_POINT('Ctrl Pts',(354.919861382001,217.298453320156,381.021595941104));
#59781=CARTESIAN_POINT('Ctrl Pts',(350.868410694004,218.138264239459,382.444622280587));
#59782=CARTESIAN_POINT('Ctrl Pts',(348.884628885239,218.768978182231,383.252808054169));
#59783=CARTESIAN_POINT('Ctrl Pts',(345.124132814251,220.400640082137,384.989258968462));
#59784=CARTESIAN_POINT('Ctrl Pts',(343.344590306969,221.402426333465,385.918364292264));
#59785=CARTESIAN_POINT('Ctrl Pts',(340.077241909773,223.688973202756,387.795558540336));
#59786=CARTESIAN_POINT('Ctrl Pts',(338.5892495324,224.973941335523,388.743070052525));
#59787=CARTESIAN_POINT('Ctrl Pts',(336.046567394082,227.614002320155,390.481116463648));
#59788=CARTESIAN_POINT('Ctrl Pts',(334.878783177339,229.05453689296,391.341550794677));
#59789=CARTESIAN_POINT('Ctrl Pts',(332.79430570224,232.207271532133,392.969842155029));
#59790=CARTESIAN_POINT('Ctrl Pts',(331.877170850109,233.919572526647,393.73693833283));
#59791=CARTESIAN_POINT('Ctrl Pts',(330.379937606024,237.533474697026,395.038184711296));
#59792=CARTESIAN_POINT('Ctrl Pts',(329.798561481046,239.439070802072,395.572021113079));
#59793=CARTESIAN_POINT('Ctrl Pts',(329.023070644187,243.333346648986,396.294380977303));
#59794=CARTESIAN_POINT('Ctrl Pts',(328.829396170951,245.322412916721,396.481292261452));
#59795=CARTESIAN_POINT('Ctrl Pts',(328.829396170951,247.282959303209,396.481292261452));
#59796=CARTESIAN_POINT('Ctrl Pts',(328.829396170951,249.243505689698,396.481292261452));
#59797=CARTESIAN_POINT('Ctrl Pts',(329.023070644186,251.232571957432,396.294380977303));
#59798=CARTESIAN_POINT('Ctrl Pts',(329.798561481045,255.126847804347,395.572021113079));
#59799=CARTESIAN_POINT('Ctrl Pts',(330.379937606023,257.032443909393,395.038184711295));
#59800=CARTESIAN_POINT('Ctrl Pts',(331.877170850107,260.646346079772,393.73693833283));
#59801=CARTESIAN_POINT('Ctrl Pts',(332.794305702238,262.358647074286,392.969842155029));
#59802=CARTESIAN_POINT('Ctrl Pts',(334.878783177337,265.511381713459,391.341550794677));
#59803=CARTESIAN_POINT('Ctrl Pts',(336.046567394079,266.951916286264,390.481116463648));
#59804=CARTESIAN_POINT('Ctrl Pts',(338.589249532397,269.591977270897,388.743070052524));
#59805=CARTESIAN_POINT('Ctrl Pts',(340.07724190977,270.876945403664,387.795558540335));
#59806=CARTESIAN_POINT('Ctrl Pts',(343.344590306966,273.163492272956,385.918364292264));
#59807=CARTESIAN_POINT('Ctrl Pts',(345.124132814247,274.165278524283,384.989258968461));
#59808=CARTESIAN_POINT('Ctrl Pts',(348.884628885235,275.79694042419,383.252808054168));
#59809=CARTESIAN_POINT('Ctrl Pts',(350.868410694,276.427654366962,382.444622280586));
#59810=CARTESIAN_POINT('Ctrl Pts',(354.919861381997,277.267465286266,381.021595941103));
#59811=CARTESIAN_POINT('Ctrl Pts',(356.987690988918,277.476040903211,380.406905349137));
#59812=CARTESIAN_POINT('Ctrl Pts',(360.868092239216,277.476040903211,379.447570460801));
#59813=CARTESIAN_POINT('Ctrl Pts',(362.793307997572,277.303867220446,379.057096473175));
#59814=CARTESIAN_POINT('Ctrl Pts',(366.648020923171,276.563074815822,378.452212963473));
#59815=CARTESIAN_POINT('Ctrl Pts',(368.577472050987,275.994397532373,378.23758179025));
#59816=CARTESIAN_POINT('Ctrl Pts',(372.061821595804,274.571931197522,377.993721471898));
#59817=CARTESIAN_POINT('Ctrl Pts',(373.636790201081,273.761254571476,377.944000551891));
#59818=CARTESIAN_POINT('Ctrl Pts',(375.115917770905,272.829453494629,377.944000551891));
#59819=CARTESIAN_POINT('Origin',(298.461074890952,247.282959303209,538.073728551892));
#59820=CARTESIAN_POINT('',(281.384594574745,271.198084181898,538.878400551893));
#59821=CARTESIAN_POINT('',(281.654564602264,270.819998838662,538.073728551893));
#59822=CARTESIAN_POINT('Origin',(298.461074890952,247.282959303208,538.878400551891));
#59823=CARTESIAN_POINT('Origin',(375.115917770951,248.695605703213,445.000000551891));
#59824=CARTESIAN_POINT('',(375.115917770951,248.695605703212,377.944000551891));
#59825=CARTESIAN_POINT('',(375.115917770951,248.695605703212,377.944000551891));
#59826=CARTESIAN_POINT('Origin',(400.433645843278,288.694127375543,334.86186607715));
#59827=CARTESIAN_POINT('Origin',(400.433645843284,205.871791230884,334.86186607715));
#59828=CARTESIAN_POINT('Origin',(375.115917770948,301.607260103212,445.000000551891));
#59829=CARTESIAN_POINT('',(375.115917770949,292.219420103213,491.948141351891));
#59830=CARTESIAN_POINT('Origin',(375.115917770948,292.219420103212,445.000000551891));
#59831=CARTESIAN_POINT('',(375.115917770947,310.995100103213,491.948141351891));
#59832=CARTESIAN_POINT('',(375.115917770948,301.607260103213,491.948141351891));
#59833=CARTESIAN_POINT('Origin',(375.115917770947,310.995100103212,445.000000551891));
#59834=CARTESIAN_POINT('Origin',(375.115917770946,320.025308103214,445.00000055189));
#59835=CARTESIAN_POINT('',(347.833950284676,319.93590010321,406.792381224659));
#59836=CARTESIAN_POINT('',(375.115917770947,319.935900103213,491.94814135189));
#59837=CARTESIAN_POINT('Origin',(375.115917770947,319.935900103212,445.00000055189));
#59838=CARTESIAN_POINT('Origin',(375.115917770947,319.935900103212,445.00000055189));
#59839=CARTESIAN_POINT('',(347.533983587431,320.829980103214,406.37228639884));
#59840=CARTESIAN_POINT('',(347.80395361495,320.025308103214,406.750371742075));
#59841=CARTESIAN_POINT('Origin',(375.115917770947,320.829980103212,445.00000055189));
#59842=CARTESIAN_POINT('Origin',(446.660199370947,320.829980103217,445.00000055189));
#59843=CARTESIAN_POINT('',(430.89144884552,320.829980103216,386.862702781548));
#59844=CARTESIAN_POINT('',(434.117682149752,320.829980103216,392.450702781548));
#59845=CARTESIAN_POINT('',(430.89144884552,320.829980103216,386.862702781548));
#59846=CARTESIAN_POINT('',(430.89144884552,320.829980103216,398.038702781548));
#59847=CARTESIAN_POINT('',(434.117682149752,320.829980103216,392.450702781548));
#59848=CARTESIAN_POINT('',(424.438982237057,320.829980103215,398.038702781548));
#59849=CARTESIAN_POINT('',(430.89144884552,320.829980103216,398.038702781548));
#59850=CARTESIAN_POINT('',(421.212748932825,320.829980103215,392.450702781548));
#59851=CARTESIAN_POINT('',(424.438982237057,320.829980103215,398.038702781548));
#59852=CARTESIAN_POINT('',(424.438982237057,320.829980103215,386.862702781548));
#59853=CARTESIAN_POINT('',(421.212748932825,320.829980103215,392.450702781548));
#59854=CARTESIAN_POINT('',(424.438982237057,320.829980103215,386.862702781548));
#59855=CARTESIAN_POINT('',(325.792853304836,320.82998010321,491.961298322233));
#59856=CARTESIAN_POINT('',(329.019086609068,320.82998010321,497.549298322233));
#59857=CARTESIAN_POINT('',(325.792853304836,320.829980103209,491.961298322233));
#59858=CARTESIAN_POINT('',(325.792853304836,320.82998010321,503.137298322233));
#59859=CARTESIAN_POINT('',(329.019086609068,320.82998010321,497.549298322233));
#59860=CARTESIAN_POINT('',(319.340386696373,320.829980103209,503.137298322233));
#59861=CARTESIAN_POINT('',(325.792853304836,320.82998010321,503.137298322233));
#59862=CARTESIAN_POINT('',(316.114153392142,320.829980103209,497.549298322233));
#59863=CARTESIAN_POINT('',(319.340386696373,320.829980103209,503.137298322233));
#59864=CARTESIAN_POINT('',(319.340386696373,320.829980103209,491.961298322233));
#59865=CARTESIAN_POINT('',(316.114153392142,320.829980103209,497.549298322233));
#59866=CARTESIAN_POINT('',(319.340386696373,320.829980103209,491.961298322233));
#59867=CARTESIAN_POINT('Origin',(442.162976970949,292.219420103217,445.000000551891));
#59868=CARTESIAN_POINT('',(375.115917770949,292.219420103213,512.029178151891));
#59869=CARTESIAN_POINT('Origin',(375.115917770948,292.219420103212,445.000000551891));
#59870=CARTESIAN_POINT('Origin',(375.115917770948,303.127196103212,445.000000551891));
#59871=CARTESIAN_POINT('',(375.115917770947,314.034972103213,512.029178151891));
#59872=CARTESIAN_POINT('Origin',(375.115917770947,314.034972103212,445.000000551891));
#59873=CARTESIAN_POINT('',(375.115917770948,303.127196103213,512.029178151891));
#59874=CARTESIAN_POINT('Origin',(442.80923616536,314.034972103217,445.00000055189));
#59875=CARTESIAN_POINT('Origin',(392.118190090946,325.425551303214,445.00000055189));
#59876=CARTESIAN_POINT('',(392.595628810946,325.425551303214,442.25249271189));
#59877=CARTESIAN_POINT('',(392.595628810946,327.022151685719,442.764007137444));
#59878=CARTESIAN_POINT('Origin',(392.595628810946,325.425551303214,445.00000055189));
#59879=CARTESIAN_POINT('Origin',(392.595628810946,325.425551303214,445.00000055189));
#59880=CARTESIAN_POINT('',(391.640751370946,325.425551303214,442.25249271189));
#59881=CARTESIAN_POINT('',(392.118190090946,325.425551303214,442.25249271189));
#59882=CARTESIAN_POINT('Origin',(391.640751370946,325.425551303214,445.00000055189));
#59883=CARTESIAN_POINT('Origin',(375.115917770946,331.254952903213,445.00000055189));
#59884=CARTESIAN_POINT('',(353.03991703791,331.147663303211,475.916811544351));
#59885=CARTESIAN_POINT('',(375.115917770946,331.147663303212,407.01054135189));
#59886=CARTESIAN_POINT('Origin',(375.115917770946,331.147663303213,445.00000055189));
#59887=CARTESIAN_POINT('Origin',(375.115917770946,331.147663303213,445.00000055189));
#59888=CARTESIAN_POINT('',(353.399877074602,332.220559303212,475.41269775337));
#59889=CARTESIAN_POINT('',(353.075913041579,331.254952903211,475.866400165253));
#59890=CARTESIAN_POINT('Origin',(375.115917770946,332.220559303213,445.00000055189));
#59891=CARTESIAN_POINT('Origin',(412.503821776533,332.220559303215,445.00000055189));
#59892=CARTESIAN_POINT('',(391.640751370946,332.220559303214,448.36174135189));
#59893=CARTESIAN_POINT('',(391.640751370946,332.220559303214,441.63825975189));
#59894=CARTESIAN_POINT('',(391.640751370946,332.220559303214,448.36174135189));
#59895=CARTESIAN_POINT('',(389.391142518186,332.220559303214,448.36174135189));
#59896=CARTESIAN_POINT('',(391.640751370946,332.220559303214,448.36174135189));
#59897=CARTESIAN_POINT('',(389.391142518186,332.220559303214,441.63825975189));
#59898=CARTESIAN_POINT('Origin',(375.115917770946,332.220559303213,445.00000055189));
#59899=CARTESIAN_POINT('',(391.640751370946,332.220559303214,441.63825975189));
#59900=CARTESIAN_POINT('Origin',(375.115917770946,330.289346503213,445.00000055189));
#59901=CARTESIAN_POINT('',(388.115106324191,330.074767303214,441.63825975189));
#59902=CARTESIAN_POINT('',(388.115106324191,330.074767303214,448.36174135189));
#59903=CARTESIAN_POINT('Origin',(375.115917770946,330.074767303213,445.00000055189));
#59904=CARTESIAN_POINT('Ctrl Pts',(388.115106324191,330.074767303214,441.63825975189));
#59905=CARTESIAN_POINT('Ctrl Pts',(388.541335653371,330.789504164161,441.63825975189));
#59906=CARTESIAN_POINT('Ctrl Pts',(388.966604868582,331.504817465291,441.63825975189));
#59907=CARTESIAN_POINT('Ctrl Pts',(389.391142518186,332.220559303214,441.63825975189));
#59908=CARTESIAN_POINT('Ctrl Pts',(389.391142518186,332.220559303214,448.36174135189));
#59909=CARTESIAN_POINT('Ctrl Pts',(388.966603199871,331.504814651955,448.36174135189));
#59910=CARTESIAN_POINT('Ctrl Pts',(388.54133083666,330.789496087098,448.36174135189));
#59911=CARTESIAN_POINT('Ctrl Pts',(388.115106324191,330.074767303214,448.36174135189));
#59912=CARTESIAN_POINT('Origin',(403.843567738701,147.345359303214,445.000000551892));
#59913=CARTESIAN_POINT('',(358.432425010641,147.345359303211,421.635243565227));
#59914=CARTESIAN_POINT('Origin',(375.115917770958,147.345359303212,445.000000551892));
#59915=CARTESIAN_POINT('Origin',(375.115917770951,247.282959303213,445.000000551891));
#59916=CARTESIAN_POINT('',(388.115106324202,164.491151303213,448.361741351892));
#59917=CARTESIAN_POINT('',(388.115106324191,330.074767303214,448.36174135189));
#59918=CARTESIAN_POINT('',(388.115106324202,164.491151303213,441.638259751892));
#59919=CARTESIAN_POINT('Origin',(375.115917770957,164.491151303213,445.000000551892));
#59920=CARTESIAN_POINT('',(388.115106324202,164.491151303213,441.638259751892));
#59921=CARTESIAN_POINT('',(370.923963348087,169.140367303212,457.755694275315));
#59922=CARTESIAN_POINT('Ctrl Pts',(370.923963348087,169.140367303212,457.755694275315));
#59923=CARTESIAN_POINT('Ctrl Pts',(370.923963348087,169.48641478499,457.755694275315));
#59924=CARTESIAN_POINT('Ctrl Pts',(370.856354814583,169.854836977962,457.734079023222));
#59925=CARTESIAN_POINT('Ctrl Pts',(370.586255285233,170.531462911025,457.640522237506));
#59926=CARTESIAN_POINT('Ctrl Pts',(370.384223692787,170.839753936057,457.567887535573));
#59927=CARTESIAN_POINT('Ctrl Pts',(369.927073334233,171.326528548091,457.386145959219));
#59928=CARTESIAN_POINT('Ctrl Pts',(369.641199463923,171.537822113727,457.264699280901));
#59929=CARTESIAN_POINT('Ctrl Pts',(369.02859564363,171.818522071294,456.972464156601));
#59930=CARTESIAN_POINT('Ctrl Pts',(368.702162046036,171.887875143212,456.801003724408));
#59931=CARTESIAN_POINT('Ctrl Pts',(368.102827095877,171.887875143212,456.454977529599));
#59932=CARTESIAN_POINT('Ctrl Pts',(367.791121207057,171.818522071294,456.258007957531));
#59933=CARTESIAN_POINT('Ctrl Pts',(367.231736255389,171.537822113727,455.873595048851));
#59934=CARTESIAN_POINT('Ctrl Pts',(366.983623411605,171.326528548091,455.686744354044));
#59935=CARTESIAN_POINT('Ctrl Pts',(366.597655410281,170.839753936057,455.381711318364));
#59936=CARTESIAN_POINT('Ctrl Pts',(366.433736116989,170.531462911025,455.243064177905));
#59937=CARTESIAN_POINT('Ctrl Pts',(366.217663799188,169.854836977962,455.055929516796));
#59938=CARTESIAN_POINT('Ctrl Pts',(366.165140175013,169.486414784989,455.008186435315));
#59939=CARTESIAN_POINT('Ctrl Pts',(366.165140175013,168.794319821435,455.008186435315));
#59940=CARTESIAN_POINT('Ctrl Pts',(366.217663799188,168.425897628462,455.055929516796));
#59941=CARTESIAN_POINT('Ctrl Pts',(366.433736116989,167.749271695399,455.243064177905));
#59942=CARTESIAN_POINT('Ctrl Pts',(366.597655410282,167.440980670367,455.381711318364));
#59943=CARTESIAN_POINT('Ctrl Pts',(366.983623411605,166.954206058333,455.686744354044));
#59944=CARTESIAN_POINT('Ctrl Pts',(367.231736255389,166.742912492697,455.873595048851));
#59945=CARTESIAN_POINT('Ctrl Pts',(367.791121207058,166.46221253513,456.258007957531));
#59946=CARTESIAN_POINT('Ctrl Pts',(368.102827095878,166.392859463212,456.454977529599));
#59947=CARTESIAN_POINT('Ctrl Pts',(368.702162046036,166.392859463212,456.801003724408));
#59948=CARTESIAN_POINT('Ctrl Pts',(369.02859564363,166.46221253513,456.972464156601));
#59949=CARTESIAN_POINT('Ctrl Pts',(369.641199463924,166.742912492697,457.264699280901));
#59950=CARTESIAN_POINT('Ctrl Pts',(369.927073334233,166.954206058333,457.386145959219));
#59951=CARTESIAN_POINT('Ctrl Pts',(370.384223692787,167.440980670368,457.567887535574));
#59952=CARTESIAN_POINT('Ctrl Pts',(370.586255285233,167.749271695399,457.640522237506));
#59953=CARTESIAN_POINT('Ctrl Pts',(370.856354814583,168.425897628462,457.734079023222));
#59954=CARTESIAN_POINT('Ctrl Pts',(370.923963348087,168.794319821435,457.755694275315));
#59955=CARTESIAN_POINT('Ctrl Pts',(370.923963348087,169.140367303212,457.755694275315));
#59956=CARTESIAN_POINT('',(366.165140175003,325.425551303212,434.991814668467));
#59957=CARTESIAN_POINT('Ctrl Pts',(366.165140175003,325.425551303212,434.991814668467));
#59958=CARTESIAN_POINT('Ctrl Pts',(366.165140175003,325.771598784989,434.991814668467));
#59959=CARTESIAN_POINT('Ctrl Pts',(366.217663799177,326.140020977962,434.944071586987));
#59960=CARTESIAN_POINT('Ctrl Pts',(366.433736116978,326.816646911025,434.756936925877));
#59961=CARTESIAN_POINT('Ctrl Pts',(366.597655410271,327.124937936057,434.618289785419));
#59962=CARTESIAN_POINT('Ctrl Pts',(366.983623411595,327.611712548091,434.313256749738));
#59963=CARTESIAN_POINT('Ctrl Pts',(367.231736255378,327.823006113727,434.126406054932));
#59964=CARTESIAN_POINT('Ctrl Pts',(367.791121207047,328.103706071295,433.741993146252));
#59965=CARTESIAN_POINT('Ctrl Pts',(368.102827095867,328.173059143212,433.545023574183));
#59966=CARTESIAN_POINT('Ctrl Pts',(368.702162046025,328.173059143212,433.198997379374));
#59967=CARTESIAN_POINT('Ctrl Pts',(369.028595643619,328.103706071295,433.027536947181));
#59968=CARTESIAN_POINT('Ctrl Pts',(369.641199463913,327.823006113727,432.735301822882));
#59969=CARTESIAN_POINT('Ctrl Pts',(369.927073334222,327.611712548091,432.613855144563));
#59970=CARTESIAN_POINT('Ctrl Pts',(370.384223692777,327.124937936057,432.432113568209));
#59971=CARTESIAN_POINT('Ctrl Pts',(370.586255285222,326.816646911026,432.359478866277));
#59972=CARTESIAN_POINT('Ctrl Pts',(370.856354814572,326.140020977963,432.265922080561));
#59973=CARTESIAN_POINT('Ctrl Pts',(370.923963348077,325.77159878499,432.244306828467));
#59974=CARTESIAN_POINT('Ctrl Pts',(370.923963348077,325.079503821435,432.244306828467));
#59975=CARTESIAN_POINT('Ctrl Pts',(370.856354814573,324.711081628462,432.265922080561));
#59976=CARTESIAN_POINT('Ctrl Pts',(370.586255285223,324.034455695399,432.359478866277));
#59977=CARTESIAN_POINT('Ctrl Pts',(370.384223692777,323.726164670368,432.432113568209));
#59978=CARTESIAN_POINT('Ctrl Pts',(369.927073334222,323.239390058333,432.613855144563));
#59979=CARTESIAN_POINT('Ctrl Pts',(369.641199463913,323.028096492698,432.735301822882));
#59980=CARTESIAN_POINT('Ctrl Pts',(369.028595643619,322.74739653513,433.027536947181));
#59981=CARTESIAN_POINT('Ctrl Pts',(368.702162046026,322.678043463212,433.198997379374));
#59982=CARTESIAN_POINT('Ctrl Pts',(368.102827095867,322.678043463212,433.545023574183));
#59983=CARTESIAN_POINT('Ctrl Pts',(367.791121207047,322.74739653513,433.741993146252));
#59984=CARTESIAN_POINT('Ctrl Pts',(367.231736255379,323.028096492697,434.126406054932));
#59985=CARTESIAN_POINT('Ctrl Pts',(366.983623411595,323.239390058333,434.313256749738));
#59986=CARTESIAN_POINT('Ctrl Pts',(366.597655410271,323.726164670367,434.618289785419));
#59987=CARTESIAN_POINT('Ctrl Pts',(366.433736116978,324.034455695399,434.756936925877));
#59988=CARTESIAN_POINT('Ctrl Pts',(366.217663799177,324.711081628462,434.944071586987));
#59989=CARTESIAN_POINT('Ctrl Pts',(366.165140175003,325.079503821435,434.991814668467));
#59990=CARTESIAN_POINT('Ctrl Pts',(366.165140175003,325.425551303212,434.991814668467));
#59991=CARTESIAN_POINT('Origin',(392.118190090957,169.140367303214,445.000000551892));
#59992=CARTESIAN_POINT('',(392.595628810957,169.140367303214,442.252492711892));
#59993=CARTESIAN_POINT('',(392.595628810957,170.736967685718,442.764007137445));
#59994=CARTESIAN_POINT('Origin',(392.595628810957,169.140367303214,445.000000551892));
#59995=CARTESIAN_POINT('Origin',(392.595628810957,169.140367303214,445.000000551892));
#59996=CARTESIAN_POINT('',(391.640751370957,169.140367303214,442.252492711892));
#59997=CARTESIAN_POINT('',(392.118190090957,169.140367303214,442.252492711892));
#59998=CARTESIAN_POINT('Origin',(391.640751370957,169.140367303214,445.000000551892));
#59999=CARTESIAN_POINT('Origin',(391.640751370957,162.327477703214,445.000000551892));
#60000=CARTESIAN_POINT('',(391.640751370946,332.220559303214,448.36174135189));
#60001=CARTESIAN_POINT('',(391.640751370946,332.220559303214,441.63825975189));
#60002=CARTESIAN_POINT('Origin',(356.121188170946,323.85907771718,412.100163808658));
#60003=CARTESIAN_POINT('',(357.282632160469,326.199847296226,411.429603808658));
#60004=CARTESIAN_POINT('',(357.28263216047,324.651255310195,411.429603808658));
#60005=CARTESIAN_POINT('',(357.282632160469,326.199847296226,411.429603808658));
#60006=CARTESIAN_POINT('',(356.121188170946,323.87695931718,412.100163808658));
#60007=CARTESIAN_POINT('',(357.28263216047,324.651255310195,411.429603808658));
#60008=CARTESIAN_POINT('',(354.959744181423,324.651255310195,412.770723808658));
#60009=CARTESIAN_POINT('',(356.121188170946,323.87695931718,412.100163808658));
#60010=CARTESIAN_POINT('',(354.959744181423,326.199847296226,412.770723808658));
#60011=CARTESIAN_POINT('',(354.959744181423,324.651255310195,412.770723808658));
#60012=CARTESIAN_POINT('',(356.121188170946,326.974143289242,412.100163808658));
#60013=CARTESIAN_POINT('',(354.959744181423,326.199847296226,412.770723808658));
#60014=CARTESIAN_POINT('',(356.121188170946,326.974143289242,412.100163808658));
#60015=CARTESIAN_POINT('Origin',(356.3929721424,326.416159246118,410.637994030892));
#60016=CARTESIAN_POINT('',(355.674148170946,326.974143289242,411.325867815642));
#60017=CARTESIAN_POINT('',(356.835592160469,326.199847296226,410.655307815642));
#60018=CARTESIAN_POINT('',(355.674148170946,326.974143289242,411.325867815642));
#60019=CARTESIAN_POINT('',(357.282632160469,326.199847296226,411.429603808658));
#60020=CARTESIAN_POINT('',(356.121188170946,326.974143289242,412.100163808658));
#60021=CARTESIAN_POINT('Origin',(355.231528152876,326.757831339351,411.308554030892));
#60022=CARTESIAN_POINT('',(354.512704181423,326.199847296226,411.996427815642));
#60023=CARTESIAN_POINT('',(354.512704181423,326.199847296226,411.996427815642));
#60024=CARTESIAN_POINT('',(354.959744181423,326.199847296226,412.770723808658));
#60025=CARTESIAN_POINT('Origin',(354.736224181423,324.633373710195,412.38357581215));
#60026=CARTESIAN_POINT('',(354.512704181423,324.651255310195,411.996427815642));
#60027=CARTESIAN_POINT('',(354.959744181423,324.651255310195,412.770723808658));
#60028=CARTESIAN_POINT('',(354.512704181423,326.199847296226,411.996427815642));
#60029=CARTESIAN_POINT('Origin',(355.231528152876,324.093271267072,411.308554030892));
#60030=CARTESIAN_POINT('',(355.674148170946,323.87695931718,411.325867815642));
#60031=CARTESIAN_POINT('',(355.674148170946,323.87695931718,411.325867815642));
#60032=CARTESIAN_POINT('',(356.121188170946,323.87695931718,412.100163808658));
#60033=CARTESIAN_POINT('Origin',(356.3929721424,324.434943360304,410.637994030892));
#60034=CARTESIAN_POINT('',(356.83559216047,324.651255310195,410.655307815642));
#60035=CARTESIAN_POINT('',(356.83559216047,324.651255310195,410.655307815642));
#60036=CARTESIAN_POINT('',(357.28263216047,324.651255310195,411.429603808658));
#60037=CARTESIAN_POINT('Origin',(357.05911216047,324.633373710195,411.04245581215));
#60038=CARTESIAN_POINT('',(356.835592160469,326.199847296226,410.655307815642));
#60039=CARTESIAN_POINT('Origin',(413.105376970946,323.859077717184,445.00000055189));
#60040=CARTESIAN_POINT('',(413.105376970946,326.19984729623,446.34112055189));
#60041=CARTESIAN_POINT('',(413.105376970946,324.651255310199,446.34112055189));
#60042=CARTESIAN_POINT('',(413.105376970946,326.19984729623,446.34112055189));
#60043=CARTESIAN_POINT('',(413.105376970946,323.876959317184,445.00000055189));
#60044=CARTESIAN_POINT('',(413.105376970946,324.651255310199,446.34112055189));
#60045=CARTESIAN_POINT('',(413.105376970946,324.651255310199,443.65888055189));
#60046=CARTESIAN_POINT('',(413.105376970946,323.876959317184,445.00000055189));
#60047=CARTESIAN_POINT('',(413.105376970946,326.19984729623,443.65888055189));
#60048=CARTESIAN_POINT('',(413.105376970946,324.651255310199,443.65888055189));
#60049=CARTESIAN_POINT('',(413.105376970946,326.974143289246,445.00000055189));
#60050=CARTESIAN_POINT('',(413.105376970946,326.19984729623,443.65888055189));
#60051=CARTESIAN_POINT('',(413.105376970946,326.974143289246,445.00000055189));
#60052=CARTESIAN_POINT('Origin',(414.017338570946,326.586995292738,445.67056055189));
#60053=CARTESIAN_POINT('',(413.999456970946,326.974143289246,445.00000055189));
#60054=CARTESIAN_POINT('',(413.999456970946,326.19984729623,446.34112055189));
#60055=CARTESIAN_POINT('',(413.999456970946,326.974143289246,445.00000055189));
#60056=CARTESIAN_POINT('',(413.105376970946,326.19984729623,446.34112055189));
#60057=CARTESIAN_POINT('',(413.105376970946,326.974143289246,445.00000055189));
#60058=CARTESIAN_POINT('Origin',(414.017338570946,326.586995292738,444.32944055189));
#60059=CARTESIAN_POINT('',(413.999456970946,326.19984729623,443.65888055189));
#60060=CARTESIAN_POINT('',(413.999456970946,326.19984729623,443.65888055189));
#60061=CARTESIAN_POINT('',(413.105376970946,326.19984729623,443.65888055189));
#60062=CARTESIAN_POINT('Origin',(414.017338570946,325.425551303215,443.65888055189));
#60063=CARTESIAN_POINT('',(413.999456970946,324.651255310199,443.65888055189));
#60064=CARTESIAN_POINT('',(413.105376970946,324.651255310199,443.65888055189));
#60065=CARTESIAN_POINT('',(413.999456970946,326.19984729623,443.65888055189));
#60066=CARTESIAN_POINT('Origin',(414.017338570946,324.264107313692,444.32944055189));
#60067=CARTESIAN_POINT('',(413.999456970946,323.876959317184,445.00000055189));
#60068=CARTESIAN_POINT('',(413.999456970946,323.876959317184,445.00000055189));
#60069=CARTESIAN_POINT('',(413.105376970946,323.876959317184,445.00000055189));
#60070=CARTESIAN_POINT('Origin',(414.017338570946,324.264107313692,445.67056055189));
#60071=CARTESIAN_POINT('',(413.999456970946,324.651255310199,446.34112055189));
#60072=CARTESIAN_POINT('',(413.999456970946,324.651255310199,446.34112055189));
#60073=CARTESIAN_POINT('',(413.105376970946,324.651255310199,446.34112055189));
#60074=CARTESIAN_POINT('Origin',(414.017338570946,325.425551303215,446.34112055189));
#60075=CARTESIAN_POINT('',(413.999456970946,326.19984729623,446.34112055189));
#60076=CARTESIAN_POINT('Origin',(355.674148170946,322.720959303211,411.325867815642));
#60077=CARTESIAN_POINT('',(357.567725598318,326.986821771622,410.232610378218));
#60078=CARTESIAN_POINT('Origin',(355.674148170946,325.425551303211,411.325867815642));
#60079=CARTESIAN_POINT('Origin',(355.973888490946,325.425551303211,411.845033278959));
#60080=CARTESIAN_POINT('',(358.370226366169,327.373892153973,410.538420363603));
#60081=CARTESIAN_POINT('',(353.103582997138,325.425551303211,413.579118330439));
#60082=CARTESIAN_POINT('Origin',(356.007192970946,325.425551303211,411.902718330439));
#60083=CARTESIAN_POINT('Origin',(356.007192970946,325.425551303211,411.902718330439));
#60084=CARTESIAN_POINT('',(358.289976289384,327.335185115738,410.507839365064));
#60085=CARTESIAN_POINT('Origin',(356.10125099401,325.425551303211,412.065631605245));
#60086=CARTESIAN_POINT('',(353.291699043265,325.425551303211,413.904944880051));
#60087=CARTESIAN_POINT('Ctrl Pts',(353.291699043265,325.425551303211,413.904944880051));
#60088=CARTESIAN_POINT('Ctrl Pts',(353.291699043265,325.004330608665,413.904944880051));
#60089=CARTESIAN_POINT('Ctrl Pts',(353.360762093389,324.555183834243,413.856113692485));
#60090=CARTESIAN_POINT('Ctrl Pts',(353.643146477605,323.729188378078,413.660750718005));
#60091=CARTESIAN_POINT('Ctrl Pts',(353.856660763807,323.352320991875,413.514577125536));
#60092=CARTESIAN_POINT('Ctrl Pts',(354.353438858032,322.757206995828,413.184794032729));
#60093=CARTESIAN_POINT('Ctrl Pts',(354.669916248831,322.499210926969,412.979213640235));
#60094=CARTESIAN_POINT('Ctrl Pts',(355.371290146867,322.156977028214,412.54203615688));
#60095=CARTESIAN_POINT('Ctrl Pts',(355.756401100623,322.072751303211,412.310773721906));
#60096=CARTESIAN_POINT('Ctrl Pts',(356.48597524127,322.072751303211,411.88955389541));
#60097=CARTESIAN_POINT('Ctrl Pts',(356.878809861776,322.156977028214,411.671669243669));
#60098=CARTESIAN_POINT('Ctrl Pts',(357.608103617342,322.499210926969,411.282850372095));
#60099=CARTESIAN_POINT('Ctrl Pts',(357.944380155161,322.757206995828,411.111563108187));
#60100=CARTESIAN_POINT('Ctrl Pts',(358.478369738383,323.352320991875,410.846232204948));
#60101=CARTESIAN_POINT('Ctrl Pts',(358.711716925925,323.729188378078,410.734410205261));
#60102=CARTESIAN_POINT('Ctrl Pts',(359.022098416891,324.555183834244,410.587539642138));
#60103=CARTESIAN_POINT('Ctrl Pts',(359.098918990882,325.004330608665,410.552144880051));
#60104=CARTESIAN_POINT('Ctrl Pts',(359.098918990882,325.846771997758,410.552144880051));
#60105=CARTESIAN_POINT('Ctrl Pts',(359.022098416891,326.295918772179,410.587539642138));
#60106=CARTESIAN_POINT('Ctrl Pts',(358.711716925925,327.121914228345,410.734410205261));
#60107=CARTESIAN_POINT('Ctrl Pts',(358.478369738383,327.498781614548,410.846232204948));
#60108=CARTESIAN_POINT('Ctrl Pts',(357.944380155161,328.093895610594,411.111563108187));
#60109=CARTESIAN_POINT('Ctrl Pts',(357.608103617341,328.351891679454,411.282850372095));
#60110=CARTESIAN_POINT('Ctrl Pts',(356.878809861776,328.694125578209,411.671669243669));
#60111=CARTESIAN_POINT('Ctrl Pts',(356.485975241269,328.778351303211,411.88955389541));
#60112=CARTESIAN_POINT('Ctrl Pts',(355.756401100623,328.778351303211,412.310773721906));
#60113=CARTESIAN_POINT('Ctrl Pts',(355.371290146867,328.694125578208,412.54203615688));
#60114=CARTESIAN_POINT('Ctrl Pts',(354.66991624883,328.351891679453,412.979213640235));
#60115=CARTESIAN_POINT('Ctrl Pts',(354.353438858032,328.093895610594,413.184794032729));
#60116=CARTESIAN_POINT('Ctrl Pts',(353.856660763806,327.498781614547,413.514577125536));
#60117=CARTESIAN_POINT('Ctrl Pts',(353.643146477605,327.121914228344,413.660750718005));
#60118=CARTESIAN_POINT('Ctrl Pts',(353.360762093389,326.295918772179,413.856113692485));
#60119=CARTESIAN_POINT('Ctrl Pts',(353.291699043265,325.846771997757,413.904944880051));
#60120=CARTESIAN_POINT('Ctrl Pts',(353.291699043265,325.425551303211,413.904944880051));
#60121=CARTESIAN_POINT('',(353.197641020201,325.425551303211,413.742031605245));
#60122=CARTESIAN_POINT('Origin',(367.928095722949,325.425551303212,432.550327568991));
#60123=CARTESIAN_POINT('',(365.545644264409,325.425551303212,433.918816276238));
#60124=CARTESIAN_POINT('',(365.988628751342,327.022151685719,433.663059063461));
#60125=CARTESIAN_POINT('Origin',(367.925055850946,325.425551303212,432.545062356238));
#60126=CARTESIAN_POINT('Origin',(367.925055850946,325.425551303212,432.545062356238));
#60127=CARTESIAN_POINT('',(366.061877143581,326.986821771622,433.690971921189));
#60128=CARTESIAN_POINT('',(365.99595359057,327.018618694307,433.665850349235));
#60129=CARTESIAN_POINT('Origin',(367.955454570946,325.425551303212,432.597714483763));
#60130=CARTESIAN_POINT('Origin',(367.955454570946,322.720959303212,432.597714483763));
#60131=CARTESIAN_POINT('Origin',(413.999456970946,322.720959303215,445.00000055189));
#60132=CARTESIAN_POINT('',(413.999456970946,326.986821771626,447.18651542674));
#60133=CARTESIAN_POINT('Origin',(413.999456970946,325.425551303215,445.00000055189));
#60134=CARTESIAN_POINT('Origin',(413.399976330946,325.425551303215,445.00000055189));
#60135=CARTESIAN_POINT('',(413.333367370946,327.373892153977,447.728596485562));
#60136=CARTESIAN_POINT('',(413.333367370946,325.425551303215,441.64720055189));
#60137=CARTESIAN_POINT('Origin',(413.333367370946,325.425551303215,445.00000055189));
#60138=CARTESIAN_POINT('Origin',(413.333367370946,325.425551303215,445.00000055189));
#60139=CARTESIAN_POINT('',(413.399976330946,327.335185115742,447.67438837968));
#60140=CARTESIAN_POINT('Origin',(413.105376970957,167.573893717184,445.000000551892));
#60141=CARTESIAN_POINT('',(413.105376970957,169.914663296231,446.341120551892));
#60142=CARTESIAN_POINT('',(413.105376970957,168.3660713102,446.341120551892));
#60143=CARTESIAN_POINT('',(413.105376970957,169.914663296231,446.341120551892));
#60144=CARTESIAN_POINT('',(413.105376970957,167.591775317184,445.000000551892));
#60145=CARTESIAN_POINT('',(413.105376970957,168.3660713102,446.341120551892));
#60146=CARTESIAN_POINT('',(413.105376970957,168.3660713102,443.658880551892));
#60147=CARTESIAN_POINT('',(413.105376970957,167.591775317184,445.000000551892));
#60148=CARTESIAN_POINT('',(413.105376970957,169.914663296231,443.658880551892));
#60149=CARTESIAN_POINT('',(413.105376970957,168.3660713102,443.658880551892));
#60150=CARTESIAN_POINT('',(413.105376970957,170.688959289246,445.000000551892));
#60151=CARTESIAN_POINT('',(413.105376970957,169.914663296231,443.658880551892));
#60152=CARTESIAN_POINT('',(413.105376970957,170.688959289246,445.000000551892));
#60153=CARTESIAN_POINT('Origin',(414.017338570957,170.301811292738,445.670560551892));
#60154=CARTESIAN_POINT('',(413.999456970957,170.688959289246,445.000000551892));
#60155=CARTESIAN_POINT('',(413.999456970957,169.914663296231,446.341120551892));
#60156=CARTESIAN_POINT('',(413.999456970957,170.688959289246,445.000000551892));
#60157=CARTESIAN_POINT('',(413.105376970957,169.914663296231,446.341120551892));
#60158=CARTESIAN_POINT('',(413.105376970957,170.688959289246,445.000000551892));
#60159=CARTESIAN_POINT('Origin',(414.017338570957,170.301811292738,444.329440551892));
#60160=CARTESIAN_POINT('',(413.999456970957,169.914663296231,443.658880551892));
#60161=CARTESIAN_POINT('',(413.999456970957,169.914663296231,443.658880551892));
#60162=CARTESIAN_POINT('',(413.105376970957,169.914663296231,443.658880551892));
#60163=CARTESIAN_POINT('Origin',(414.017338570957,169.140367303215,443.658880551892));
#60164=CARTESIAN_POINT('',(413.999456970957,168.3660713102,443.658880551892));
#60165=CARTESIAN_POINT('',(413.105376970957,168.3660713102,443.658880551892));
#60166=CARTESIAN_POINT('',(413.999456970957,169.914663296231,443.658880551892));
#60167=CARTESIAN_POINT('Origin',(414.017338570957,167.978923313692,444.329440551892));
#60168=CARTESIAN_POINT('',(413.999456970957,167.591775317184,445.000000551892));
#60169=CARTESIAN_POINT('',(413.999456970957,167.591775317184,445.000000551892));
#60170=CARTESIAN_POINT('',(413.105376970957,167.591775317184,445.000000551892));
#60171=CARTESIAN_POINT('Origin',(414.017338570957,167.978923313692,445.670560551892));
#60172=CARTESIAN_POINT('',(413.999456970957,168.3660713102,446.341120551892));
#60173=CARTESIAN_POINT('',(413.999456970957,168.3660713102,446.341120551892));
#60174=CARTESIAN_POINT('',(413.105376970957,168.3660713102,446.341120551892));
#60175=CARTESIAN_POINT('Origin',(414.017338570957,169.140367303215,446.341120551892));
#60176=CARTESIAN_POINT('',(413.999456970957,169.914663296231,446.341120551892));
#60177=CARTESIAN_POINT('Origin',(356.121188170957,167.57389371718,477.899837295124));
#60178=CARTESIAN_POINT('',(354.959744181434,169.914663296227,477.229277295124));
#60179=CARTESIAN_POINT('',(354.959744181434,168.366071310196,477.229277295124));
#60180=CARTESIAN_POINT('',(354.959744181434,169.914663296227,477.229277295124));
#60181=CARTESIAN_POINT('',(356.121188170957,167.59177531718,477.899837295124));
#60182=CARTESIAN_POINT('',(354.959744181434,168.366071310196,477.229277295124));
#60183=CARTESIAN_POINT('',(357.28263216048,168.366071310196,478.570397295124));
#60184=CARTESIAN_POINT('',(356.121188170957,167.59177531718,477.899837295124));
#60185=CARTESIAN_POINT('',(357.28263216048,169.914663296227,478.570397295124));
#60186=CARTESIAN_POINT('',(357.28263216048,168.366071310196,478.570397295124));
#60187=CARTESIAN_POINT('',(356.121188170957,170.688959289243,477.899837295124));
#60188=CARTESIAN_POINT('',(357.28263216048,169.914663296227,478.570397295124));
#60189=CARTESIAN_POINT('',(356.121188170957,170.688959289243,477.899837295124));
#60190=CARTESIAN_POINT('Origin',(355.402364199503,170.130975246119,477.211963510373));
#60191=CARTESIAN_POINT('',(355.674148170957,170.688959289243,478.67413328814));
#60192=CARTESIAN_POINT('',(354.512704181433,169.914663296227,478.00357328814));
#60193=CARTESIAN_POINT('',(355.674148170957,170.688959289243,478.67413328814));
#60194=CARTESIAN_POINT('',(354.959744181434,169.914663296227,477.229277295124));
#60195=CARTESIAN_POINT('',(356.121188170957,170.688959289243,477.899837295124));
#60196=CARTESIAN_POINT('Origin',(356.563808189027,170.472647339351,477.882523510373));
#60197=CARTESIAN_POINT('',(356.83559216048,169.914663296227,479.34469328814));
#60198=CARTESIAN_POINT('',(356.83559216048,169.914663296227,479.34469328814));
#60199=CARTESIAN_POINT('',(357.28263216048,169.914663296227,478.570397295124));
#60200=CARTESIAN_POINT('Origin',(357.05911216048,168.348189710196,478.957545291632));
#60201=CARTESIAN_POINT('',(356.83559216048,168.366071310196,479.34469328814));
#60202=CARTESIAN_POINT('',(357.28263216048,168.366071310196,478.570397295124));
#60203=CARTESIAN_POINT('',(356.83559216048,169.914663296227,479.34469328814));
#60204=CARTESIAN_POINT('Origin',(356.563808189027,167.808087267072,477.882523510373));
#60205=CARTESIAN_POINT('',(355.674148170957,167.59177531718,478.67413328814));
#60206=CARTESIAN_POINT('',(355.674148170957,167.59177531718,478.67413328814));
#60207=CARTESIAN_POINT('',(356.121188170957,167.59177531718,477.899837295124));
#60208=CARTESIAN_POINT('Origin',(355.402364199503,168.149759360304,477.211963510373));
#60209=CARTESIAN_POINT('',(354.512704181434,168.366071310196,478.00357328814));
#60210=CARTESIAN_POINT('',(354.512704181434,168.366071310196,478.00357328814));
#60211=CARTESIAN_POINT('',(354.959744181434,168.366071310196,477.229277295124));
#60212=CARTESIAN_POINT('Origin',(354.736224181434,168.348189710196,477.616425291632));
#60213=CARTESIAN_POINT('',(354.512704181433,169.914663296227,478.00357328814));
#60214=CARTESIAN_POINT('Origin',(355.674148170957,166.435775303211,478.67413328814));
#60215=CARTESIAN_POINT('',(353.780570743585,170.701637771622,477.580875850715));
#60216=CARTESIAN_POINT('Origin',(355.674148170957,169.140367303211,478.67413328814));
#60217=CARTESIAN_POINT('Origin',(355.973888490957,169.140367303211,478.154967824823));
#60218=CARTESIAN_POINT('',(353.644159575734,171.088708153973,476.732984806507));
#60219=CARTESIAN_POINT('',(358.910802944765,169.140367303212,479.773682773344));
#60220=CARTESIAN_POINT('Origin',(356.007192970957,169.140367303212,478.097282773343));
#60221=CARTESIAN_POINT('Origin',(356.007192970957,169.140367303212,478.097282773343));
#60222=CARTESIAN_POINT('',(353.657800692519,171.050001115738,476.817773910928));
#60223=CARTESIAN_POINT('Origin',(356.10125099402,169.140367303212,477.934369498538));
#60224=CARTESIAN_POINT('',(359.098918990893,169.140367303212,479.447856223731));
#60225=CARTESIAN_POINT('Ctrl Pts',(359.098918990893,169.140367303212,479.447856223731));
#60226=CARTESIAN_POINT('Ctrl Pts',(359.098918990893,168.719146608665,479.447856223731));
#60227=CARTESIAN_POINT('Ctrl Pts',(359.022098416902,168.269999834244,479.412461461645));
#60228=CARTESIAN_POINT('Ctrl Pts',(358.711716925936,167.444004378079,479.265590898522));
#60229=CARTESIAN_POINT('Ctrl Pts',(358.478369738394,167.067136991875,479.153768898834));
#60230=CARTESIAN_POINT('Ctrl Pts',(357.944380155172,166.472022995829,478.888437995595));
#60231=CARTESIAN_POINT('Ctrl Pts',(357.608103617353,166.214026926969,478.717150731687));
#60232=CARTESIAN_POINT('Ctrl Pts',(356.878809861787,165.871793028214,478.328331860114));
#60233=CARTESIAN_POINT('Ctrl Pts',(356.48597524128,165.787567303211,478.110447208372));
#60234=CARTESIAN_POINT('Ctrl Pts',(355.756401100634,165.787567303211,477.689227381876));
#60235=CARTESIAN_POINT('Ctrl Pts',(355.371290146878,165.871793028214,477.457964946902));
#60236=CARTESIAN_POINT('Ctrl Pts',(354.669916248842,166.214026926969,477.020787463548));
#60237=CARTESIAN_POINT('Ctrl Pts',(354.353438858043,166.472022995828,476.815207071053));
#60238=CARTESIAN_POINT('Ctrl Pts',(353.856660763817,167.067136991875,476.485423978246));
#60239=CARTESIAN_POINT('Ctrl Pts',(353.643146477615,167.444004378078,476.339250385777));
#60240=CARTESIAN_POINT('Ctrl Pts',(353.3607620934,168.269999834243,476.143887411298));
#60241=CARTESIAN_POINT('Ctrl Pts',(353.291699043276,168.719146608665,476.095056223732));
#60242=CARTESIAN_POINT('Ctrl Pts',(353.291699043276,169.561587997758,476.095056223732));
#60243=CARTESIAN_POINT('Ctrl Pts',(353.3607620934,170.010734772179,476.143887411298));
#60244=CARTESIAN_POINT('Ctrl Pts',(353.643146477615,170.836730228344,476.339250385777));
#60245=CARTESIAN_POINT('Ctrl Pts',(353.856660763817,171.213597614548,476.485423978246));
#60246=CARTESIAN_POINT('Ctrl Pts',(354.353438858043,171.808711610594,476.815207071053));
#60247=CARTESIAN_POINT('Ctrl Pts',(354.669916248841,172.066707679454,477.020787463548));
#60248=CARTESIAN_POINT('Ctrl Pts',(355.371290146877,172.408941578209,477.457964946902));
#60249=CARTESIAN_POINT('Ctrl Pts',(355.756401100633,172.493167303211,477.689227381876));
#60250=CARTESIAN_POINT('Ctrl Pts',(356.48597524128,172.493167303212,478.110447208372));
#60251=CARTESIAN_POINT('Ctrl Pts',(356.878809861787,172.408941578209,478.328331860114));
#60252=CARTESIAN_POINT('Ctrl Pts',(357.608103617352,172.066707679454,478.717150731687));
#60253=CARTESIAN_POINT('Ctrl Pts',(357.944380155172,171.808711610595,478.888437995595));
#60254=CARTESIAN_POINT('Ctrl Pts',(358.478369738394,171.213597614548,479.153768898834));
#60255=CARTESIAN_POINT('Ctrl Pts',(358.711716925935,170.836730228345,479.265590898522));
#60256=CARTESIAN_POINT('Ctrl Pts',(359.022098416902,170.010734772179,479.412461461645));
#60257=CARTESIAN_POINT('Ctrl Pts',(359.098918990893,169.561587997758,479.447856223732));
#60258=CARTESIAN_POINT('Ctrl Pts',(359.098918990893,169.140367303212,479.447856223732));
#60259=CARTESIAN_POINT('',(359.004860967829,169.140367303212,479.610769498538));
#60260=CARTESIAN_POINT('Origin',(367.928095722957,169.140367303212,457.449673534792));
#60261=CARTESIAN_POINT('',(370.304467437494,169.140367303212,458.828692667544));
#60262=CARTESIAN_POINT('',(369.861482950562,170.736967685717,458.572935454769));
#60263=CARTESIAN_POINT('Origin',(367.925055850957,169.140367303212,457.454938747544));
#60264=CARTESIAN_POINT('Origin',(367.925055850957,169.140367303212,457.454938747544));
#60265=CARTESIAN_POINT('',(369.849031998329,170.701637771622,458.495544057444));
#60266=CARTESIAN_POINT('',(369.860237855339,170.733434694307,458.565196315036));
#60267=CARTESIAN_POINT('Origin',(367.955454570957,169.140367303212,457.402286620019));
#60268=CARTESIAN_POINT('Origin',(367.955454570957,166.435775303212,457.402286620019));
#60269=CARTESIAN_POINT('Origin',(413.999456970957,166.435775303215,445.000000551892));
#60270=CARTESIAN_POINT('',(413.999456970957,170.701637771626,447.186515426741));
#60271=CARTESIAN_POINT('Origin',(413.999456970957,169.140367303215,445.000000551892));
#60272=CARTESIAN_POINT('Origin',(413.399976330957,169.140367303215,445.000000551892));
#60273=CARTESIAN_POINT('',(413.333367370957,171.088708153977,447.728596485564));
#60274=CARTESIAN_POINT('',(413.333367370957,169.140367303215,441.647200551892));
#60275=CARTESIAN_POINT('Origin',(413.333367370957,169.140367303215,445.000000551892));
#60276=CARTESIAN_POINT('Origin',(413.333367370957,169.140367303215,445.000000551892));
#60277=CARTESIAN_POINT('',(413.399976330957,171.050001115742,447.674388379681));
#60278=CARTESIAN_POINT('Origin',(413.145251324829,169.140367303215,445.000000551892));
#60279=CARTESIAN_POINT('',(412.957135278702,169.140367303215,441.647200551892));
#60280=CARTESIAN_POINT('Ctrl Pts',(412.957135278702,169.140367303215,441.647200551892));
#60281=CARTESIAN_POINT('Ctrl Pts',(412.957135278702,168.719146608669,441.647200551892));
#60282=CARTESIAN_POINT('Ctrl Pts',(412.964892802569,168.269999834247,441.731426501545));
#60283=CARTESIAN_POINT('Ctrl Pts',(412.99288990932,167.444004378082,442.073660039147));
#60284=CARTESIAN_POINT('Ctrl Pts',(413.012722810659,167.067136991879,442.331655631304));
#60285=CARTESIAN_POINT('Ctrl Pts',(413.049934299656,166.472022995832,442.92676962735));
#60286=CARTESIAN_POINT('Ctrl Pts',(413.069733446677,166.214026926973,443.303637283752));
#60287=CARTESIAN_POINT('Ctrl Pts',(413.097653304206,165.871793028218,444.12963363868));
#60288=CARTESIAN_POINT('Ctrl Pts',(413.105376970957,165.787567303215,444.578780725396));
#60289=CARTESIAN_POINT('Ctrl Pts',(413.105376970957,165.787567303215,445.421220378388));
#60290=CARTESIAN_POINT('Ctrl Pts',(413.097653304206,165.871793028218,445.870367465103));
#60291=CARTESIAN_POINT('Ctrl Pts',(413.069733446677,166.214026926973,446.696363820031));
#60292=CARTESIAN_POINT('Ctrl Pts',(413.049934299656,166.472022995832,447.073231476433));
#60293=CARTESIAN_POINT('Ctrl Pts',(413.012722810659,167.067136991879,447.66834547248));
#60294=CARTESIAN_POINT('Ctrl Pts',(412.99288990932,167.444004378082,447.926341064636));
#60295=CARTESIAN_POINT('Ctrl Pts',(412.964892802569,168.269999834247,448.268574602239));
#60296=CARTESIAN_POINT('Ctrl Pts',(412.957135278702,168.719146608669,448.352800551892));
#60297=CARTESIAN_POINT('Ctrl Pts',(412.957135278702,169.561587997761,448.352800551892));
#60298=CARTESIAN_POINT('Ctrl Pts',(412.964892802569,170.010734772183,448.268574602239));
#60299=CARTESIAN_POINT('Ctrl Pts',(412.992889909319,170.836730228348,447.926341064636));
#60300=CARTESIAN_POINT('Ctrl Pts',(413.012722810659,171.213597614551,447.66834547248));
#60301=CARTESIAN_POINT('Ctrl Pts',(413.049934299656,171.808711610598,447.073231476433));
#60302=CARTESIAN_POINT('Ctrl Pts',(413.069733446677,172.066707679457,446.696363820031));
#60303=CARTESIAN_POINT('Ctrl Pts',(413.097653304206,172.408941578212,445.870367465103));
#60304=CARTESIAN_POINT('Ctrl Pts',(413.105376970957,172.493167303215,445.421220378388));
#60305=CARTESIAN_POINT('Ctrl Pts',(413.105376970957,172.493167303215,444.578780725396));
#60306=CARTESIAN_POINT('Ctrl Pts',(413.097653304206,172.408941578212,444.12963363868));
#60307=CARTESIAN_POINT('Ctrl Pts',(413.069733446677,172.066707679457,443.303637283752));
#60308=CARTESIAN_POINT('Ctrl Pts',(413.049934299656,171.808711610598,442.92676962735));
#60309=CARTESIAN_POINT('Ctrl Pts',(413.012722810659,171.213597614551,442.331655631304));
#60310=CARTESIAN_POINT('Ctrl Pts',(412.992889909319,170.836730228348,442.073660039147));
#60311=CARTESIAN_POINT('Ctrl Pts',(412.964892802569,170.010734772183,441.731426501545));
#60312=CARTESIAN_POINT('Ctrl Pts',(412.957135278702,169.561587997761,441.647200551892));
#60313=CARTESIAN_POINT('Ctrl Pts',(412.957135278702,169.140367303215,441.647200551892));
#60314=CARTESIAN_POINT('',(413.145251324829,169.140367303215,441.647200551892));
#60315=CARTESIAN_POINT('Origin',(392.589549066957,169.140367303214,445.000000551892));
#60316=CARTESIAN_POINT('',(392.534831370957,170.701637771624,442.813485677043));
#60317=CARTESIAN_POINT('',(392.589549066957,170.733434694309,442.768954991405));
#60318=CARTESIAN_POINT('Origin',(392.534831370957,169.140367303214,445.000000551892));
#60319=CARTESIAN_POINT('Origin',(392.534831370957,166.435775303214,445.000000551892));
#60320=CARTESIAN_POINT('Origin',(368.234803806253,169.140367303212,456.91843955143));
#60321=CARTESIAN_POINT('',(370.61421539279,169.140367303212,458.29219347143));
#60322=CARTESIAN_POINT('Origin',(368.234803806243,325.425551303212,433.081561552353));
#60323=CARTESIAN_POINT('',(365.855392219706,325.425551303212,434.455315472353));
#60324=CARTESIAN_POINT('Origin',(392.534831370946,322.720959303214,445.00000055189));
#60325=CARTESIAN_POINT('',(392.534831370946,326.986821771625,442.813485677041));
#60326=CARTESIAN_POINT('Origin',(392.534831370946,325.425551303214,445.00000055189));
#60327=CARTESIAN_POINT('Origin',(392.589549066946,325.425551303214,445.00000055189));
#60328=CARTESIAN_POINT('',(392.589549066946,327.018618694309,442.768954991404));
#60329=CARTESIAN_POINT('Origin',(413.145251324819,325.425551303215,445.00000055189));
#60330=CARTESIAN_POINT('',(412.957135278691,325.425551303215,441.64720055189));
#60331=CARTESIAN_POINT('Ctrl Pts',(412.957135278691,325.425551303215,441.64720055189));
#60332=CARTESIAN_POINT('Ctrl Pts',(412.957135278691,325.004330608669,441.64720055189));
#60333=CARTESIAN_POINT('Ctrl Pts',(412.964892802559,324.555183834248,441.731426501543));
#60334=CARTESIAN_POINT('Ctrl Pts',(412.992889909309,323.729188378082,442.073660039146));
#60335=CARTESIAN_POINT('Ctrl Pts',(413.012722810649,323.352320991879,442.331655631302));
#60336=CARTESIAN_POINT('Ctrl Pts',(413.049934299646,322.757206995832,442.926769627349));
#60337=CARTESIAN_POINT('Ctrl Pts',(413.069733446666,322.499210926973,443.303637283751));
#60338=CARTESIAN_POINT('Ctrl Pts',(413.097653304196,322.156977028218,444.129633638679));
#60339=CARTESIAN_POINT('Ctrl Pts',(413.105376970947,322.072751303215,444.578780725394));
#60340=CARTESIAN_POINT('Ctrl Pts',(413.105376970947,322.072751303215,445.421220378386));
#60341=CARTESIAN_POINT('Ctrl Pts',(413.097653304196,322.156977028218,445.870367465102));
#60342=CARTESIAN_POINT('Ctrl Pts',(413.069733446666,322.499210926973,446.69636382003));
#60343=CARTESIAN_POINT('Ctrl Pts',(413.049934299646,322.757206995832,447.073231476432));
#60344=CARTESIAN_POINT('Ctrl Pts',(413.012722810649,323.352320991879,447.668345472478));
#60345=CARTESIAN_POINT('Ctrl Pts',(412.992889909309,323.729188378082,447.926341064635));
#60346=CARTESIAN_POINT('Ctrl Pts',(412.964892802559,324.555183834248,448.268574602237));
#60347=CARTESIAN_POINT('Ctrl Pts',(412.957135278691,325.004330608669,448.35280055189));
#60348=CARTESIAN_POINT('Ctrl Pts',(412.957135278691,325.846771997762,448.35280055189));
#60349=CARTESIAN_POINT('Ctrl Pts',(412.964892802559,326.295918772183,448.268574602237));
#60350=CARTESIAN_POINT('Ctrl Pts',(412.992889909309,327.121914228348,447.926341064635));
#60351=CARTESIAN_POINT('Ctrl Pts',(413.012722810649,327.498781614552,447.668345472478));
#60352=CARTESIAN_POINT('Ctrl Pts',(413.049934299645,328.093895610598,447.073231476432));
#60353=CARTESIAN_POINT('Ctrl Pts',(413.069733446666,328.351891679458,446.69636382003));
#60354=CARTESIAN_POINT('Ctrl Pts',(413.097653304195,328.694125578213,445.870367465102));
#60355=CARTESIAN_POINT('Ctrl Pts',(413.105376970946,328.778351303215,445.421220378386));
#60356=CARTESIAN_POINT('Ctrl Pts',(413.105376970946,328.778351303215,444.578780725394));
#60357=CARTESIAN_POINT('Ctrl Pts',(413.097653304195,328.694125578213,444.129633638679));
#60358=CARTESIAN_POINT('Ctrl Pts',(413.069733446666,328.351891679458,443.303637283751));
#60359=CARTESIAN_POINT('Ctrl Pts',(413.049934299645,328.093895610598,442.926769627349));
#60360=CARTESIAN_POINT('Ctrl Pts',(413.012722810649,327.498781614552,442.331655631302));
#60361=CARTESIAN_POINT('Ctrl Pts',(412.992889909309,327.121914228348,442.073660039146));
#60362=CARTESIAN_POINT('Ctrl Pts',(412.964892802559,326.295918772183,441.731426501543));
#60363=CARTESIAN_POINT('Ctrl Pts',(412.957135278691,325.846771997762,441.64720055189));
#60364=CARTESIAN_POINT('Ctrl Pts',(412.957135278691,325.425551303215,441.64720055189));
#60365=CARTESIAN_POINT('',(413.145251324819,325.425551303215,441.64720055189));
#60366=CARTESIAN_POINT('Origin',(375.115917770957,168.514511303212,445.000000551892));
#60367=CARTESIAN_POINT('',(375.115917770957,163.418255303212,407.010541351892));
#60368=CARTESIAN_POINT('',(353.039917037922,163.418255303211,414.083189559432));
#60369=CARTESIAN_POINT('Origin',(375.115917770957,163.418255303212,445.000000551892));
#60370=CARTESIAN_POINT('Origin',(375.115917770957,163.418255303212,445.000000551892));
#60371=CARTESIAN_POINT('',(375.115917770956,173.610767303212,407.010541351892));
#60372=CARTESIAN_POINT('',(375.115917770957,168.514511303212,407.010541351892));
#60373=CARTESIAN_POINT('Origin',(375.115917770956,173.610767303212,445.000000551892));
#60374=CARTESIAN_POINT('Origin',(375.115917770957,161.810965703212,445.000000551892));
#60375=CARTESIAN_POINT('',(353.579167835194,161.810965703211,414.838394960011));
#60376=CARTESIAN_POINT('Origin',(391.658632970951,247.282959303214,448.361741351891));
#60377=CARTESIAN_POINT('Ctrl Pts',(388.115106324202,164.491151303213,448.361741351892));
#60378=CARTESIAN_POINT('Ctrl Pts',(388.541335653383,163.776414442266,448.361741351892));
#60379=CARTESIAN_POINT('Ctrl Pts',(388.966604868594,163.061101141136,448.361741351892));
#60380=CARTESIAN_POINT('Ctrl Pts',(389.391142518198,162.345359303214,448.361741351892));
#60381=CARTESIAN_POINT('Origin',(375.115917770957,164.276572103213,445.000000551892));
#60382=CARTESIAN_POINT('Ctrl Pts',(389.391142518198,162.345359303214,441.638259751892));
#60383=CARTESIAN_POINT('Ctrl Pts',(388.966603199882,163.061103954472,441.638259751892));
#60384=CARTESIAN_POINT('Ctrl Pts',(388.541330836671,163.776422519329,441.638259751892));
#60385=CARTESIAN_POINT('Ctrl Pts',(388.115106324202,164.491151303213,441.638259751892));
#60386=CARTESIAN_POINT('Origin',(391.658632970951,247.282959303214,441.638259751891));
#60387=CARTESIAN_POINT('Origin',(375.115917770946,325.988821703213,445.00000055189));
#60388=CARTESIAN_POINT('',(375.115917770946,320.829980103212,407.01054135189));
#60389=CARTESIAN_POINT('Origin',(375.115917770947,320.829980103212,445.000000551891));
#60390=CARTESIAN_POINT('',(375.115917770946,325.988821703212,407.01054135189));
#60391=CARTESIAN_POINT('Origin',(422.081940170956,183.445647303215,445.000000551892));
#60392=CARTESIAN_POINT('',(375.115917770956,183.445647303212,407.010541351892));
#60393=CARTESIAN_POINT('Origin',(375.115917770956,183.445647303212,445.000000551892));
#60394=CARTESIAN_POINT('Origin',(422.081940170956,173.610767303215,445.000000551892));
#60395=CARTESIAN_POINT('',(375.115917770957,173.610767303213,491.948141351892));
#60396=CARTESIAN_POINT('Origin',(375.115917770956,173.610767303212,445.000000551892));
#60397=CARTESIAN_POINT('Origin',(375.115917770956,174.057807303212,445.000000551892));
#60398=CARTESIAN_POINT('',(375.115917770957,174.057807303213,491.948141351892));
#60399=CARTESIAN_POINT('Origin',(375.115917770951,247.220373703212,445.000000551891));
#60400=CARTESIAN_POINT('',(375.115917770947,310.995100103212,407.01054135189));
#60401=CARTESIAN_POINT('',(375.115917770951,247.220373703212,407.010541351891));
#60402=CARTESIAN_POINT('Origin',(375.115917770947,310.995100103212,445.000000551891));
#60403=CARTESIAN_POINT('Origin',(328.149895370947,310.995100103209,445.000000551891));
#60404=CARTESIAN_POINT('Origin',(328.149895370946,320.829980103209,445.000000551891));
#60405=CARTESIAN_POINT('',(375.115917770947,320.829980103213,491.94814135189));
#60406=CARTESIAN_POINT('Origin',(375.115917770947,320.829980103212,445.00000055189));
#60407=CARTESIAN_POINT('Origin',(375.115917770947,320.382940103212,445.00000055189));
#60408=CARTESIAN_POINT('',(375.115917770947,320.382940103213,491.94814135189));
#60409=CARTESIAN_POINT('Origin',(328.660166744143,326.48056570321,497.549298322233));
#60410=CARTESIAN_POINT('',(317.315530368861,326.480565703209,499.630144284955));
#60411=CARTESIAN_POINT('',(317.315530368861,326.480565703209,495.46845235951));
#60412=CARTESIAN_POINT('Origin',(322.566620000601,326.48056570321,497.549298322233));
#60413=CARTESIAN_POINT('',(318.139009719652,326.480565703209,501.05645235951));
#60414=CARTESIAN_POINT('',(318.139009719652,326.480565703209,501.05645235951));
#60415=CARTESIAN_POINT('',(321.743140649812,326.48056570321,503.137298322233));
#60416=CARTESIAN_POINT('Origin',(322.566620000605,326.48056570321,497.549298322231));
#60417=CARTESIAN_POINT('',(323.390099351396,326.48056570321,503.137298322233));
#60418=CARTESIAN_POINT('',(323.390099351396,326.48056570321,503.137298322233));
#60419=CARTESIAN_POINT('',(326.994230281556,326.48056570321,501.05645235951));
#60420=CARTESIAN_POINT('Origin',(322.566620000604,326.48056570321,497.549298322233));
#60421=CARTESIAN_POINT('',(327.817709632347,326.48056570321,499.630144284955));
#60422=CARTESIAN_POINT('',(327.817709632347,326.48056570321,499.630144284955));
#60423=CARTESIAN_POINT('',(327.817709632347,326.48056570321,495.46845235951));
#60424=CARTESIAN_POINT('Origin',(322.566620000604,326.48056570321,497.549298322233));
#60425=CARTESIAN_POINT('',(326.994230281556,326.48056570321,494.042144284955));
#60426=CARTESIAN_POINT('',(326.994230281556,326.48056570321,494.042144284955));
#60427=CARTESIAN_POINT('',(323.390099351396,326.48056570321,491.961298322233));
#60428=CARTESIAN_POINT('Origin',(322.566620000604,326.48056570321,497.549298322233));
#60429=CARTESIAN_POINT('',(321.743140649812,326.48056570321,491.961298322233));
#60430=CARTESIAN_POINT('',(321.743140649812,326.48056570321,491.961298322233));
#60431=CARTESIAN_POINT('',(318.139009719652,326.480565703209,494.042144284955));
#60432=CARTESIAN_POINT('Origin',(322.566620000605,326.48056570321,497.549298322235));
#60433=CARTESIAN_POINT('',(317.315530368861,326.480565703209,495.46845235951));
#60434=CARTESIAN_POINT('Origin',(322.566620000609,326.062734664725,497.549298322235));
#60435=CARTESIAN_POINT('',(319.340386696372,326.016308993793,491.961298322233));
#60436=CARTESIAN_POINT('Ctrl Pts',(319.340386696347,326.016308993785,491.961298322233));
#60437=CARTESIAN_POINT('Ctrl Pts',(320.621596852842,326.386162508159,491.961298322233));
#60438=CARTESIAN_POINT('Ctrl Pts',(321.743140649817,326.48056570321,491.961298322233));
#60439=CARTESIAN_POINT('Ctrl Pts',(318.13900971965,326.480565703209,494.042144284959));
#60440=CARTESIAN_POINT('Ctrl Pts',(318.699781618137,326.386162508158,493.070858865322));
#60441=CARTESIAN_POINT('Ctrl Pts',(319.340386696385,326.016308993785,491.961298322211));
#60442=CARTESIAN_POINT('Origin',(325.810734904862,323.65527290321,503.137298322233));
#60443=CARTESIAN_POINT('',(325.792853304836,326.016308993794,503.137298322233));
#60444=CARTESIAN_POINT('Ctrl Pts',(325.792853304861,326.016308993786,503.137298322233));
#60445=CARTESIAN_POINT('Ctrl Pts',(324.511643148366,326.386162508159,503.137298322233));
#60446=CARTESIAN_POINT('Ctrl Pts',(323.390099351391,326.48056570321,503.137298322233));
#60447=CARTESIAN_POINT('',(319.340386696372,326.016308993794,503.137298322233));
#60448=CARTESIAN_POINT('Ctrl Pts',(321.743140649817,326.48056570321,503.137298322233));
#60449=CARTESIAN_POINT('Ctrl Pts',(320.621596852842,326.386162508159,503.137298322233));
#60450=CARTESIAN_POINT('Ctrl Pts',(319.340386696347,326.016308993786,503.137298322233));
#60451=CARTESIAN_POINT('',(319.340386696372,326.016308993794,503.137298322233));
#60452=CARTESIAN_POINT('',(325.792853304836,326.016308993794,503.137298322233));
#60453=CARTESIAN_POINT('Origin',(327.405969956952,326.49844730321,500.343298322233));
#60454=CARTESIAN_POINT('',(329.019086609067,326.016308993794,497.549298322233));
#60455=CARTESIAN_POINT('Ctrl Pts',(329.01908660908,326.016308993786,497.549298322211));
#60456=CARTESIAN_POINT('Ctrl Pts',(328.378481530832,326.386162508159,498.658858865322));
#60457=CARTESIAN_POINT('Ctrl Pts',(327.817709632345,326.48056570321,499.630144284959));
#60458=CARTESIAN_POINT('Ctrl Pts',(326.994230281558,326.48056570321,501.056452359506));
#60459=CARTESIAN_POINT('Ctrl Pts',(326.433458383071,326.386162508159,502.027737779143));
#60460=CARTESIAN_POINT('Ctrl Pts',(325.792853304823,326.016308993786,503.137298322255));
#60461=CARTESIAN_POINT('',(329.019086609067,326.016308993794,497.549298322233));
#60462=CARTESIAN_POINT('Origin',(322.566620000604,326.062734664728,497.549298322233));
#60463=CARTESIAN_POINT('',(325.792853304836,326.016308993794,491.961298322233));
#60464=CARTESIAN_POINT('Ctrl Pts',(323.390099351391,326.48056570321,491.961298322233));
#60465=CARTESIAN_POINT('Ctrl Pts',(324.511643148366,326.386162508159,491.961298322233));
#60466=CARTESIAN_POINT('Ctrl Pts',(325.792853304861,326.016308993786,491.961298322233));
#60467=CARTESIAN_POINT('Ctrl Pts',(325.792853304823,326.016308993786,491.961298322211));
#60468=CARTESIAN_POINT('Ctrl Pts',(326.433458383071,326.386162508159,493.070858865322));
#60469=CARTESIAN_POINT('Ctrl Pts',(326.994230281558,326.48056570321,494.042144284959));
#60470=CARTESIAN_POINT('Origin',(322.566620000608,326.062734664731,497.549298322233));
#60471=CARTESIAN_POINT('Ctrl Pts',(327.817709632345,326.48056570321,495.468452359506));
#60472=CARTESIAN_POINT('Ctrl Pts',(328.378481530832,326.386162508159,496.439737779143));
#60473=CARTESIAN_POINT('Ctrl Pts',(329.01908660908,326.016308993786,497.549298322255));
#60474=CARTESIAN_POINT('Origin',(322.566620000601,326.062734664725,497.549298322228));
#60475=CARTESIAN_POINT('Origin',(322.5666200006,326.062734664732,497.549298322233));
#60476=CARTESIAN_POINT('',(316.114153392141,326.016308993793,497.549298322233));
#60477=CARTESIAN_POINT('Ctrl Pts',(317.315530368863,326.480565703209,499.630144284959));
#60478=CARTESIAN_POINT('Ctrl Pts',(316.754758470376,326.386162508158,498.658858865322));
#60479=CARTESIAN_POINT('Ctrl Pts',(316.114153392128,326.016308993785,497.549298322211));
#60480=CARTESIAN_POINT('Ctrl Pts',(316.114153392128,326.016308993785,497.549298322255));
#60481=CARTESIAN_POINT('Ctrl Pts',(316.754758470376,326.386162508158,496.439737779143));
#60482=CARTESIAN_POINT('Ctrl Pts',(317.315530368863,326.480565703209,495.468452359506));
#60483=CARTESIAN_POINT('Origin',(322.566620000606,326.06273466473,497.549298322236));
#60484=CARTESIAN_POINT('Ctrl Pts',(319.340386696385,326.016308993786,503.137298322255));
#60485=CARTESIAN_POINT('Ctrl Pts',(318.699781618137,326.386162508159,502.027737779143));
#60486=CARTESIAN_POINT('Ctrl Pts',(318.13900971965,326.480565703209,501.056452359506));
#60487=CARTESIAN_POINT('Origin',(317.727270044256,326.498447303209,500.343298322233));
#60488=CARTESIAN_POINT('',(316.114153392141,326.016308993793,497.549298322233));
#60489=CARTESIAN_POINT('Origin',(317.727270044256,326.498447303209,494.755298322233));
#60490=CARTESIAN_POINT('',(319.340386696372,326.016308993793,491.961298322233));
#60491=CARTESIAN_POINT('Origin',(325.810734904862,323.65527290321,491.961298322233));
#60492=CARTESIAN_POINT('',(325.792853304836,326.016308993794,491.961298322233));
#60493=CARTESIAN_POINT('Origin',(327.405969956952,326.49844730321,494.755298322233));
#60494=CARTESIAN_POINT('Origin',(433.758762284827,326.480565703216,392.450702781548));
#60495=CARTESIAN_POINT('',(422.414125909545,326.480565703216,394.531548744271));
#60496=CARTESIAN_POINT('',(422.414125909545,326.480565703216,390.369856818826));
#60497=CARTESIAN_POINT('Origin',(427.665215541288,326.480565703216,392.450702781548));
#60498=CARTESIAN_POINT('',(423.237605260337,326.480565703216,395.957856818826));
#60499=CARTESIAN_POINT('',(423.237605260337,326.480565703216,395.957856818826));
#60500=CARTESIAN_POINT('',(426.841736190497,326.480565703216,398.038702781548));
#60501=CARTESIAN_POINT('Origin',(427.665215541288,326.480565703216,392.450702781548));
#60502=CARTESIAN_POINT('',(428.48869489208,326.480565703216,398.038702781548));
#60503=CARTESIAN_POINT('',(428.48869489208,326.480565703216,398.038702781548));
#60504=CARTESIAN_POINT('',(432.09282582224,326.480565703216,395.957856818826));
#60505=CARTESIAN_POINT('Origin',(427.665215541288,326.480565703216,392.450702781548));
#60506=CARTESIAN_POINT('',(432.916305173032,326.480565703216,394.531548744271));
#60507=CARTESIAN_POINT('',(432.916305173032,326.480565703216,394.531548744271));
#60508=CARTESIAN_POINT('',(432.916305173032,326.480565703216,390.369856818826));
#60509=CARTESIAN_POINT('Origin',(427.665215541289,326.480565703216,392.450702781548));
#60510=CARTESIAN_POINT('',(432.09282582224,326.480565703216,388.943548744271));
#60511=CARTESIAN_POINT('',(432.09282582224,326.480565703216,388.943548744271));
#60512=CARTESIAN_POINT('',(428.48869489208,326.480565703216,386.862702781548));
#60513=CARTESIAN_POINT('Origin',(427.665215541288,326.480565703216,392.450702781548));
#60514=CARTESIAN_POINT('',(426.841736190497,326.480565703216,386.862702781548));
#60515=CARTESIAN_POINT('',(426.841736190497,326.480565703216,386.862702781548));
#60516=CARTESIAN_POINT('',(423.237605260337,326.480565703216,388.943548744271));
#60517=CARTESIAN_POINT('Origin',(427.665215541288,326.480565703216,392.450702781548));
#60518=CARTESIAN_POINT('',(422.414125909545,326.480565703216,390.369856818826));
#60519=CARTESIAN_POINT('Origin',(427.665215541288,326.062734664734,392.450702781548));
#60520=CARTESIAN_POINT('',(424.438982237057,326.016308993799,386.862702781548));
#60521=CARTESIAN_POINT('Ctrl Pts',(424.438982237031,326.016308993792,386.862702781548));
#60522=CARTESIAN_POINT('Ctrl Pts',(425.720192393527,326.386162508165,386.862702781548));
#60523=CARTESIAN_POINT('Ctrl Pts',(426.841736190502,326.480565703216,386.862702781548));
#60524=CARTESIAN_POINT('Ctrl Pts',(423.237605260334,326.480565703216,388.943548744275));
#60525=CARTESIAN_POINT('Ctrl Pts',(423.798377158822,326.386162508165,387.972263324638));
#60526=CARTESIAN_POINT('Ctrl Pts',(424.438982237069,326.016308993792,386.862702781526));
#60527=CARTESIAN_POINT('Origin',(430.909330445546,323.655272903216,398.038702781548));
#60528=CARTESIAN_POINT('',(430.89144884552,326.0163089938,398.038702781548));
#60529=CARTESIAN_POINT('Ctrl Pts',(430.891448845546,326.016308993792,398.038702781548));
#60530=CARTESIAN_POINT('Ctrl Pts',(429.61023868905,326.386162508165,398.038702781548));
#60531=CARTESIAN_POINT('Ctrl Pts',(428.488694892075,326.480565703216,398.038702781548));
#60532=CARTESIAN_POINT('',(424.438982237057,326.016308993799,398.038702781548));
#60533=CARTESIAN_POINT('Ctrl Pts',(426.841736190502,326.480565703216,398.038702781548));
#60534=CARTESIAN_POINT('Ctrl Pts',(425.720192393527,326.386162508165,398.038702781548));
#60535=CARTESIAN_POINT('Ctrl Pts',(424.438982237031,326.016308993792,398.038702781548));
#60536=CARTESIAN_POINT('',(424.438982237057,326.016308993799,398.038702781548));
#60537=CARTESIAN_POINT('',(430.89144884552,326.016308993799,398.038702781548));
#60538=CARTESIAN_POINT('Origin',(432.504565497636,326.498447303216,395.244702781548));
#60539=CARTESIAN_POINT('',(434.117682149752,326.0163089938,392.450702781548));
#60540=CARTESIAN_POINT('Ctrl Pts',(434.117682149764,326.016308993792,392.450702781526));
#60541=CARTESIAN_POINT('Ctrl Pts',(433.477077071517,326.386162508165,393.560263324638));
#60542=CARTESIAN_POINT('Ctrl Pts',(432.916305173029,326.480565703216,394.531548744275));
#60543=CARTESIAN_POINT('Ctrl Pts',(432.092825822242,326.480565703216,395.957856818821));
#60544=CARTESIAN_POINT('Ctrl Pts',(431.532053923755,326.386162508165,396.929142238459));
#60545=CARTESIAN_POINT('Ctrl Pts',(430.891448845507,326.016308993792,398.03870278157));
#60546=CARTESIAN_POINT('',(434.117682149752,326.016308993799,392.450702781548));
#60547=CARTESIAN_POINT('Origin',(427.665215541288,326.062734664734,392.450702781549));
#60548=CARTESIAN_POINT('',(430.89144884552,326.0163089938,386.862702781548));
#60549=CARTESIAN_POINT('Ctrl Pts',(428.488694892075,326.480565703216,386.862702781548));
#60550=CARTESIAN_POINT('Ctrl Pts',(429.61023868905,326.386162508165,386.862702781548));
#60551=CARTESIAN_POINT('Ctrl Pts',(430.891448845545,326.016308993792,386.862702781548));
#60552=CARTESIAN_POINT('Ctrl Pts',(430.891448845507,326.016308993792,386.862702781526));
#60553=CARTESIAN_POINT('Ctrl Pts',(431.532053923755,326.386162508165,387.972263324638));
#60554=CARTESIAN_POINT('Ctrl Pts',(432.092825822242,326.480565703216,388.943548744275));
#60555=CARTESIAN_POINT('Origin',(427.665215541293,326.062734664737,392.450702781548));
#60556=CARTESIAN_POINT('Ctrl Pts',(432.916305173029,326.480565703216,390.369856818821));
#60557=CARTESIAN_POINT('Ctrl Pts',(433.477077071517,326.386162508165,391.341142238458));
#60558=CARTESIAN_POINT('Ctrl Pts',(434.117682149764,326.016308993792,392.45070278157));
#60559=CARTESIAN_POINT('Origin',(427.665215541288,326.062734664734,392.450702781548));
#60560=CARTESIAN_POINT('Origin',(427.665215541289,326.062734664734,392.450702781548));
#60561=CARTESIAN_POINT('',(421.212748932825,326.016308993799,392.450702781548));
#60562=CARTESIAN_POINT('Ctrl Pts',(422.414125909548,326.480565703216,394.531548744275));
#60563=CARTESIAN_POINT('Ctrl Pts',(421.85335401106,326.386162508165,393.560263324638));
#60564=CARTESIAN_POINT('Ctrl Pts',(421.212748932812,326.016308993791,392.450702781526));
#60565=CARTESIAN_POINT('Ctrl Pts',(421.212748932812,326.016308993791,392.45070278157));
#60566=CARTESIAN_POINT('Ctrl Pts',(421.85335401106,326.386162508165,391.341142238459));
#60567=CARTESIAN_POINT('Ctrl Pts',(422.414125909547,326.480565703216,390.369856818821));
#60568=CARTESIAN_POINT('Origin',(427.665215541289,326.062734664734,392.450702781548));
#60569=CARTESIAN_POINT('Ctrl Pts',(424.438982237069,326.016308993792,398.03870278157));
#60570=CARTESIAN_POINT('Ctrl Pts',(423.798377158822,326.386162508165,396.929142238459));
#60571=CARTESIAN_POINT('Ctrl Pts',(423.237605260334,326.480565703216,395.957856818821));
#60572=CARTESIAN_POINT('Origin',(422.825865584941,326.498447303216,395.244702781548));
#60573=CARTESIAN_POINT('',(421.212748932825,326.016308993798,392.450702781548));
#60574=CARTESIAN_POINT('Origin',(422.825865584941,326.498447303216,389.656702781548));
#60575=CARTESIAN_POINT('',(424.438982237057,326.016308993799,386.862702781548));
#60576=CARTESIAN_POINT('Origin',(430.909330445546,323.655272903216,386.862702781548));
#60577=CARTESIAN_POINT('',(430.89144884552,326.016308993799,386.862702781548));
#60578=CARTESIAN_POINT('Origin',(432.504565497636,326.498447303216,389.656702781548));
#60579=CARTESIAN_POINT('Origin',(280.876756490954,220.460559303207,538.878400551892));
#60580=CARTESIAN_POINT('',(277.226674890954,216.828359303207,538.878400551892));
#60581=CARTESIAN_POINT('Origin',(277.226674890954,220.460559303207,538.878400551892));
#60582=CARTESIAN_POINT('Origin',(323.345556490953,220.46055930321,538.878400551891));
#60583=CARTESIAN_POINT('',(319.695474890954,216.82835930321,538.878400551891));
#60584=CARTESIAN_POINT('Origin',(319.695474890954,220.46055930321,538.878400551891));
#60585=CARTESIAN_POINT('Origin',(280.87675649095,274.105359303207,538.878400551891));
#60586=CARTESIAN_POINT('',(277.22667489095,270.473159303207,538.878400551891));
#60587=CARTESIAN_POINT('Origin',(277.22667489095,274.105359303207,538.878400551891));
#60588=CARTESIAN_POINT('Origin',(298.461074890955,194.755759303208,556.760000551892));
#60589=CARTESIAN_POINT('',(298.461074890955,197.503267143208,560.336320551892));
#60590=CARTESIAN_POINT('Origin',(298.461074890955,194.755759303208,560.336320551892));
#60591=CARTESIAN_POINT('',(298.461074890955,197.503267143208,553.183680551892));
#60592=CARTESIAN_POINT('',(298.461074890955,197.503267143208,556.760000551892));
#60593=CARTESIAN_POINT('Origin',(298.461074890955,194.755759303208,553.183680551892));
#60594=CARTESIAN_POINT('Origin',(298.461074890948,299.810159303208,556.760000551891));
#60595=CARTESIAN_POINT('',(298.461074890948,302.557667143208,560.336320551891));
#60596=CARTESIAN_POINT('Origin',(298.461074890948,299.810159303208,560.336320551891));
#60597=CARTESIAN_POINT('',(298.461074890948,302.557667143208,553.183680551891));
#60598=CARTESIAN_POINT('',(298.461074890948,302.557667143208,556.760000551891));
#60599=CARTESIAN_POINT('Origin',(298.461074890948,299.810159303208,553.183680551891));
#60600=CARTESIAN_POINT('Origin',(298.461074890952,247.282959303208,538.699584551891));
#60601=CARTESIAN_POINT('',(298.46107489095,269.108793223208,543.348800551891));
#60602=CARTESIAN_POINT('Origin',(298.461074890952,247.282959303208,543.348800551891));
#60603=CARTESIAN_POINT('',(298.46107489095,269.108793223208,538.699584551891));
#60604=CARTESIAN_POINT('Origin',(335.603414207691,284.425298619953,556.760000551891));
#60605=CARTESIAN_POINT('',(335.603414207691,288.057498619953,560.336320551891));
#60606=CARTESIAN_POINT('Origin',(335.603414207691,284.425298619953,560.336320551891));
#60607=CARTESIAN_POINT('',(335.603414207691,288.057498619953,553.183680551891));
#60608=CARTESIAN_POINT('',(335.603414207691,288.057498619953,556.760000551891));
#60609=CARTESIAN_POINT('Origin',(335.603414207691,284.425298619953,553.183680551891));
#60610=CARTESIAN_POINT('Origin',(335.603414207696,210.140619986469,556.760000551891));
#60611=CARTESIAN_POINT('',(335.603414207696,213.772819986469,560.336320551891));
#60612=CARTESIAN_POINT('Origin',(335.603414207696,210.140619986469,560.336320551892));
#60613=CARTESIAN_POINT('',(335.603414207696,213.772819986469,553.183680551891));
#60614=CARTESIAN_POINT('',(335.603414207696,213.772819986469,556.760000551891));
#60615=CARTESIAN_POINT('Origin',(335.603414207696,210.140619986469,553.183680551891));
#60616=CARTESIAN_POINT('Origin',(261.318735574212,210.140619986464,556.760000551892));
#60617=CARTESIAN_POINT('',(261.318735574212,213.772819986464,560.336320551892));
#60618=CARTESIAN_POINT('Origin',(261.318735574212,210.140619986464,560.336320551892));
#60619=CARTESIAN_POINT('',(261.318735574212,213.772819986464,553.183680551891));
#60620=CARTESIAN_POINT('',(261.318735574212,213.772819986464,556.760000551892));
#60621=CARTESIAN_POINT('Origin',(261.318735574212,210.140619986464,553.183680551892));
#60622=CARTESIAN_POINT('Origin',(261.318735574207,284.425298619948,556.760000551891));
#60623=CARTESIAN_POINT('',(261.318735574207,288.057498619948,560.336320551891));
#60624=CARTESIAN_POINT('Origin',(261.318735574207,284.425298619948,560.336320551891));
#60625=CARTESIAN_POINT('',(261.318735574207,288.057498619948,553.183680551891));
#60626=CARTESIAN_POINT('',(261.318735574207,288.057498619948,556.760000551891));
#60627=CARTESIAN_POINT('Origin',(261.318735574207,284.425298619948,553.183680551891));
#60628=CARTESIAN_POINT('Origin',(331.524498889391,292.950375595403,555.865920551891));
#60629=CARTESIAN_POINT('',(323.713038793177,284.604387432155,555.865920551891));
#60630=CARTESIAN_POINT('',(305.715314890949,291.756846928711,555.865920551891));
#60631=CARTESIAN_POINT('Origin',(298.461074890952,247.282959303207,555.865920551892));
#60632=CARTESIAN_POINT('',(326.432817338928,284.864294221222,555.865920551891));
#60633=CARTESIAN_POINT('Origin',(324.915513264712,286.381598295438,555.865920551891));
#60634=CARTESIAN_POINT('',(330.801832688819,289.233309571114,555.865920551891));
#60635=CARTESIAN_POINT('',(326.432817338928,284.864294221222,555.865920551891));
#60636=CARTESIAN_POINT('',(330.525741198797,292.500989213059,555.865920551891));
#60637=CARTESIAN_POINT('Origin',(329.284528614603,290.75061364533,555.865920551891));
#60638=CARTESIAN_POINT('',(306.366782273498,302.149277250954,555.865920551891));
#60639=CARTESIAN_POINT('Origin',(298.461074890953,247.282959303211,555.865920551892));
#60640=CARTESIAN_POINT('',(303.914962890948,300.025419782009,555.865920551891));
#60641=CARTESIAN_POINT('Origin',(306.060754890948,300.025419782009,555.865920551891));
#60642=CARTESIAN_POINT('',(303.914962890949,293.874651101354,555.865920551891));
#60643=CARTESIAN_POINT('',(303.914962890948,300.025419782009,555.865920551891));
#60644=CARTESIAN_POINT('Origin',(306.060754890949,293.874651101354,555.865920551891));
#60645=CARTESIAN_POINT('Origin',(351.010702786122,254.077967303212,558.101120551891));
#60646=CARTESIAN_POINT('',(344.814100392115,254.077967303212,560.336320551891));
#60647=CARTESIAN_POINT('',(350.992821186122,254.077967303212,560.336320551891));
#60648=CARTESIAN_POINT('',(344.814100392115,254.077967303212,560.336320551891));
#60649=CARTESIAN_POINT('',(350.992821186122,254.077967303212,555.865920551891));
#60650=CARTESIAN_POINT('',(350.992821186122,254.077967303212,555.865920551891));
#60651=CARTESIAN_POINT('',(344.814100392115,254.077967303212,555.865920551891));
#60652=CARTESIAN_POINT('',(344.814100392115,254.077967303212,555.865920551891));
#60653=CARTESIAN_POINT('',(344.814100392115,254.077967303212,555.865920551891));
#60654=CARTESIAN_POINT('Origin',(350.992821186122,256.223759303212,558.101120551891));
#60655=CARTESIAN_POINT('',(353.108193550251,256.583791341156,560.336320551891));
#60656=CARTESIAN_POINT('Origin',(350.992821186122,256.223759303212,560.336320551891));
#60657=CARTESIAN_POINT('',(353.108193550251,256.583791341156,555.865920551891));
#60658=CARTESIAN_POINT('',(353.108193550251,256.583791341156,555.865920551891));
#60659=CARTESIAN_POINT('Origin',(350.992821186122,256.223759303212,555.865920551891));
#60660=CARTESIAN_POINT('Origin',(298.461074890952,247.282959303209,558.101120551891));
#60661=CARTESIAN_POINT('',(343.679104575705,279.347625928489,560.336320551891));
#60662=CARTESIAN_POINT('Origin',(298.461074890952,247.282959303209,560.336320551891));
#60663=CARTESIAN_POINT('',(343.679104575705,279.347625928489,555.865920551891));
#60664=CARTESIAN_POINT('',(343.679104575705,279.347625928489,555.865920551891));
#60665=CARTESIAN_POINT('Origin',(298.461074890952,247.282959303209,555.865920551891));
#60666=CARTESIAN_POINT('Origin',(341.928729233069,278.106413026865,558.101120551891));
#60667=CARTESIAN_POINT('',(340.411425158853,279.623717101081,560.336320551891));
#60668=CARTESIAN_POINT('Origin',(341.928729233069,278.106413026865,560.336320551891));
#60669=CARTESIAN_POINT('',(340.411425158853,279.623717101081,555.865920551891));
#60670=CARTESIAN_POINT('',(340.411425158853,279.623717101081,555.865920551891));
#60671=CARTESIAN_POINT('Origin',(341.928729233069,278.106413026866,555.865920551891));
#60672=CARTESIAN_POINT('Origin',(338.226917483907,277.439209426135,555.848038951891));
#60673=CARTESIAN_POINT('',(336.042409808962,275.254701751189,560.336320551891));
#60674=CARTESIAN_POINT('',(340.411425158853,279.623717101081,560.336320551891));
#60675=CARTESIAN_POINT('',(336.042409808962,275.254701751189,555.865920551891));
#60676=CARTESIAN_POINT('',(336.042409808962,275.254701751189,555.865920551891));
#60677=CARTESIAN_POINT('',(340.411425158853,279.623717101081,555.865920551891));
#60678=CARTESIAN_POINT('Origin',(337.559713883178,273.737397676974,558.101120551891));
#60679=CARTESIAN_POINT('',(335.782502581966,272.53492385268,560.336320551891));
#60680=CARTESIAN_POINT('Origin',(337.559713883178,273.737397676974,560.336320551891));
#60681=CARTESIAN_POINT('',(335.782502581966,272.53492385268,555.865920551891));
#60682=CARTESIAN_POINT('',(335.782502581966,272.53492385268,555.865920551891));
#60683=CARTESIAN_POINT('Origin',(337.559713883178,273.737397676974,555.865920551891));
#60684=CARTESIAN_POINT('Origin',(298.461074890951,247.282959303208,558.101120551891));
#60685=CARTESIAN_POINT('',(342.707144718038,255.817359303211,560.336320551891));
#60686=CARTESIAN_POINT('Origin',(298.461074890951,247.282959303208,560.336320551891));
#60687=CARTESIAN_POINT('',(342.707144718038,255.817359303211,555.865920551891));
#60688=CARTESIAN_POINT('',(342.707144718038,255.817359303211,555.865920551891));
#60689=CARTESIAN_POINT('Origin',(298.461074890951,247.282959303208,555.865920551891));
#60690=CARTESIAN_POINT('Origin',(344.814100424089,256.223759303212,558.101120551891));
#60691=CARTESIAN_POINT('Origin',(344.814100424089,256.223759303212,560.336320551891));
#60692=CARTESIAN_POINT('Origin',(344.814100424089,256.223759303212,555.865920551891));
#60693=CARTESIAN_POINT('Origin',(353.29330925736,267.203234460617,555.865920551891));
#60694=CARTESIAN_POINT('Origin',(338.226917483912,217.126709180287,555.848038951891));
#60695=CARTESIAN_POINT('',(336.042409808966,219.311216855232,560.336320551891));
#60696=CARTESIAN_POINT('',(340.411425158857,214.942201505341,560.336320551891));
#60697=CARTESIAN_POINT('',(336.042409808966,219.311216855232,560.336320551891));
#60698=CARTESIAN_POINT('',(340.411425158857,214.942201505341,555.865920551891));
#60699=CARTESIAN_POINT('',(340.411425158857,214.942201505341,555.865920551891));
#60700=CARTESIAN_POINT('',(336.042409808966,219.311216855232,555.865920551891));
#60701=CARTESIAN_POINT('',(336.042409808966,219.311216855232,555.865920551891));
#60702=CARTESIAN_POINT('',(336.042409808966,219.311216855232,555.865920551891));
#60703=CARTESIAN_POINT('Origin',(341.928729233073,216.459505579557,558.101120551891));
#60704=CARTESIAN_POINT('',(343.679104471958,215.218292531622,560.336320551891));
#60705=CARTESIAN_POINT('Origin',(341.928729233073,216.459505579557,560.336320551891));
#60706=CARTESIAN_POINT('',(343.679104471958,215.218292531622,555.865920551891));
#60707=CARTESIAN_POINT('',(343.679104471958,215.218292531622,555.865920551891));
#60708=CARTESIAN_POINT('Origin',(341.928729233073,216.459505579557,555.865920551891));
#60709=CARTESIAN_POINT('Origin',(298.461074890951,247.282959303208,558.101120551891));
#60710=CARTESIAN_POINT('',(353.108193520157,237.982127088447,560.336320551891));
#60711=CARTESIAN_POINT('Origin',(298.461074890952,247.282959303209,560.336320551891));
#60712=CARTESIAN_POINT('',(353.108193520157,237.982127088447,555.865920551891));
#60713=CARTESIAN_POINT('',(353.108193520157,237.982127088447,555.865920551891));
#60714=CARTESIAN_POINT('Origin',(298.461074890952,247.282959303208,555.865920551892));
#60715=CARTESIAN_POINT('Origin',(350.992821186124,238.342159303212,558.101120551891));
#60716=CARTESIAN_POINT('',(350.992821154148,240.487951303212,560.336320551891));
#60717=CARTESIAN_POINT('Origin',(350.992821186123,238.342159303212,560.336320551891));
#60718=CARTESIAN_POINT('',(350.992821154148,240.487951303212,555.865920551891));
#60719=CARTESIAN_POINT('',(350.992821154148,240.487951303212,555.865920551891));
#60720=CARTESIAN_POINT('Origin',(350.992821186123,238.342159303212,555.865920551891));
#60721=CARTESIAN_POINT('Origin',(351.010702754149,240.487951303212,558.101120551891));
#60722=CARTESIAN_POINT('',(344.81410042409,240.487951303211,560.336320551891));
#60723=CARTESIAN_POINT('',(350.992821154148,240.487951303212,560.336320551891));
#60724=CARTESIAN_POINT('',(344.81410042409,240.487951303211,555.865920551891));
#60725=CARTESIAN_POINT('',(344.81410042409,240.487951303211,555.865920551891));
#60726=CARTESIAN_POINT('',(350.992821154148,240.487951303212,555.865920551891));
#60727=CARTESIAN_POINT('Origin',(344.81410042409,238.342159303212,558.101120551891));
#60728=CARTESIAN_POINT('',(342.707144808688,238.748559773175,560.336320551891));
#60729=CARTESIAN_POINT('Origin',(344.81410042409,238.342159303211,560.336320551891));
#60730=CARTESIAN_POINT('',(342.707144808688,238.748559773175,555.865920551891));
#60731=CARTESIAN_POINT('',(342.707144808688,238.748559773175,555.865920551891));
#60732=CARTESIAN_POINT('Origin',(344.81410042409,238.342159303211,555.865920551891));
#60733=CARTESIAN_POINT('Origin',(298.461074890952,247.282959303208,558.101120551891));
#60734=CARTESIAN_POINT('',(335.782502502643,222.030994636499,560.336320551891));
#60735=CARTESIAN_POINT('Origin',(298.461074890951,247.282959303209,560.33632055189));
#60736=CARTESIAN_POINT('',(335.782502502643,222.030994636499,555.865920551891));
#60737=CARTESIAN_POINT('',(335.782502502643,222.030994636499,555.865920551891));
#60738=CARTESIAN_POINT('Origin',(298.461074890951,247.282959303209,555.865920551889));
#60739=CARTESIAN_POINT('Origin',(337.559713883181,220.828520929449,558.101120551891));
#60740=CARTESIAN_POINT('Origin',(337.559713883181,220.828520929448,560.336320551891));
#60741=CARTESIAN_POINT('Origin',(337.559713883181,220.828520929448,555.865920551891));
#60742=CARTESIAN_POINT('Origin',(353.293309320179,227.362684172507,555.865920551891));
#60743=CARTESIAN_POINT('Origin',(303.914962890955,197.615883164736,555.848038951892));
#60744=CARTESIAN_POINT('',(303.914962890955,200.691267505063,560.336320551892));
#60745=CARTESIAN_POINT('',(303.914962890955,194.540498824408,560.336320551892));
#60746=CARTESIAN_POINT('',(303.914962890955,200.691267505063,560.336320551892));
#60747=CARTESIAN_POINT('',(303.914962890955,194.540498824408,555.865920551892));
#60748=CARTESIAN_POINT('',(303.914962890955,194.540498824408,555.865920551892));
#60749=CARTESIAN_POINT('',(303.914962890955,200.691267505063,555.865920551892));
#60750=CARTESIAN_POINT('',(303.914962890955,200.691267505063,555.865920551892));
#60751=CARTESIAN_POINT('',(303.914962890955,200.691267505063,555.865920551892));
#60752=CARTESIAN_POINT('Origin',(306.060754890955,194.540498824408,558.101120551892));
#60753=CARTESIAN_POINT('',(306.366782273506,192.416641355463,560.336320551892));
#60754=CARTESIAN_POINT('Origin',(306.060754890955,194.540498824409,560.336320551892));
#60755=CARTESIAN_POINT('',(306.366782273505,192.416641355463,555.865920551892));
#60756=CARTESIAN_POINT('',(306.366782273505,192.416641355463,555.865920551892));
#60757=CARTESIAN_POINT('Origin',(306.060754890955,194.540498824409,555.865920551892));
#60758=CARTESIAN_POINT('Origin',(298.461074890951,247.282959303211,558.101120551891));
#60759=CARTESIAN_POINT('',(330.525741516232,202.064929618455,560.336320551892));
#60760=CARTESIAN_POINT('Origin',(298.461074890951,247.282959303209,560.336320551892));
#60761=CARTESIAN_POINT('',(330.525741516232,202.064929618455,555.865920551891));
#60762=CARTESIAN_POINT('',(330.525741516232,202.064929618455,555.865920551891));
#60763=CARTESIAN_POINT('Origin',(298.461074890951,247.282959303209,555.86592055189));
#60764=CARTESIAN_POINT('Origin',(329.284528614608,203.815304961091,558.101120551892));
#60765=CARTESIAN_POINT('',(330.801832688824,205.332609035307,560.336320551892));
#60766=CARTESIAN_POINT('Origin',(329.284528614609,203.815304961091,560.336320551892));
#60767=CARTESIAN_POINT('',(330.801832688824,205.332609035307,555.865920551891));
#60768=CARTESIAN_POINT('',(330.801832688824,205.332609035307,555.865920551891));
#60769=CARTESIAN_POINT('Origin',(329.284528614609,203.815304961091,555.865920551891));
#60770=CARTESIAN_POINT('Origin',(328.617325013878,207.517116710252,555.848038951891));
#60771=CARTESIAN_POINT('',(326.432817338932,209.701624385198,560.336320551892));
#60772=CARTESIAN_POINT('',(330.801832688824,205.332609035307,560.336320551892));
#60773=CARTESIAN_POINT('',(326.432817338932,209.701624385198,555.865920551891));
#60774=CARTESIAN_POINT('',(326.432817338932,209.701624385198,555.865920551891));
#60775=CARTESIAN_POINT('',(330.801832688824,205.332609035307,555.865920551891));
#60776=CARTESIAN_POINT('Origin',(324.915513264717,208.184320310982,558.101120551891));
#60777=CARTESIAN_POINT('',(323.713039257659,209.961531488534,560.336320551892));
#60778=CARTESIAN_POINT('Origin',(324.915513264717,208.184320310982,560.336320551892));
#60779=CARTESIAN_POINT('',(323.713039257659,209.961531488534,555.865920551891));
#60780=CARTESIAN_POINT('',(323.713039257659,209.961531488534,555.865920551891));
#60781=CARTESIAN_POINT('Origin',(324.915513264717,208.184320310982,555.865920551891));
#60782=CARTESIAN_POINT('Origin',(298.461074890953,247.282959303205,558.101120551891));
#60783=CARTESIAN_POINT('',(305.715314890955,202.809071677706,560.336320551892));
#60784=CARTESIAN_POINT('Origin',(298.461074890953,247.282959303206,560.336320551891));
#60785=CARTESIAN_POINT('',(305.715314890955,202.809071677706,555.865920551892));
#60786=CARTESIAN_POINT('',(305.715314890955,202.809071677706,555.865920551892));
#60787=CARTESIAN_POINT('Origin',(298.461074890953,247.282959303206,555.865920551891));
#60788=CARTESIAN_POINT('Origin',(306.060754890955,200.691267505063,558.101120551892));
#60789=CARTESIAN_POINT('Origin',(306.060754890955,200.691267505063,560.336320551892));
#60790=CARTESIAN_POINT('Origin',(306.060754890955,200.691267505063,555.865920551892));
#60791=CARTESIAN_POINT('Origin',(331.524498805765,201.615542844315,555.865920551891));
#60792=CARTESIAN_POINT('Origin',(277.22667489095,274.105359303207,543.795840551891));
#60793=CARTESIAN_POINT('',(277.22667489095,270.473159303207,548.713280551891));
#60794=CARTESIAN_POINT('',(277.22667489095,270.473159303207,543.795840551891));
#60795=CARTESIAN_POINT('Origin',(277.22667489095,274.105359303207,548.713280551891));
#60796=CARTESIAN_POINT('Origin',(319.695474890954,220.46055930321,543.795840551891));
#60797=CARTESIAN_POINT('',(319.695474890954,216.82835930321,548.713280551891));
#60798=CARTESIAN_POINT('',(319.695474890954,216.82835930321,543.795840551891));
#60799=CARTESIAN_POINT('Origin',(319.695474890954,220.46055930321,548.713280551891));
#60800=CARTESIAN_POINT('Origin',(277.226674890954,220.460559303207,543.795840551892));
#60801=CARTESIAN_POINT('',(277.226674890954,216.828359303207,548.713280551892));
#60802=CARTESIAN_POINT('',(277.226674890954,216.828359303207,543.795840551892));
#60803=CARTESIAN_POINT('Origin',(277.226674890954,220.460559303207,548.713280551892));
#60804=CARTESIAN_POINT('Origin',(298.461074890952,247.282959303208,558.655450151891));
#60805=CARTESIAN_POINT('',(327.384562890954,219.289859923024,560.336320551891));
#60806=CARTESIAN_POINT('',(327.38456289095,275.276058683397,560.336320551891));
#60807=CARTESIAN_POINT('Origin',(298.461074890952,247.282959303208,560.336320551891));
#60808=CARTESIAN_POINT('',(327.267168315382,275.396848266106,556.974579751891));
#60809=CARTESIAN_POINT('Origin',(308.672610372403,257.207479808827,24.496731278983));
#60810=CARTESIAN_POINT('',(327.267168315386,219.169070340315,556.974579751891));
#60811=CARTESIAN_POINT('Origin',(298.461074890952,247.282959303208,556.974579751891));
#60812=CARTESIAN_POINT('Origin',(308.657304290093,237.373317660302,24.0584227317262));
#60813=CARTESIAN_POINT('Origin',(354.723367946653,247.282959303212,556.974579751891));
#60814=CARTESIAN_POINT('',(327.267168315382,275.396848266106,556.974579751891));
#60815=CARTESIAN_POINT('Origin',(298.461074890952,247.282959303209,558.655450151891));
#60816=CARTESIAN_POINT('',(311.739002757719,285.281359303209,560.336320551891));
#60817=CARTESIAN_POINT('',(285.183147024179,285.281359303207,560.336320551891));
#60818=CARTESIAN_POINT('Origin',(298.461074890952,247.282959303206,560.336320551891));
#60819=CARTESIAN_POINT('',(284.851842766054,285.16396472764,556.974579751891));
#60820=CARTESIAN_POINT('Origin',(1528.18940949044,280.947624093096,436.288406677437));
#60821=CARTESIAN_POINT('',(312.070307015844,285.163964727641,556.974579751891));
#60822=CARTESIAN_POINT('Origin',(298.461074890952,247.282959303209,556.974579751891));
#60823=CARTESIAN_POINT('Origin',(-931.267259897731,280.947624001165,436.288406661732));
#60824=CARTESIAN_POINT('Origin',(312.088188615844,287.608609437492,556.974579751891));
#60825=CARTESIAN_POINT('',(284.851842766054,285.16396472764,556.974579751891));
#60826=CARTESIAN_POINT('Origin',(298.461074890952,247.282959303209,558.655450151891));
#60827=CARTESIAN_POINT('',(269.53758689095,275.276058683393,560.336320551891));
#60828=CARTESIAN_POINT('',(269.654981466518,275.396848266102,556.974579751891));
#60829=CARTESIAN_POINT('Origin',(288.253780195306,257.203359931411,24.3752918824331));
#60830=CARTESIAN_POINT('',(269.537586890954,219.28985992302,560.336320551892));
#60831=CARTESIAN_POINT('Origin',(298.461074890952,247.282959303208,560.336320551891));
#60832=CARTESIAN_POINT('',(269.654981466522,219.169070340311,556.974579751891));
#60833=CARTESIAN_POINT('Origin',(288.259429378608,237.368050819944,24.2135203256732));
#60834=CARTESIAN_POINT('Origin',(298.461074890951,247.282959303208,556.974579751891));
#60835=CARTESIAN_POINT('Origin',(269.67286306652,247.282959303206,556.974579751891));
#60836=CARTESIAN_POINT('',(269.654981466522,219.169070340311,556.974579751891));
#60837=CARTESIAN_POINT('Origin',(288.644076490954,218.651822053524,548.713280551891));
#60838=CARTESIAN_POINT('',(288.626194890954,209.690444803841,548.713280551892));
#60839=CARTESIAN_POINT('',(278.478386890954,209.69044480384,548.713280551892));
#60840=CARTESIAN_POINT('',(288.626194890954,209.690444803841,548.713280551892));
#60841=CARTESIAN_POINT('',(288.626194890954,218.672399303208,548.713280551891));
#60842=CARTESIAN_POINT('',(288.626194890954,218.672399303208,548.713280551891));
#60843=CARTESIAN_POINT('',(279.685394890953,227.613199303207,548.713280551891));
#60844=CARTESIAN_POINT('Origin',(279.685394890954,218.672399303207,548.713280551892));
#60845=CARTESIAN_POINT('',(269.943472391586,227.613199303206,548.713280551891));
#60846=CARTESIAN_POINT('',(269.943472391586,227.613199303206,548.713280551891));
#60847=CARTESIAN_POINT('',(269.943472391587,218.225359303206,548.713280551892));
#60848=CARTESIAN_POINT('',(269.943472391587,218.225359303206,548.713280551892));
#60849=CARTESIAN_POINT('Origin',(278.478386890954,218.225359303207,548.713280551892));
#60850=CARTESIAN_POINT('Origin',(288.64407649095,275.914096552891,548.713280551891));
#60851=CARTESIAN_POINT('',(278.478386890949,284.875473802573,548.713280551891));
#60852=CARTESIAN_POINT('',(288.626194890949,284.875473802574,548.713280551891));
#60853=CARTESIAN_POINT('',(278.478386890949,284.875473802574,548.713280551891));
#60854=CARTESIAN_POINT('',(269.943472391583,276.340559303206,548.713280551891));
#60855=CARTESIAN_POINT('Origin',(278.47838689095,276.340559303207,548.713280551891));
#60856=CARTESIAN_POINT('',(269.943472391583,266.952719303206,548.713280551891));
#60857=CARTESIAN_POINT('',(269.943472391583,266.952719303206,548.713280551891));
#60858=CARTESIAN_POINT('',(279.68539489095,266.952719303207,548.713280551891));
#60859=CARTESIAN_POINT('',(279.68539489095,266.952719303207,548.713280551891));
#60860=CARTESIAN_POINT('',(288.62619489095,275.893519303208,548.713280551891));
#60861=CARTESIAN_POINT('Origin',(279.68539489095,275.893519303207,548.713280551891));
#60862=CARTESIAN_POINT('',(288.626194890949,284.875473802574,548.713280551891));
#60863=CARTESIAN_POINT('Origin',(326.996558990316,275.914096552894,548.713280551891));
#60864=CARTESIAN_POINT('',(326.978677390316,276.34055930321,548.713280551891));
#60865=CARTESIAN_POINT('',(326.978677390317,266.95271930321,548.713280551891));
#60866=CARTESIAN_POINT('',(326.978677390316,276.34055930321,548.713280551891));
#60867=CARTESIAN_POINT('',(318.443762890949,284.875473802576,548.713280551891));
#60868=CARTESIAN_POINT('Origin',(318.44376289095,276.34055930321,548.713280551891));
#60869=CARTESIAN_POINT('',(308.295954890949,284.875473802576,548.713280551891));
#60870=CARTESIAN_POINT('',(308.295954890949,284.875473802576,548.713280551891));
#60871=CARTESIAN_POINT('',(308.29595489095,275.893519303209,548.713280551891));
#60872=CARTESIAN_POINT('',(308.29595489095,275.893519303209,548.713280551891));
#60873=CARTESIAN_POINT('',(317.23675489095,266.95271930321,548.713280551891));
#60874=CARTESIAN_POINT('Origin',(317.23675489095,275.89351930321,548.713280551891));
#60875=CARTESIAN_POINT('',(326.978677390317,266.95271930321,548.713280551891));
#60876=CARTESIAN_POINT('',(322.550443684267,270.107056728403,548.713280551891));
#60877=CARTESIAN_POINT('Origin',(319.69547489095,274.10535930321,548.713280551891));
#60878=CARTESIAN_POINT('Origin',(298.461074890956,247.282959303207,559.796751782383));
#60879=CARTESIAN_POINT('',(264.689833477746,294.578622153519,560.336320551894));
#60880=CARTESIAN_POINT('Origin',(298.461074890952,247.282959303208,560.336320551891));
#60881=CARTESIAN_POINT('',(264.74456349207,294.501974325459,554.940632856795));
#60882=CARTESIAN_POINT('',(264.695306479179,294.570957370713,559.796751782384));
#60883=CARTESIAN_POINT('',(298.461074890956,189.261941382259,554.940632856797));
#60884=CARTESIAN_POINT('Origin',(298.461074890952,247.282959303208,554.940632856796));
#60885=CARTESIAN_POINT('Origin',(298.461074890952,247.282959303208,554.940632856796));
#60886=CARTESIAN_POINT('Origin',(280.594960810809,284.397922553604,536.282915140689));
#60887=CARTESIAN_POINT('',(276.061696911308,288.167387864213,542.153831267514));
#60888=CARTESIAN_POINT('',(276.061696911308,288.167387864213,542.153831267514));
#60889=CARTESIAN_POINT('',(267.053894329943,279.159585282847,542.153831267514));
#60890=CARTESIAN_POINT('',(267.16827489095,274.641807303206,538.878400551891));
#60891=CARTESIAN_POINT('',(267.053894329943,279.159585282847,542.153831267514));
#60892=CARTESIAN_POINT('Origin',(329.883741371816,279.879071753365,542.673535228732));
#60893=CARTESIAN_POINT('',(320.860452870589,288.167387864216,542.153831267514));
#60894=CARTESIAN_POINT('',(316.342674890949,288.053007303209,538.878400551891));
#60895=CARTESIAN_POINT('',(329.868255451956,279.159585282851,542.153831267514));
#60896=CARTESIAN_POINT('',(320.860452870589,288.167387864216,542.153831267514));
#60897=CARTESIAN_POINT('',(329.868255451956,279.159585282851,542.153831267514));
#60898=CARTESIAN_POINT('Origin',(280.594960810814,210.16799605281,536.28291514069));
#60899=CARTESIAN_POINT('',(267.053894329947,215.406333323565,542.153831267515));
#60900=CARTESIAN_POINT('',(267.053894329947,215.406333323565,542.153831267515));
#60901=CARTESIAN_POINT('',(276.061696911314,206.3985307422,542.153831267515));
#60902=CARTESIAN_POINT('',(280.579474890954,206.512911303207,538.878400551892));
#60903=CARTESIAN_POINT('',(276.061696911314,206.3985307422,542.153831267515));
#60904=CARTESIAN_POINT('Origin',(329.883741371821,214.686846853056,542.673535228733));
#60905=CARTESIAN_POINT('',(320.860452870594,206.398530742203,542.153831267515));
#60906=CARTESIAN_POINT('',(320.860452870594,206.398530742203,542.153831267515));
#60907=CARTESIAN_POINT('',(329.86825545196,215.40633332357,542.153831267514));
#60908=CARTESIAN_POINT('',(329.753874890953,219.92411130321,538.878400551891));
#60909=CARTESIAN_POINT('',(329.86825545196,215.40633332357,542.153831267514));
#60910=CARTESIAN_POINT('Origin',(269.834195526028,276.358440903206,551.842560551891));
#60911=CARTESIAN_POINT('',(269.53758689095,276.340559303206,560.336320551891));
#60912=CARTESIAN_POINT('',(269.53758689095,276.340559303206,560.336320551891));
#60913=CARTESIAN_POINT('',(269.537586890954,218.225359303206,560.336320551892));
#60914=CARTESIAN_POINT('',(269.537586890954,219.28985992302,560.336320551892));
#60915=CARTESIAN_POINT('',(269.943472391587,218.225359303206,548.713280551892));
#60916=CARTESIAN_POINT('',(270.130804161109,227.613199303206,543.348800551891));
#60917=CARTESIAN_POINT('',(269.943472391586,227.613199303206,548.713280551891));
#60918=CARTESIAN_POINT('',(270.130804161106,266.952719303206,543.348800551891));
#60919=CARTESIAN_POINT('',(270.130804161106,266.952719303206,543.348800551891));
#60920=CARTESIAN_POINT('',(270.130804161106,266.952719303206,543.348800551891));
#60921=CARTESIAN_POINT('',(269.943472391583,276.340559303206,548.713280551891));
#60922=CARTESIAN_POINT('Origin',(278.47838689095,276.340559303206,549.875584551891));
#60923=CARTESIAN_POINT('',(278.478386890949,285.281359303207,560.336320551891));
#60924=CARTESIAN_POINT('',(278.478386890949,284.875473802574,548.713280551891));
#60925=CARTESIAN_POINT('Origin',(278.47838689095,276.340559303207,560.336320551891));
#60926=CARTESIAN_POINT('Origin',(318.461644490949,284.984750668131,551.842560551891));
#60927=CARTESIAN_POINT('',(318.443762890949,285.28135930321,560.336320551891));
#60928=CARTESIAN_POINT('',(318.443762890949,285.28135930321,560.336320551891));
#60929=CARTESIAN_POINT('',(285.183147024179,285.281359303208,560.336320551891));
#60930=CARTESIAN_POINT('',(288.626194890949,284.688142033051,543.348800551891));
#60931=CARTESIAN_POINT('',(288.626194890949,284.875473802574,548.713280551891));
#60932=CARTESIAN_POINT('',(308.295954890949,284.688142033052,543.348800551891));
#60933=CARTESIAN_POINT('',(308.295954890949,284.688142033052,543.348800551891));
#60934=CARTESIAN_POINT('',(308.295954890949,284.688142033052,543.348800551891));
#60935=CARTESIAN_POINT('',(318.443762890949,284.875473802576,548.713280551891));
#60936=CARTESIAN_POINT('Origin',(318.44376289095,276.34055930321,549.875584551891));
#60937=CARTESIAN_POINT('',(327.38456289095,276.34055930321,560.336320551891));
#60938=CARTESIAN_POINT('',(326.978677390316,276.34055930321,548.713280551891));
#60939=CARTESIAN_POINT('Origin',(318.44376289095,276.34055930321,560.336320551891));
#60940=CARTESIAN_POINT('Origin',(327.087954255871,276.35844090321,551.842560551891));
#60941=CARTESIAN_POINT('',(327.384562890954,218.22535930321,560.336320551891));
#60942=CARTESIAN_POINT('',(327.384562890954,218.22535930321,560.336320551891));
#60943=CARTESIAN_POINT('',(327.38456289095,275.276058683397,560.336320551891));
#60944=CARTESIAN_POINT('',(326.791345620794,266.95271930321,543.348800551891));
#60945=CARTESIAN_POINT('',(326.978677390317,266.95271930321,548.713280551891));
#60946=CARTESIAN_POINT('',(326.791345620796,227.61319930321,543.348800551891));
#60947=CARTESIAN_POINT('',(326.791345620796,227.61319930321,543.348800551891));
#60948=CARTESIAN_POINT('',(326.978677390319,227.61319930321,548.713280551891));
#60949=CARTESIAN_POINT('',(326.791345620796,227.61319930321,543.348800551891));
#60950=CARTESIAN_POINT('',(326.97867739032,218.22535930321,548.713280551891));
#60951=CARTESIAN_POINT('',(326.978677390319,227.61319930321,548.713280551891));
#60952=CARTESIAN_POINT('',(326.97867739032,218.22535930321,548.713280551891));
#60953=CARTESIAN_POINT('Origin',(318.443762890954,218.225359303209,549.875584551891));
#60954=CARTESIAN_POINT('',(318.443762890954,209.690444803843,548.713280551891));
#60955=CARTESIAN_POINT('Origin',(318.443762890954,218.22535930321,548.713280551891));
#60956=CARTESIAN_POINT('',(318.443762890954,209.28455930321,560.336320551892));
#60957=CARTESIAN_POINT('',(318.443762890954,209.690444803843,548.713280551891));
#60958=CARTESIAN_POINT('Origin',(318.443762890954,218.22535930321,560.336320551891));
#60959=CARTESIAN_POINT('Origin',(318.461644490954,209.581167938288,551.842560551891));
#60960=CARTESIAN_POINT('',(278.478386890954,209.284559303207,560.336320551892));
#60961=CARTESIAN_POINT('',(285.183147024184,209.284559303207,560.336320551892));
#60962=CARTESIAN_POINT('',(278.478386890954,209.284559303207,560.336320551892));
#60963=CARTESIAN_POINT('',(284.851842766059,209.401953878775,556.974579751891));
#60964=CARTESIAN_POINT('Origin',(1528.1900678514,213.616412470822,436.288276072105));
#60965=CARTESIAN_POINT('',(312.070307015849,209.401953878777,556.974579751891));
#60966=CARTESIAN_POINT('',(312.070307015849,209.401953878777,556.974579751891));
#60967=CARTESIAN_POINT('',(311.739002757724,209.284559303209,560.336320551892));
#60968=CARTESIAN_POINT('Origin',(-931.267917787646,213.616412469681,436.288276099316));
#60969=CARTESIAN_POINT('',(311.739002757723,209.284559303209,560.336320551892));
#60970=CARTESIAN_POINT('',(308.295954890954,209.690444803842,548.713280551892));
#60971=CARTESIAN_POINT('',(318.443762890954,209.690444803843,548.713280551891));
#60972=CARTESIAN_POINT('',(308.295954890954,209.877776573365,543.348800551892));
#60973=CARTESIAN_POINT('',(308.295954890954,209.690444803842,548.713280551892));
#60974=CARTESIAN_POINT('',(288.626194890954,209.877776573364,543.348800551892));
#60975=CARTESIAN_POINT('',(288.626194890954,209.877776573364,543.348800551892));
#60976=CARTESIAN_POINT('',(288.626194890954,209.877776573364,543.348800551892));
#60977=CARTESIAN_POINT('',(278.478386890954,209.69044480384,548.713280551892));
#60978=CARTESIAN_POINT('Origin',(278.478386890954,218.225359303207,549.875584551892));
#60979=CARTESIAN_POINT('Origin',(278.478386890954,218.225359303207,560.336320551892));
#60980=CARTESIAN_POINT('Origin',(326.809227220795,247.28295930321,543.348800551891));
#60981=CARTESIAN_POINT('',(288.626194890954,218.672399303207,543.348800551892));
#60982=CARTESIAN_POINT('',(288.626194890954,218.672399303207,543.348800551892));
#60983=CARTESIAN_POINT('',(308.295954890954,218.672399303209,543.348800551892));
#60984=CARTESIAN_POINT('',(308.295954890954,218.672399303209,543.348800551891));
#60985=CARTESIAN_POINT('',(317.236754890953,227.613199303209,543.348800551891));
#60986=CARTESIAN_POINT('Origin',(317.236754890954,218.672399303209,543.348800551892));
#60987=CARTESIAN_POINT('',(317.236754890953,227.613199303209,543.348800551891));
#60988=CARTESIAN_POINT('',(317.23675489095,266.95271930321,543.348800551891));
#60989=CARTESIAN_POINT('',(317.23675489095,266.95271930321,543.348800551891));
#60990=CARTESIAN_POINT('',(308.29595489095,275.893519303209,543.348800551891));
#60991=CARTESIAN_POINT('Origin',(317.23675489095,275.893519303209,543.348800551891));
#60992=CARTESIAN_POINT('',(308.29595489095,275.893519303209,543.348800551891));
#60993=CARTESIAN_POINT('',(288.62619489095,275.893519303207,543.348800551891));
#60994=CARTESIAN_POINT('',(288.62619489095,275.893519303208,543.348800551891));
#60995=CARTESIAN_POINT('',(279.68539489095,266.952719303207,543.348800551891));
#60996=CARTESIAN_POINT('Origin',(279.68539489095,275.893519303207,543.348800551891));
#60997=CARTESIAN_POINT('',(279.68539489095,266.952719303207,543.348800551891));
#60998=CARTESIAN_POINT('',(279.685394890953,227.613199303207,543.348800551891));
#60999=CARTESIAN_POINT('',(279.685394890953,227.613199303207,543.348800551891));
#61000=CARTESIAN_POINT('Origin',(279.685394890954,218.672399303207,543.348800551892));
#61001=CARTESIAN_POINT('Origin',(308.295954890954,214.181422053526,543.330918951892));
#61002=CARTESIAN_POINT('',(308.295954890954,218.672399303209,548.713280551891));
#61003=CARTESIAN_POINT('',(308.295954890954,209.690444803842,548.713280551892));
#61004=CARTESIAN_POINT('',(308.295954890954,218.672399303209,548.713280551891));
#61005=CARTESIAN_POINT('Origin',(317.236754890954,218.67239930321,546.031040551891));
#61006=CARTESIAN_POINT('',(317.236754890953,227.61319930321,548.713280551891));
#61007=CARTESIAN_POINT('Origin',(317.236754890954,218.67239930321,548.713280551891));
#61008=CARTESIAN_POINT('',(317.236754890953,227.61319930321,548.713280551891));
#61009=CARTESIAN_POINT('Origin',(326.99655899032,227.61319930321,546.031040551891));
#61010=CARTESIAN_POINT('',(317.236754890953,227.61319930321,548.713280551891));
#61011=CARTESIAN_POINT('Origin',(322.107716140633,266.95271930321,543.330918951891));
#61012=CARTESIAN_POINT('',(317.23675489095,266.95271930321,548.713280551891));
#61013=CARTESIAN_POINT('Origin',(317.23675489095,275.89351930321,546.031040551891));
#61014=CARTESIAN_POINT('',(308.29595489095,275.893519303209,548.713280551891));
#61015=CARTESIAN_POINT('Origin',(308.295954890949,280.384496552892,543.330918951891));
#61016=CARTESIAN_POINT('Origin',(288.626194890949,280.384496552891,543.330918951891));
#61017=CARTESIAN_POINT('',(288.62619489095,275.893519303208,548.713280551891));
#61018=CARTESIAN_POINT('Origin',(279.68539489095,275.893519303207,546.031040551891));
#61019=CARTESIAN_POINT('',(279.68539489095,266.952719303207,548.713280551891));
#61020=CARTESIAN_POINT('Origin',(279.70327649095,266.952719303207,546.031040551891));
#61021=CARTESIAN_POINT('Origin',(274.814433641269,227.613199303207,543.330918951892));
#61022=CARTESIAN_POINT('',(279.685394890953,227.613199303207,548.713280551891));
#61023=CARTESIAN_POINT('Origin',(279.685394890954,218.672399303207,546.031040551891));
#61024=CARTESIAN_POINT('',(288.626194890954,218.672399303208,548.713280551891));
#61025=CARTESIAN_POINT('Origin',(288.626194890954,214.181422053524,543.330918951892));
#61026=CARTESIAN_POINT('Origin',(326.99655899032,218.651822053527,548.713280551891));
#61027=CARTESIAN_POINT('Origin',(298.461074890952,247.282959303208,558.655450151891));
#61028=CARTESIAN_POINT('Origin',(298.461074890952,247.28295930321,560.336320551891));
#61029=CARTESIAN_POINT('Origin',(298.461074890952,247.282959303208,556.974579751891));
#61030=CARTESIAN_POINT('Origin',(312.08818861585,206.957309168927,556.974579751891));
#61031=CARTESIAN_POINT('Origin',(245.92932859578,256.223759303205,558.101120551891));
#61032=CARTESIAN_POINT('',(243.813956261746,256.58379151797,560.336320551891));
#61033=CARTESIAN_POINT('',(245.92932859578,254.077967303205,560.336320551891));
#61034=CARTESIAN_POINT('Origin',(245.92932859578,256.223759303205,560.336320551891));
#61035=CARTESIAN_POINT('',(245.92932859578,254.077967303205,555.865920551891));
#61036=CARTESIAN_POINT('',(245.92932859578,254.077967303205,555.865920551891));
#61037=CARTESIAN_POINT('',(243.813956261746,256.58379151797,555.865920551891));
#61038=CARTESIAN_POINT('Origin',(245.92932859578,256.223759303205,555.865920551891));
#61039=CARTESIAN_POINT('',(243.813956261746,256.58379151797,555.865920551891));
#61040=CARTESIAN_POINT('Origin',(252.125930957813,254.077967303205,558.101120551891));
#61041=CARTESIAN_POINT('',(252.108049357812,254.077967303205,560.336320551891));
#61042=CARTESIAN_POINT('',(245.92932859578,254.077967303205,560.336320551891));
#61043=CARTESIAN_POINT('',(252.108049357812,254.077967303205,555.865920551891));
#61044=CARTESIAN_POINT('',(252.108049357812,254.077967303205,555.865920551891));
#61045=CARTESIAN_POINT('',(245.92932859578,254.077967303205,555.865920551891));
#61046=CARTESIAN_POINT('Origin',(252.108049357814,256.223759303204,558.101120551891));
#61047=CARTESIAN_POINT('',(254.215005063864,255.817359303205,560.336320551891));
#61048=CARTESIAN_POINT('Origin',(252.108049357813,256.223759303205,560.336320551891));
#61049=CARTESIAN_POINT('',(254.215005063864,255.817359303205,555.865920551891));
#61050=CARTESIAN_POINT('',(254.215005063864,255.817359303205,555.865920551891));
#61051=CARTESIAN_POINT('Origin',(252.108049357813,256.223759303205,555.865920551891));
#61052=CARTESIAN_POINT('Origin',(298.461074890954,247.282959303206,558.101120551891));
#61053=CARTESIAN_POINT('',(261.139646762005,272.534923205434,560.336320551891));
#61054=CARTESIAN_POINT('Origin',(298.461074890955,247.282959303206,560.336320551891));
#61055=CARTESIAN_POINT('',(261.139646762005,272.534923205434,555.865920551891));
#61056=CARTESIAN_POINT('',(261.139646762005,272.534923205434,555.865920551891));
#61057=CARTESIAN_POINT('Origin',(298.461074890955,247.282959303206,555.865920551892));
#61058=CARTESIAN_POINT('Origin',(259.362435898722,273.737397676969,558.101120551891));
#61059=CARTESIAN_POINT('',(260.879739972938,275.254701751184,560.336320551891));
#61060=CARTESIAN_POINT('Origin',(259.362435898722,273.737397676968,560.336320551891));
#61061=CARTESIAN_POINT('',(260.879739972938,275.254701751184,555.865920551891));
#61062=CARTESIAN_POINT('',(260.879739972938,275.254701751184,555.865920551891));
#61063=CARTESIAN_POINT('Origin',(259.362435898722,273.737397676968,555.865920551891));
#61064=CARTESIAN_POINT('Origin',(258.695232297992,277.43920942613,555.848038951891));
#61065=CARTESIAN_POINT('',(256.510724623046,279.623717101076,560.336320551891));
#61066=CARTESIAN_POINT('',(260.879739972938,275.254701751184,560.336320551891));
#61067=CARTESIAN_POINT('',(256.510724623046,279.623717101076,555.865920551891));
#61068=CARTESIAN_POINT('',(256.510724623046,279.623717101076,555.865920551891));
#61069=CARTESIAN_POINT('',(260.879739972938,275.254701751184,555.865920551891));
#61070=CARTESIAN_POINT('Origin',(254.993420548831,278.106413026859,558.101120551891));
#61071=CARTESIAN_POINT('',(253.243045309946,279.347626074795,560.336320551891));
#61072=CARTESIAN_POINT('Origin',(254.99342054883,278.106413026859,560.336320551891));
#61073=CARTESIAN_POINT('',(253.243045309946,279.347626074795,555.865920551891));
#61074=CARTESIAN_POINT('',(253.243045309946,279.347626074795,555.865920551891));
#61075=CARTESIAN_POINT('Origin',(254.99342054883,278.106413026859,555.865920551891));
#61076=CARTESIAN_POINT('Origin',(298.461074890961,247.282959303205,558.101120551891));
#61077=CARTESIAN_POINT('Origin',(298.46107489096,247.282959303205,560.33632055189));
#61078=CARTESIAN_POINT('Origin',(298.46107489096,247.282959303205,555.865920551891));
#61079=CARTESIAN_POINT('Origin',(262.15022814681,267.203234441337,555.865920551891));
#61080=CARTESIAN_POINT('Origin',(268.304824768025,287.048801896164,555.848038951891));
#61081=CARTESIAN_POINT('',(266.120317093079,289.23330957111,560.336320551891));
#61082=CARTESIAN_POINT('',(270.48933244297,284.864294221219,560.336320551891));
#61083=CARTESIAN_POINT('',(266.120317093079,289.23330957111,560.336320551891));
#61084=CARTESIAN_POINT('',(270.48933244297,284.864294221219,555.865920551891));
#61085=CARTESIAN_POINT('',(270.48933244297,284.864294221219,555.865920551891));
#61086=CARTESIAN_POINT('',(266.120317093079,289.23330957111,555.865920551891));
#61087=CARTESIAN_POINT('',(266.120317093079,289.23330957111,555.865920551891));
#61088=CARTESIAN_POINT('',(266.120317093079,289.23330957111,555.865920551891));
#61089=CARTESIAN_POINT('Origin',(272.006636517186,286.381598295435,558.101120551891));
#61090=CARTESIAN_POINT('',(273.209110988721,284.604387432152,560.336320551891));
#61091=CARTESIAN_POINT('Origin',(272.006636517186,286.381598295436,560.336320551891));
#61092=CARTESIAN_POINT('',(273.209110988721,284.604387432152,555.865920551891));
#61093=CARTESIAN_POINT('',(273.209110988721,284.604387432152,555.865920551891));
#61094=CARTESIAN_POINT('Origin',(272.006636517186,286.381598295436,555.865920551891));
#61095=CARTESIAN_POINT('Origin',(298.461074890949,247.282959303215,558.101120551891));
#61096=CARTESIAN_POINT('',(291.206834890949,291.75684692871,560.336320551891));
#61097=CARTESIAN_POINT('Origin',(298.461074890951,247.282959303211,560.336320551892));
#61098=CARTESIAN_POINT('',(291.206834890949,291.75684692871,555.865920551891));
#61099=CARTESIAN_POINT('',(291.206834890949,291.75684692871,555.865920551891));
#61100=CARTESIAN_POINT('Origin',(298.461074890951,247.282959303211,555.865920551891));
#61101=CARTESIAN_POINT('Origin',(290.861394890949,293.874651101353,558.101120551891));
#61102=CARTESIAN_POINT('',(293.007186890949,293.874651101353,560.336320551891));
#61103=CARTESIAN_POINT('Origin',(290.861394890949,293.874651101353,560.336320551891));
#61104=CARTESIAN_POINT('',(293.007186890949,293.874651101353,555.865920551891));
#61105=CARTESIAN_POINT('',(293.007186890949,293.874651101353,555.865920551891));
#61106=CARTESIAN_POINT('Origin',(290.861394890949,293.874651101353,555.865920551891));
#61107=CARTESIAN_POINT('Origin',(293.007186890948,296.950035441681,555.848038951891));
#61108=CARTESIAN_POINT('',(293.007186890948,300.025419782008,560.336320551891));
#61109=CARTESIAN_POINT('',(293.007186890949,293.874651101353,560.336320551891));
#61110=CARTESIAN_POINT('',(293.007186890948,300.025419782008,555.865920551891));
#61111=CARTESIAN_POINT('',(293.007186890948,300.025419782008,555.865920551891));
#61112=CARTESIAN_POINT('',(293.007186890949,293.874651101353,555.865920551891));
#61113=CARTESIAN_POINT('Origin',(290.861394890948,300.025419782008,558.101120551891));
#61114=CARTESIAN_POINT('',(290.555367685928,302.149277276534,560.336320551891));
#61115=CARTESIAN_POINT('Origin',(290.861394890948,300.025419782008,560.336320551891));
#61116=CARTESIAN_POINT('',(290.555367685928,302.149277276534,555.865920551891));
#61117=CARTESIAN_POINT('',(290.555367685928,302.149277276534,555.865920551891));
#61118=CARTESIAN_POINT('Origin',(290.861394890948,300.025419782008,555.865920551891));
#61119=CARTESIAN_POINT('Origin',(298.461074890954,247.282959303205,558.101120551891));
#61120=CARTESIAN_POINT('',(266.396408265671,292.500988987961,560.336320551891));
#61121=CARTESIAN_POINT('Origin',(298.461074890952,247.282959303207,560.336320551891));
#61122=CARTESIAN_POINT('',(266.396408265671,292.500988987961,555.865920551891));
#61123=CARTESIAN_POINT('',(266.396408265671,292.500988987961,555.865920551891));
#61124=CARTESIAN_POINT('Origin',(298.461074890952,247.282959303207,555.865920551891));
#61125=CARTESIAN_POINT('Origin',(267.637621167297,290.750613645327,558.101120551891));
#61126=CARTESIAN_POINT('Origin',(267.637621167294,290.750613645326,560.336320551891));
#61127=CARTESIAN_POINT('Origin',(267.637621167294,290.750613645326,555.865920551891));
#61128=CARTESIAN_POINT('Origin',(293.025068490949,292.95037556378,555.865920551891));
#61129=CARTESIAN_POINT('Origin',(298.461074890946,247.282959303207,558.101120551891));
#61130=CARTESIAN_POINT('',(243.813956261747,237.98212708844,560.336320551892));
#61131=CARTESIAN_POINT('',(253.243045206199,215.218292677928,560.336320551892));
#61132=CARTESIAN_POINT('Origin',(298.461074890947,247.282959303207,560.336320551892));
#61133=CARTESIAN_POINT('',(253.243045206199,215.218292677928,555.865920551892));
#61134=CARTESIAN_POINT('',(253.243045206199,215.218292677928,555.865920551892));
#61135=CARTESIAN_POINT('',(243.813956261747,237.982127088439,555.865920551891));
#61136=CARTESIAN_POINT('Origin',(298.461074890947,247.282959303207,555.865920551892));
#61137=CARTESIAN_POINT('',(243.813956261747,237.982127088439,555.865920551891));
#61138=CARTESIAN_POINT('Origin',(254.993420548834,216.459505579551,558.101120551892));
#61139=CARTESIAN_POINT('',(256.51072462305,214.942201505336,560.336320551892));
#61140=CARTESIAN_POINT('Origin',(254.993420548834,216.459505579551,560.336320551892));
#61141=CARTESIAN_POINT('',(256.51072462305,214.942201505335,555.865920551892));
#61142=CARTESIAN_POINT('',(256.51072462305,214.942201505335,555.865920551892));
#61143=CARTESIAN_POINT('Origin',(254.993420548834,216.459505579551,555.865920551892));
#61144=CARTESIAN_POINT('Origin',(258.695232297996,217.126709180281,555.848038951892));
#61145=CARTESIAN_POINT('',(260.879739972942,219.311216855227,560.336320551892));
#61146=CARTESIAN_POINT('',(256.51072462305,214.942201505336,560.336320551892));
#61147=CARTESIAN_POINT('',(260.879739972942,219.311216855227,555.865920551891));
#61148=CARTESIAN_POINT('',(260.879739972942,219.311216855227,555.865920551891));
#61149=CARTESIAN_POINT('',(256.51072462305,214.942201505335,555.865920551892));
#61150=CARTESIAN_POINT('Origin',(259.362435898725,220.828520929443,558.101120551892));
#61151=CARTESIAN_POINT('',(261.139646762008,222.030995400978,560.336320551892));
#61152=CARTESIAN_POINT('Origin',(259.362435898726,220.828520929443,560.336320551892));
#61153=CARTESIAN_POINT('',(261.139646762008,222.030995400978,555.865920551891));
#61154=CARTESIAN_POINT('',(261.139646762008,222.030995400978,555.865920551891));
#61155=CARTESIAN_POINT('Origin',(259.362435898726,220.828520929443,555.865920551891));
#61156=CARTESIAN_POINT('Origin',(298.461074890954,247.28295930321,558.101120551891));
#61157=CARTESIAN_POINT('',(254.215005063865,238.748559303205,560.336320551891));
#61158=CARTESIAN_POINT('Origin',(298.461074890955,247.282959303211,560.336320551891));
#61159=CARTESIAN_POINT('',(254.215005063865,238.748559303205,555.865920551891));
#61160=CARTESIAN_POINT('',(254.215005063865,238.748559303205,555.865920551891));
#61161=CARTESIAN_POINT('Origin',(298.461074890955,247.282959303211,555.86592055189));
#61162=CARTESIAN_POINT('Origin',(252.108049357813,238.342159303204,558.101120551891));
#61163=CARTESIAN_POINT('',(252.108049357813,240.487951303205,560.336320551891));
#61164=CARTESIAN_POINT('Origin',(252.108049357814,238.342159303206,560.336320551891));
#61165=CARTESIAN_POINT('',(252.108049357813,240.487951303205,555.865920551891));
#61166=CARTESIAN_POINT('',(252.108049357813,240.487951303205,555.865920551891));
#61167=CARTESIAN_POINT('Origin',(252.108049357814,238.342159303206,555.865920551891));
#61168=CARTESIAN_POINT('Origin',(252.125930957813,240.487951303205,558.101120551891));
#61169=CARTESIAN_POINT('',(245.929328595781,240.487951303205,560.336320551891));
#61170=CARTESIAN_POINT('',(252.108049357813,240.487951303205,560.336320551891));
#61171=CARTESIAN_POINT('',(245.929328595781,240.487951303205,555.865920551891));
#61172=CARTESIAN_POINT('',(245.929328595781,240.487951303205,555.865920551891));
#61173=CARTESIAN_POINT('',(252.108049357813,240.487951303205,555.865920551891));
#61174=CARTESIAN_POINT('Origin',(245.929328595778,238.342159303205,558.101120551891));
#61175=CARTESIAN_POINT('Origin',(245.929328595781,238.342159303205,560.336320551892));
#61176=CARTESIAN_POINT('Origin',(245.929328595781,238.342159303205,555.865920551891));
#61177=CARTESIAN_POINT('Origin',(262.150228146813,227.362684145801,555.865920551891));
#61178=CARTESIAN_POINT('Origin',(298.461074890952,247.282959303211,558.101120551891));
#61179=CARTESIAN_POINT('',(266.396408265677,202.064929618451,560.336320551892));
#61180=CARTESIAN_POINT('',(290.555367508405,192.416641355462,560.336320551892));
#61181=CARTESIAN_POINT('Origin',(298.461074890951,247.282959303207,560.33632055189));
#61182=CARTESIAN_POINT('',(290.555367508405,192.416641355462,555.865920551892));
#61183=CARTESIAN_POINT('',(290.555367508405,192.416641355462,555.865920551892));
#61184=CARTESIAN_POINT('',(266.396408265677,202.064929618451,555.865920551892));
#61185=CARTESIAN_POINT('Origin',(298.461074890951,247.282959303206,555.86592055189));
#61186=CARTESIAN_POINT('',(266.396408265677,202.064929618451,555.865920551892));
#61187=CARTESIAN_POINT('Origin',(290.861394890955,194.540498824408,558.101120551892));
#61188=CARTESIAN_POINT('',(293.007186890955,194.540498824408,560.336320551892));
#61189=CARTESIAN_POINT('Origin',(290.861394890955,194.540498824408,560.336320551892));
#61190=CARTESIAN_POINT('',(293.007186890955,194.540498824408,555.865920551892));
#61191=CARTESIAN_POINT('',(293.007186890955,194.540498824408,555.865920551892));
#61192=CARTESIAN_POINT('Origin',(290.861394890955,194.540498824408,555.865920551892));
#61193=CARTESIAN_POINT('Origin',(293.007186890955,197.615883164735,555.848038951892));
#61194=CARTESIAN_POINT('',(293.007186890955,200.691267505062,560.336320551892));
#61195=CARTESIAN_POINT('',(293.007186890955,194.540498824408,560.336320551892));
#61196=CARTESIAN_POINT('',(293.007186890955,200.691267505062,555.865920551892));
#61197=CARTESIAN_POINT('',(293.007186890955,200.691267505062,555.865920551892));
#61198=CARTESIAN_POINT('',(293.007186890955,194.540498824408,555.865920551892));
#61199=CARTESIAN_POINT('Origin',(290.861394890955,200.691267505062,558.101120551892));
#61200=CARTESIAN_POINT('',(291.206834656197,202.809071715997,560.336320551892));
#61201=CARTESIAN_POINT('Origin',(290.861394890955,200.691267505062,560.336320551892));
#61202=CARTESIAN_POINT('',(291.206834656197,202.809071715997,555.865920551892));
#61203=CARTESIAN_POINT('',(291.206834656197,202.809071715997,555.865920551892));
#61204=CARTESIAN_POINT('Origin',(290.861394890955,200.691267505062,555.865920551892));
#61205=CARTESIAN_POINT('Origin',(298.461074890951,247.282959303207,558.101120551891));
#61206=CARTESIAN_POINT('',(273.209110224242,209.961531691517,560.336320551892));
#61207=CARTESIAN_POINT('Origin',(298.461074890951,247.282959303207,560.336320551891));
#61208=CARTESIAN_POINT('',(273.209110224242,209.961531691517,555.865920551892));
#61209=CARTESIAN_POINT('',(273.209110224242,209.961531691517,555.865920551892));
#61210=CARTESIAN_POINT('Origin',(298.46107489095,247.282959303205,555.865920551891));
#61211=CARTESIAN_POINT('Origin',(272.006636517191,208.184320310979,558.101120551892));
#61212=CARTESIAN_POINT('',(270.489332442976,209.701624385194,560.336320551892));
#61213=CARTESIAN_POINT('Origin',(272.006636517192,208.184320310979,560.336320551892));
#61214=CARTESIAN_POINT('',(270.489332442976,209.701624385194,555.865920551892));
#61215=CARTESIAN_POINT('',(270.489332442976,209.701624385194,555.865920551892));
#61216=CARTESIAN_POINT('Origin',(272.006636517192,208.184320310979,555.865920551892));
#61217=CARTESIAN_POINT('Origin',(268.30482476803,207.517116710248,555.848038951892));
#61218=CARTESIAN_POINT('',(266.120317093085,205.332609035303,560.336320551892));
#61219=CARTESIAN_POINT('',(270.489332442976,209.701624385194,560.336320551892));
#61220=CARTESIAN_POINT('',(266.120317093085,205.332609035303,555.865920551892));
#61221=CARTESIAN_POINT('',(266.120317093085,205.332609035303,555.865920551892));
#61222=CARTESIAN_POINT('',(270.489332442976,209.701624385194,555.865920551892));
#61223=CARTESIAN_POINT('Origin',(267.637621167301,203.815304961088,558.101120551892));
#61224=CARTESIAN_POINT('Origin',(267.6376211673,203.815304961087,560.336320551892));
#61225=CARTESIAN_POINT('Origin',(267.6376211673,203.815304961087,555.865920551892));
#61226=CARTESIAN_POINT('Origin',(293.025068490955,201.615542736639,555.865920551892));
#61227=CARTESIAN_POINT('Origin',(298.461074890952,247.28295930321,558.101120551891));
#61228=CARTESIAN_POINT('',(323.713038793177,284.604387432155,560.336320551891));
#61229=CARTESIAN_POINT('',(305.715314890949,291.756846928711,560.336320551891));
#61230=CARTESIAN_POINT('Origin',(298.461074890952,247.282959303207,560.336320551891));
#61231=CARTESIAN_POINT('',(323.713038793177,284.604387432155,555.865920551891));
#61232=CARTESIAN_POINT('',(305.715314890949,291.756846928711,555.865920551891));
#61233=CARTESIAN_POINT('Origin',(306.060754890949,293.874651101355,558.101120551891));
#61234=CARTESIAN_POINT('',(303.914962890949,293.874651101354,560.336320551891));
#61235=CARTESIAN_POINT('Origin',(306.060754890949,293.874651101354,560.336320551891));
#61236=CARTESIAN_POINT('',(303.914962890949,293.874651101354,555.865920551891));
#61237=CARTESIAN_POINT('Origin',(303.914962890948,296.950035441682,555.848038951891));
#61238=CARTESIAN_POINT('',(303.914962890948,300.025419782009,560.336320551891));
#61239=CARTESIAN_POINT('',(303.914962890948,300.025419782009,560.336320551891));
#61240=CARTESIAN_POINT('',(303.914962890948,300.025419782009,555.865920551891));
#61241=CARTESIAN_POINT('Origin',(306.060754890948,300.025419782009,558.101120551891));
#61242=CARTESIAN_POINT('',(306.366782273498,302.149277250954,560.336320551891));
#61243=CARTESIAN_POINT('Origin',(306.060754890948,300.025419782009,560.336320551891));
#61244=CARTESIAN_POINT('',(306.366782273498,302.149277250954,555.865920551891));
#61245=CARTESIAN_POINT('Origin',(298.461074890952,247.282959303207,558.101120551891));
#61246=CARTESIAN_POINT('',(330.525741198797,292.500989213059,560.336320551891));
#61247=CARTESIAN_POINT('Origin',(298.461074890953,247.282959303211,560.336320551892));
#61248=CARTESIAN_POINT('',(330.525741198797,292.500989213059,555.865920551891));
#61249=CARTESIAN_POINT('Origin',(329.284528614603,290.75061364533,558.101120551891));
#61250=CARTESIAN_POINT('',(330.801832688819,289.233309571114,560.336320551891));
#61251=CARTESIAN_POINT('Origin',(329.284528614603,290.75061364533,560.336320551891));
#61252=CARTESIAN_POINT('',(330.801832688819,289.233309571114,555.865920551891));
#61253=CARTESIAN_POINT('Origin',(324.915513264711,286.381598295438,558.101120551891));
#61254=CARTESIAN_POINT('',(326.432817338928,284.864294221223,560.336320551891));
#61255=CARTESIAN_POINT('Origin',(324.915513264712,286.381598295438,560.336320551891));
#61256=CARTESIAN_POINT('',(326.432817338928,284.864294221222,555.865920551891));
#61257=CARTESIAN_POINT('Origin',(328.617325013873,287.048801896168,555.848038951891));
#61258=CARTESIAN_POINT('',(326.432817338928,284.864294221223,560.336320551891));
#61259=CARTESIAN_POINT('Origin',(298.461074890952,247.282959303208,554.971840551891));
#61260=CARTESIAN_POINT('',(298.461074890956,191.04982903683,553.183680551892));
#61261=CARTESIAN_POINT('Origin',(298.461074890956,191.049829036829,554.971840551892));
#61262=CARTESIAN_POINT('Origin',(298.461074890952,247.282959303208,553.183680551891));
#61263=CARTESIAN_POINT('Origin',(354.71208675733,247.282959303212,553.183680551891));
#61264=CARTESIAN_POINT('',(266.668723505555,279.319128262139,553.183680551891));
#61265=CARTESIAN_POINT('',(266.668723505559,215.246790344273,553.183680551891));
#61266=CARTESIAN_POINT('',(266.668723505555,279.319128262139,553.183680551891));
#61267=CARTESIAN_POINT('',(275.902153932022,206.013359917812,553.183680551892));
#61268=CARTESIAN_POINT('',(266.668723505559,215.246790344273,553.183680551891));
#61269=CARTESIAN_POINT('',(321.019995849888,206.013359917815,553.183680551891));
#61270=CARTESIAN_POINT('',(275.902153932022,206.013359917812,553.183680551892));
#61271=CARTESIAN_POINT('',(330.253426276349,215.246790344278,553.183680551891));
#61272=CARTESIAN_POINT('',(321.019995849888,206.013359917815,553.183680551891));
#61273=CARTESIAN_POINT('',(330.253426276344,279.319128262143,553.183680551891));
#61274=CARTESIAN_POINT('',(330.253426276349,215.246790344278,553.183680551891));
#61275=CARTESIAN_POINT('',(321.019995849882,288.552558688605,553.183680551891));
#61276=CARTESIAN_POINT('',(330.253426276344,279.319128262143,553.183680551891));
#61277=CARTESIAN_POINT('',(275.902153932016,288.552558688602,553.183680551891));
#61278=CARTESIAN_POINT('',(321.019995849882,288.552558688605,553.183680551891));
#61279=CARTESIAN_POINT('',(275.902153932016,288.552558688602,553.183680551891));
#61280=CARTESIAN_POINT('Origin',(271.558236896863,283.663045297292,542.135960560502));
#61281=CARTESIAN_POINT('',(266.668723505555,279.319128262139,553.183680551891));
#61282=CARTESIAN_POINT('',(275.902153932016,288.552558688602,553.183680551891));
#61283=CARTESIAN_POINT('Origin',(325.363912885035,283.663045297296,542.135960560501));
#61284=CARTESIAN_POINT('',(321.019995849882,288.552558688605,553.183680551891));
#61285=CARTESIAN_POINT('',(330.253426276344,279.319128262143,553.183680551891));
#61286=CARTESIAN_POINT('Origin',(321.037877449882,288.302782995907,546.031040551891));
#61287=CARTESIAN_POINT('Origin',(321.037877449888,206.263135610512,546.031040551891));
#61288=CARTESIAN_POINT('',(321.019995849888,206.013359917815,553.183680551891));
#61289=CARTESIAN_POINT('',(275.902153932022,206.013359917812,553.183680551892));
#61290=CARTESIAN_POINT('Origin',(271.558236896869,210.902873309121,542.135960560502));
#61291=CARTESIAN_POINT('',(266.668723505559,215.246790344273,553.183680551891));
#61292=CARTESIAN_POINT('Origin',(356.594156490952,247.282959303212,560.336320551891));
#61293=CARTESIAN_POINT('Origin',(330.003650583647,279.337009862143,546.031040551891));
#61294=CARTESIAN_POINT('',(330.253426276349,215.246790344278,553.183680551891));
#61295=CARTESIAN_POINT('Origin',(266.918499198253,279.337009862139,546.031040551891));
#61296=CARTESIAN_POINT('Origin',(325.36391288504,210.902873309124,542.135960560502));
#61297=CARTESIAN_POINT('Origin',(327.864997019629,247.28295930321,538.878400551891));
#61298=CARTESIAN_POINT('Origin',(319.69547489095,274.10535930321,552.727699751891));
#61299=CARTESIAN_POINT('',(319.69547489095,279.13008890321,552.682995751891));
#61300=CARTESIAN_POINT('',(322.615388379292,278.194615075807,552.682995751891));
#61301=CARTESIAN_POINT('Origin',(319.69547489095,274.10535930321,552.682995751891));
#61302=CARTESIAN_POINT('Origin',(319.69547489095,274.10535930321,552.682995751891));
#61303=CARTESIAN_POINT('',(322.35560959919,277.830802284651,553.130035751891));
#61304=CARTESIAN_POINT('',(322.589410501282,278.158233796692,552.727699751891));
#61305=CARTESIAN_POINT('Origin',(319.69547489095,274.10535930321,553.130035751891));
#61306=CARTESIAN_POINT('Origin',(319.69547489095,274.10535930321,550.754018151891));
#61307=CARTESIAN_POINT('',(319.69547489095,279.13008890321,548.825040551891));
#61308=CARTESIAN_POINT('',(319.69547489095,279.13008890321,550.754018151891));
#61309=CARTESIAN_POINT('',(322.615388379293,270.016103530613,548.825040551891));
#61310=CARTESIAN_POINT('Origin',(319.69547489095,274.10535930321,548.825040551891));
#61311=CARTESIAN_POINT('Origin',(319.69547489095,274.10535930321,548.825040551891));
#61312=CARTESIAN_POINT('Origin',(319.69547489095,274.10535930321,548.813864551891));
#61313=CARTESIAN_POINT('',(322.60889390979,270.025198850392,548.813864551891));
#61314=CARTESIAN_POINT('Origin',(316.89700449095,274.10535930321,553.147917351891));
#61315=CARTESIAN_POINT('',(316.89700449095,275.721056941969,553.130035751891));
#61316=CARTESIAN_POINT('',(316.89700449095,272.489661664451,553.130035751891));
#61317=CARTESIAN_POINT('',(316.89700449095,275.721056941969,553.130035751891));
#61318=CARTESIAN_POINT('',(316.89700449095,272.48966166445,550.984243751891));
#61319=CARTESIAN_POINT('',(316.89700449095,272.48966166445,550.984243751891));
#61320=CARTESIAN_POINT('',(316.89700449095,275.721056941969,550.984243751891));
#61321=CARTESIAN_POINT('',(316.89700449095,275.721056941969,550.984243751891));
#61322=CARTESIAN_POINT('',(316.89700449095,275.721056941969,550.984243751891));
#61323=CARTESIAN_POINT('Origin',(318.29623969095,271.681812845071,553.147917351891));
#61324=CARTESIAN_POINT('',(319.69547489095,270.873964025691,553.130035751891));
#61325=CARTESIAN_POINT('',(316.89700449095,272.489661664451,553.130035751891));
#61326=CARTESIAN_POINT('',(319.69547489095,270.873964025691,550.984243751891));
#61327=CARTESIAN_POINT('',(319.69547489095,270.873964025691,550.984243751891));
#61328=CARTESIAN_POINT('',(316.89700449095,272.48966166445,550.984243751891));
#61329=CARTESIAN_POINT('Origin',(321.09471009095,271.681812845071,553.147917351891));
#61330=CARTESIAN_POINT('',(322.49394529095,272.489661664451,553.130035751891));
#61331=CARTESIAN_POINT('',(319.69547489095,270.873964025691,553.130035751891));
#61332=CARTESIAN_POINT('',(322.49394529095,272.489661664451,550.984243751891));
#61333=CARTESIAN_POINT('',(322.49394529095,272.489661664451,550.984243751891));
#61334=CARTESIAN_POINT('',(319.69547489095,270.873964025691,550.984243751891));
#61335=CARTESIAN_POINT('Origin',(322.49394529095,274.10535930321,553.147917351891));
#61336=CARTESIAN_POINT('',(322.49394529095,275.721056941969,553.130035751891));
#61337=CARTESIAN_POINT('',(322.49394529095,275.721056941969,553.130035751891));
#61338=CARTESIAN_POINT('',(322.49394529095,275.721056941969,550.984243751891));
#61339=CARTESIAN_POINT('',(322.49394529095,275.721056941969,550.984243751891));
#61340=CARTESIAN_POINT('',(322.49394529095,272.489661664451,550.984243751891));
#61341=CARTESIAN_POINT('Origin',(321.09471009095,276.528905761349,553.147917351891));
#61342=CARTESIAN_POINT('',(319.69547489095,277.336754580728,553.130035751891));
#61343=CARTESIAN_POINT('',(322.49394529095,275.721056941969,553.130035751891));
#61344=CARTESIAN_POINT('',(319.69547489095,277.336754580728,550.984243751891));
#61345=CARTESIAN_POINT('',(319.69547489095,277.336754580728,550.984243751891));
#61346=CARTESIAN_POINT('',(322.49394529095,275.721056941969,550.984243751891));
#61347=CARTESIAN_POINT('Origin',(316.87912289095,274.10535930321,550.984243751891));
#61348=CARTESIAN_POINT('',(319.69547489095,277.336754580728,550.984243751891));
#61349=CARTESIAN_POINT('Origin',(318.29623969095,276.528905761349,553.147917351891));
#61350=CARTESIAN_POINT('',(319.69547489095,277.336754580728,553.130035751891));
#61351=CARTESIAN_POINT('Origin',(315.09990369095,274.10535930321,553.130035751891));
#61352=CARTESIAN_POINT('',(0.,0.,0.));
#61353=CARTESIAN_POINT('Origin',(375.115917770965,45.027992731211,445.000000551893));
#61354=CARTESIAN_POINT('',(387.115917770965,45.027992731212,445.000000551893));
#61355=CARTESIAN_POINT('Origin',(375.115917770965,45.027992731211,445.000000551893));
#61356=CARTESIAN_POINT('',(387.115917770961,95.027992731212,445.000000551892));
#61357=CARTESIAN_POINT('',(387.115917770965,45.0279927312119,445.000000551893));
#61358=CARTESIAN_POINT('Origin',(375.115917770961,95.027992731211,445.000000551892));
#61359=CARTESIAN_POINT('',(378.505667770963,70.0279927312109,456.511281755021));
#61360=CARTESIAN_POINT('Ctrl Pts',(378.505667770963,70.0279927312112,456.511281755021));
#61361=CARTESIAN_POINT('Ctrl Pts',(378.505667770963,69.599793305891,456.511281755021));
#61362=CARTESIAN_POINT('Ctrl Pts',(378.419612733572,69.1447595869222,456.537670683632));
#61363=CARTESIAN_POINT('Ctrl Pts',(378.07298028749,68.3103537068892,456.631338076663));
#61364=CARTESIAN_POINT('Ctrl Pts',(377.812518336597,67.9307628737902,456.697089455795));
#61365=CARTESIAN_POINT('Ctrl Pts',(377.213217098769,67.331461635963,456.819257533707));
#61366=CARTESIAN_POINT('Ctrl Pts',(376.833597772799,67.0709457470152,456.883844434558));
#61367=CARTESIAN_POINT('Ctrl Pts',(375.999089280567,66.7242736548161,456.974814875745));
#61368=CARTESIAN_POINT('Ctrl Pts',(375.544017934913,66.6382427312109,457.000000551892));
#61369=CARTESIAN_POINT('Ctrl Pts',(374.687817607014,66.6382427312109,457.000000551892));
#61370=CARTESIAN_POINT('Ctrl Pts',(374.23274626136,66.724273654816,456.974814875745));
#61371=CARTESIAN_POINT('Ctrl Pts',(373.398237769128,67.0709457470149,456.883844434558));
#61372=CARTESIAN_POINT('Ctrl Pts',(373.018618443157,67.3314616359627,456.819257533707));
#61373=CARTESIAN_POINT('Ctrl Pts',(372.41931720533,67.9307628737898,456.697089455795));
#61374=CARTESIAN_POINT('Ctrl Pts',(372.158855254436,68.3103537068888,456.631338076663));
#61375=CARTESIAN_POINT('Ctrl Pts',(371.812222808355,69.1447595869217,456.537670683632));
#61376=CARTESIAN_POINT('Ctrl Pts',(371.726167770963,69.5997933058905,456.511281755021));
#61377=CARTESIAN_POINT('Ctrl Pts',(371.726167770963,70.4561921565308,456.511281755021));
#61378=CARTESIAN_POINT('Ctrl Pts',(371.812222808355,70.9112258754996,456.537670683632));
#61379=CARTESIAN_POINT('Ctrl Pts',(372.158855254436,71.7456317555326,456.631338076663));
#61380=CARTESIAN_POINT('Ctrl Pts',(372.41931720533,72.1252225886316,456.697089455795));
#61381=CARTESIAN_POINT('Ctrl Pts',(373.018618443157,72.7245238264588,456.819257533707));
#61382=CARTESIAN_POINT('Ctrl Pts',(373.398237769127,72.9850397154067,456.883844434558));
#61383=CARTESIAN_POINT('Ctrl Pts',(374.232746261359,73.3317118076057,456.974814875745));
#61384=CARTESIAN_POINT('Ctrl Pts',(374.687817607013,73.4177427312109,457.000000551892));
#61385=CARTESIAN_POINT('Ctrl Pts',(375.544017934912,73.417742731211,457.000000551892));
#61386=CARTESIAN_POINT('Ctrl Pts',(375.999089280567,73.3317118076058,456.974814875745));
#61387=CARTESIAN_POINT('Ctrl Pts',(376.833597772799,72.9850397154069,456.883844434557));
#61388=CARTESIAN_POINT('Ctrl Pts',(377.213217098769,72.7245238264592,456.819257533707));
#61389=CARTESIAN_POINT('Ctrl Pts',(377.812518336596,72.125222588632,456.697089455795));
#61390=CARTESIAN_POINT('Ctrl Pts',(378.07298028749,71.7456317555331,456.631338076663));
#61391=CARTESIAN_POINT('Ctrl Pts',(378.419612733571,70.9112258755002,456.537670683632));
#61392=CARTESIAN_POINT('Ctrl Pts',(378.505667770963,70.4561921565313,456.511281755021));
#61393=CARTESIAN_POINT('Ctrl Pts',(378.505667770963,70.0279927312112,456.511281755021));
#61394=CARTESIAN_POINT('',(378.505667770964,55.027992731211,456.511281755021));
#61395=CARTESIAN_POINT('Ctrl Pts',(378.505667770964,55.0279927312112,456.511281755021));
#61396=CARTESIAN_POINT('Ctrl Pts',(378.505667770964,54.5997933058911,456.511281755021));
#61397=CARTESIAN_POINT('Ctrl Pts',(378.419612733573,54.1447595869223,456.537670683633));
#61398=CARTESIAN_POINT('Ctrl Pts',(378.072980287491,53.3103537068893,456.631338076663));
#61399=CARTESIAN_POINT('Ctrl Pts',(377.812518336598,52.9307628737903,456.697089455795));
#61400=CARTESIAN_POINT('Ctrl Pts',(377.213217098771,52.331461635963,456.819257533707));
#61401=CARTESIAN_POINT('Ctrl Pts',(376.8335977728,52.0709457470152,456.883844434558));
#61402=CARTESIAN_POINT('Ctrl Pts',(375.999089280568,51.7242736548162,456.974814875745));
#61403=CARTESIAN_POINT('Ctrl Pts',(375.544017934914,51.638242731211,457.000000551893));
#61404=CARTESIAN_POINT('Ctrl Pts',(374.687817607015,51.6382427312109,457.000000551893));
#61405=CARTESIAN_POINT('Ctrl Pts',(374.232746261361,51.7242736548161,456.974814875745));
#61406=CARTESIAN_POINT('Ctrl Pts',(373.398237769129,52.070945747015,456.883844434558));
#61407=CARTESIAN_POINT('Ctrl Pts',(373.018618443158,52.3314616359627,456.819257533707));
#61408=CARTESIAN_POINT('Ctrl Pts',(372.419317205331,52.9307628737898,456.697089455795));
#61409=CARTESIAN_POINT('Ctrl Pts',(372.158855254437,53.3103537068888,456.631338076663));
#61410=CARTESIAN_POINT('Ctrl Pts',(371.812222808356,54.1447595869217,456.537670683633));
#61411=CARTESIAN_POINT('Ctrl Pts',(371.726167770964,54.5997933058906,456.511281755021));
#61412=CARTESIAN_POINT('Ctrl Pts',(371.726167770964,55.4561921565308,456.511281755021));
#61413=CARTESIAN_POINT('Ctrl Pts',(371.812222808356,55.9112258754996,456.537670683633));
#61414=CARTESIAN_POINT('Ctrl Pts',(372.158855254437,56.7456317555326,456.631338076663));
#61415=CARTESIAN_POINT('Ctrl Pts',(372.419317205331,57.1252225886316,456.697089455795));
#61416=CARTESIAN_POINT('Ctrl Pts',(373.018618443158,57.7245238264589,456.819257533707));
#61417=CARTESIAN_POINT('Ctrl Pts',(373.398237769128,57.9850397154067,456.883844434558));
#61418=CARTESIAN_POINT('Ctrl Pts',(374.23274626136,58.3317118076057,456.974814875745));
#61419=CARTESIAN_POINT('Ctrl Pts',(374.687817607015,58.4177427312109,457.000000551893));
#61420=CARTESIAN_POINT('Ctrl Pts',(375.544017934913,58.417742731211,457.000000551893));
#61421=CARTESIAN_POINT('Ctrl Pts',(375.999089280568,58.3317118076058,456.974814875745));
#61422=CARTESIAN_POINT('Ctrl Pts',(376.8335977728,57.9850397154069,456.883844434558));
#61423=CARTESIAN_POINT('Ctrl Pts',(377.21321709877,57.7245238264592,456.819257533707));
#61424=CARTESIAN_POINT('Ctrl Pts',(377.812518336597,57.125222588632,456.697089455795));
#61425=CARTESIAN_POINT('Ctrl Pts',(378.072980287491,56.7456317555331,456.631338076663));
#61426=CARTESIAN_POINT('Ctrl Pts',(378.419612733572,55.9112258755001,456.537670683633));
#61427=CARTESIAN_POINT('Ctrl Pts',(378.505667770964,55.4561921565313,456.511281755021));
#61428=CARTESIAN_POINT('Ctrl Pts',(378.505667770964,55.0279927312112,456.511281755021));
#61429=CARTESIAN_POINT('Origin',(375.115917770959,129.966587529218,473.546231028847));
#61430=CARTESIAN_POINT('',(379.378917770959,129.966587529218,467.092461505801));
#61431=CARTESIAN_POINT('Ctrl Pts',(379.378917770959,129.966587529218,467.092461505801));
#61432=CARTESIAN_POINT('Ctrl Pts',(379.378917770959,130.503268746603,467.092461505801));
#61433=CARTESIAN_POINT('Ctrl Pts',(379.271395654013,131.074810160741,467.114043744988));
#61434=CARTESIAN_POINT('Ctrl Pts',(378.83594383252,132.124725811365,467.191447285196));
#61435=CARTESIAN_POINT('Ctrl Pts',(378.508082726548,132.603214990025,467.246090869443));
#61436=CARTESIAN_POINT('Ctrl Pts',(377.752562213622,133.358735502951,467.348231142275));
#61437=CARTESIAN_POINT('Ctrl Pts',(377.274065797272,133.686609917986,467.402443514309));
#61438=CARTESIAN_POINT('Ctrl Pts',(376.224125087311,134.122071395634,467.478855729964));
#61439=CARTESIAN_POINT('Ctrl Pts',(375.652574862886,134.229587529218,467.500000551892));
#61440=CARTESIAN_POINT('Ctrl Pts',(374.579260679031,134.229587529218,467.500000551892));
#61441=CARTESIAN_POINT('Ctrl Pts',(374.007710454606,134.122071395634,467.478855729964));
#61442=CARTESIAN_POINT('Ctrl Pts',(372.957769744645,133.686609917986,467.402443514309));
#61443=CARTESIAN_POINT('Ctrl Pts',(372.479273328295,133.35873550295,467.348231142275));
#61444=CARTESIAN_POINT('Ctrl Pts',(371.723752815369,132.603214990025,467.246090869443));
#61445=CARTESIAN_POINT('Ctrl Pts',(371.395891709397,132.124725811364,467.191447285196));
#61446=CARTESIAN_POINT('Ctrl Pts',(370.960439887904,131.074810160741,467.114043744988));
#61447=CARTESIAN_POINT('Ctrl Pts',(370.852917770959,130.503268746602,467.092461505801));
#61448=CARTESIAN_POINT('Ctrl Pts',(370.852917770959,129.429906311833,467.092461505801));
#61449=CARTESIAN_POINT('Ctrl Pts',(370.960439887905,128.858364897694,467.114043744988));
#61450=CARTESIAN_POINT('Ctrl Pts',(371.395891709398,127.808449247071,467.191447285196));
#61451=CARTESIAN_POINT('Ctrl Pts',(371.723752815369,127.329960068411,467.246090869443));
#61452=CARTESIAN_POINT('Ctrl Pts',(372.479273328295,126.574439555485,467.348231142275));
#61453=CARTESIAN_POINT('Ctrl Pts',(372.957769744646,126.24656514045,467.402443514309));
#61454=CARTESIAN_POINT('Ctrl Pts',(374.007710454607,125.811103662802,467.478855729964));
#61455=CARTESIAN_POINT('Ctrl Pts',(374.579260679031,125.703587529218,467.500000551892));
#61456=CARTESIAN_POINT('Ctrl Pts',(375.652574862887,125.703587529218,467.500000551892));
#61457=CARTESIAN_POINT('Ctrl Pts',(376.224125087311,125.811103662802,467.478855729964));
#61458=CARTESIAN_POINT('Ctrl Pts',(377.274065797272,126.24656514045,467.402443514309));
#61459=CARTESIAN_POINT('Ctrl Pts',(377.752562213623,126.574439555485,467.348231142275));
#61460=CARTESIAN_POINT('Ctrl Pts',(378.508082726548,127.329960068411,467.246090869443));
#61461=CARTESIAN_POINT('Ctrl Pts',(378.83594383252,127.808449247071,467.191447285196));
#61462=CARTESIAN_POINT('Ctrl Pts',(379.271395654013,128.858364897695,467.114043744988));
#61463=CARTESIAN_POINT('Ctrl Pts',(379.378917770959,129.429906311834,467.092461505801));
#61464=CARTESIAN_POINT('Ctrl Pts',(379.378917770959,129.966587529218,467.092461505801));
#61465=CARTESIAN_POINT('',(379.378917770959,129.966587529218,479.739413773764));
#61466=CARTESIAN_POINT('',(379.378917770959,129.966587529218,473.546231028847));
#61467=CARTESIAN_POINT('Ctrl Pts',(379.378917770959,129.966587529218,479.739413773764));
#61468=CARTESIAN_POINT('Ctrl Pts',(379.378917770959,129.430742174692,479.739413773764));
#61469=CARTESIAN_POINT('Ctrl Pts',(379.27171989715,128.859547272367,479.753090630837));
#61470=CARTESIAN_POINT('Ctrl Pts',(378.836500546947,127.809391754052,479.802374391123));
#61471=CARTESIAN_POINT('Ctrl Pts',(378.508507955967,127.33038529783,479.837256921998));
#61472=CARTESIAN_POINT('Ctrl Pts',(377.752122848375,126.574000190238,479.90264400738));
#61473=CARTESIAN_POINT('Ctrl Pts',(377.273115153634,126.246005370261,479.937413294597));
#61474=CARTESIAN_POINT('Ctrl Pts',(376.22295544681,125.810784382548,479.986437599388));
#61475=CARTESIAN_POINT('Ctrl Pts',(375.651759093082,125.703587529218,480.000000551892));
#61476=CARTESIAN_POINT('Ctrl Pts',(374.580076448836,125.703587529218,480.000000551892));
#61477=CARTESIAN_POINT('Ctrl Pts',(374.008880095108,125.810784382548,479.986437599388));
#61478=CARTESIAN_POINT('Ctrl Pts',(372.958720388284,126.246005370261,479.937413294597));
#61479=CARTESIAN_POINT('Ctrl Pts',(372.479712693543,126.574000190237,479.90264400738));
#61480=CARTESIAN_POINT('Ctrl Pts',(371.723327585951,127.330385297829,479.837256921998));
#61481=CARTESIAN_POINT('Ctrl Pts',(371.395334994971,127.809391754051,479.802374391123));
#61482=CARTESIAN_POINT('Ctrl Pts',(370.960115644768,128.859547272367,479.753090630837));
#61483=CARTESIAN_POINT('Ctrl Pts',(370.852917770959,129.430742174691,479.739413773764));
#61484=CARTESIAN_POINT('Ctrl Pts',(370.852917770959,130.502432883744,479.739413773764));
#61485=CARTESIAN_POINT('Ctrl Pts',(370.960115644767,131.073627786068,479.753090630837));
#61486=CARTESIAN_POINT('Ctrl Pts',(371.39533499497,132.123783304384,479.802374391123));
#61487=CARTESIAN_POINT('Ctrl Pts',(371.723327585951,132.602789760606,479.837256921998));
#61488=CARTESIAN_POINT('Ctrl Pts',(372.479712693542,133.359174868198,479.90264400738));
#61489=CARTESIAN_POINT('Ctrl Pts',(372.958720388284,133.687169688174,479.937413294597));
#61490=CARTESIAN_POINT('Ctrl Pts',(374.008880095108,134.122390675888,479.986437599388));
#61491=CARTESIAN_POINT('Ctrl Pts',(374.580076448835,134.229587529218,480.000000551892));
#61492=CARTESIAN_POINT('Ctrl Pts',(375.651759093081,134.229587529218,480.000000551892));
#61493=CARTESIAN_POINT('Ctrl Pts',(376.222955446809,134.122390675888,479.986437599388));
#61494=CARTESIAN_POINT('Ctrl Pts',(377.273115153633,133.687169688174,479.937413294597));
#61495=CARTESIAN_POINT('Ctrl Pts',(377.752122848375,133.359174868198,479.90264400738));
#61496=CARTESIAN_POINT('Ctrl Pts',(378.508507955966,132.602789760607,479.837256921998));
#61497=CARTESIAN_POINT('Ctrl Pts',(378.836500546947,132.123783304385,479.802374391123));
#61498=CARTESIAN_POINT('Ctrl Pts',(379.27171989715,131.073627786069,479.753090630837));
#61499=CARTESIAN_POINT('Ctrl Pts',(379.378917770959,130.502432883745,479.739413773764));
#61500=CARTESIAN_POINT('Ctrl Pts',(379.378917770959,129.966587529218,479.739413773764));
#61501=CARTESIAN_POINT('Origin',(375.11591777096,105.027992731211,473.546231028847));
#61502=CARTESIAN_POINT('',(379.37891777096,105.027992731211,467.092461505801));
#61503=CARTESIAN_POINT('Ctrl Pts',(379.37891777096,105.027992731211,467.092461505801));
#61504=CARTESIAN_POINT('Ctrl Pts',(379.37891777096,105.564673948596,467.092461505801));
#61505=CARTESIAN_POINT('Ctrl Pts',(379.271395654014,106.136215362734,467.114043744988));
#61506=CARTESIAN_POINT('Ctrl Pts',(378.835943832521,107.186131013358,467.191447285196));
#61507=CARTESIAN_POINT('Ctrl Pts',(378.50808272655,107.664620192018,467.246090869444));
#61508=CARTESIAN_POINT('Ctrl Pts',(377.752562213624,108.420140704944,467.348231142275));
#61509=CARTESIAN_POINT('Ctrl Pts',(377.274065797273,108.748015119979,467.402443514309));
#61510=CARTESIAN_POINT('Ctrl Pts',(376.224125087312,109.183476597627,467.478855729964));
#61511=CARTESIAN_POINT('Ctrl Pts',(375.652574862888,109.290992731211,467.500000551892));
#61512=CARTESIAN_POINT('Ctrl Pts',(374.579260679033,109.290992731211,467.500000551892));
#61513=CARTESIAN_POINT('Ctrl Pts',(374.007710454608,109.183476597627,467.478855729964));
#61514=CARTESIAN_POINT('Ctrl Pts',(372.957769744647,108.748015119978,467.402443514309));
#61515=CARTESIAN_POINT('Ctrl Pts',(372.479273328296,108.420140704943,467.348231142275));
#61516=CARTESIAN_POINT('Ctrl Pts',(371.723752815371,107.664620192018,467.246090869444));
#61517=CARTESIAN_POINT('Ctrl Pts',(371.395891709399,107.186131013357,467.191447285196));
#61518=CARTESIAN_POINT('Ctrl Pts',(370.960439887906,106.136215362734,467.114043744988));
#61519=CARTESIAN_POINT('Ctrl Pts',(370.852917770961,105.564673948595,467.092461505801));
#61520=CARTESIAN_POINT('Ctrl Pts',(370.852917770961,104.491311513826,467.092461505801));
#61521=CARTESIAN_POINT('Ctrl Pts',(370.960439887907,103.919770099687,467.114043744988));
#61522=CARTESIAN_POINT('Ctrl Pts',(371.3958917094,102.869854449064,467.191447285196));
#61523=CARTESIAN_POINT('Ctrl Pts',(371.723752815371,102.391365270404,467.246090869444));
#61524=CARTESIAN_POINT('Ctrl Pts',(372.479273328297,101.635844757478,467.348231142275));
#61525=CARTESIAN_POINT('Ctrl Pts',(372.957769744648,101.307970342443,467.402443514309));
#61526=CARTESIAN_POINT('Ctrl Pts',(374.007710454609,100.872508864795,467.478855729964));
#61527=CARTESIAN_POINT('Ctrl Pts',(374.579260679033,100.764992731211,467.500000551892));
#61528=CARTESIAN_POINT('Ctrl Pts',(375.652574862888,100.764992731211,467.500000551892));
#61529=CARTESIAN_POINT('Ctrl Pts',(376.224125087313,100.872508864795,467.478855729964));
#61530=CARTESIAN_POINT('Ctrl Pts',(377.274065797274,101.307970342443,467.402443514309));
#61531=CARTESIAN_POINT('Ctrl Pts',(377.752562213625,101.635844757479,467.348231142275));
#61532=CARTESIAN_POINT('Ctrl Pts',(378.50808272655,102.391365270404,467.246090869444));
#61533=CARTESIAN_POINT('Ctrl Pts',(378.835943832522,102.869854449064,467.191447285196));
#61534=CARTESIAN_POINT('Ctrl Pts',(379.271395654015,103.919770099688,467.114043744988));
#61535=CARTESIAN_POINT('Ctrl Pts',(379.378917770961,104.491311513827,467.092461505801));
#61536=CARTESIAN_POINT('Ctrl Pts',(379.37891777096,105.027992731211,467.092461505801));
#61537=CARTESIAN_POINT('',(379.37891777096,105.027992731211,479.739413773764));
#61538=CARTESIAN_POINT('',(379.37891777096,105.027992731211,473.546231028847));
#61539=CARTESIAN_POINT('Ctrl Pts',(379.37891777096,105.027992731211,479.739413773765));
#61540=CARTESIAN_POINT('Ctrl Pts',(379.37891777096,104.492147376685,479.739413773765));
#61541=CARTESIAN_POINT('Ctrl Pts',(379.271719897152,103.92095247436,479.753090630838));
#61542=CARTESIAN_POINT('Ctrl Pts',(378.836500546949,102.870796956045,479.802374391123));
#61543=CARTESIAN_POINT('Ctrl Pts',(378.508507955969,102.391790499823,479.837256921998));
#61544=CARTESIAN_POINT('Ctrl Pts',(377.752122848377,101.635405392231,479.90264400738));
#61545=CARTESIAN_POINT('Ctrl Pts',(377.273115153636,101.307410572254,479.937413294598));
#61546=CARTESIAN_POINT('Ctrl Pts',(376.222955446812,100.872189584541,479.986437599389));
#61547=CARTESIAN_POINT('Ctrl Pts',(375.651759093084,100.764992731211,480.000000551892));
#61548=CARTESIAN_POINT('Ctrl Pts',(374.580076448838,100.764992731211,480.000000551892));
#61549=CARTESIAN_POINT('Ctrl Pts',(374.00888009511,100.872189584541,479.986437599389));
#61550=CARTESIAN_POINT('Ctrl Pts',(372.958720388286,101.307410572254,479.937413294598));
#61551=CARTESIAN_POINT('Ctrl Pts',(372.479712693545,101.63540539223,479.90264400738));
#61552=CARTESIAN_POINT('Ctrl Pts',(371.723327585953,102.391790499822,479.837256921998));
#61553=CARTESIAN_POINT('Ctrl Pts',(371.395334994972,102.870796956044,479.802374391123));
#61554=CARTESIAN_POINT('Ctrl Pts',(370.960115644769,103.92095247436,479.753090630838));
#61555=CARTESIAN_POINT('Ctrl Pts',(370.852917770961,104.492147376684,479.739413773765));
#61556=CARTESIAN_POINT('Ctrl Pts',(370.852917770961,105.563838085737,479.739413773765));
#61557=CARTESIAN_POINT('Ctrl Pts',(370.960115644769,106.135032988061,479.753090630838));
#61558=CARTESIAN_POINT('Ctrl Pts',(371.395334994972,107.185188506377,479.802374391123));
#61559=CARTESIAN_POINT('Ctrl Pts',(371.723327585952,107.664194962599,479.837256921998));
#61560=CARTESIAN_POINT('Ctrl Pts',(372.479712693544,108.420580070191,479.90264400738));
#61561=CARTESIAN_POINT('Ctrl Pts',(372.958720388285,108.748574890167,479.937413294598));
#61562=CARTESIAN_POINT('Ctrl Pts',(374.008880095109,109.183795877881,479.986437599388));
#61563=CARTESIAN_POINT('Ctrl Pts',(374.580076448837,109.290992731211,480.000000551892));
#61564=CARTESIAN_POINT('Ctrl Pts',(375.651759093083,109.290992731211,480.000000551892));
#61565=CARTESIAN_POINT('Ctrl Pts',(376.222955446811,109.183795877881,479.986437599388));
#61566=CARTESIAN_POINT('Ctrl Pts',(377.273115153635,108.748574890168,479.937413294598));
#61567=CARTESIAN_POINT('Ctrl Pts',(377.752122848376,108.420580070191,479.90264400738));
#61568=CARTESIAN_POINT('Ctrl Pts',(378.508507955968,107.664194962599,479.837256921998));
#61569=CARTESIAN_POINT('Ctrl Pts',(378.836500546949,107.185188506377,479.802374391123));
#61570=CARTESIAN_POINT('Ctrl Pts',(379.271719897152,106.135032988062,479.753090630838));
#61571=CARTESIAN_POINT('Ctrl Pts',(379.37891777096,105.563838085738,479.739413773765));
#61572=CARTESIAN_POINT('Ctrl Pts',(379.37891777096,105.027992731211,479.739413773765));
#61573=CARTESIAN_POINT('Origin',(375.115917770963,70.0279927312109,462.203977458126));
#61574=CARTESIAN_POINT('',(378.505667770963,70.027992731211,469.769126393098));
#61575=CARTESIAN_POINT('',(378.505667770963,70.0279927312109,462.203977458126));
#61576=CARTESIAN_POINT('',(371.726167770963,70.0279927312108,469.769126393098));
#61577=CARTESIAN_POINT('Ctrl Pts',(371.726167770963,70.0279927312109,469.769126393098));
#61578=CARTESIAN_POINT('Ctrl Pts',(371.726167770963,70.4541839515356,469.769126393098));
#61579=CARTESIAN_POINT('Ctrl Pts',(371.811449811382,70.9084195073466,469.781261919919));
#61580=CARTESIAN_POINT('Ctrl Pts',(372.157548323688,71.7434257096236,469.82495721765));
#61581=CARTESIAN_POINT('Ctrl Pts',(372.418336416162,72.1242417994641,469.855870958313));
#61582=CARTESIAN_POINT('Ctrl Pts',(373.019665216239,72.7255705995408,469.913791149419));
#61583=CARTESIAN_POINT('Ctrl Pts',(373.400482816929,72.9863614255432,469.944580424309));
#61584=CARTESIAN_POINT('Ctrl Pts',(374.235494154767,73.3324619346181,469.987990393875));
#61585=CARTESIAN_POINT('Ctrl Pts',(374.689731492675,73.4177427312108,470.000000551892));
#61586=CARTESIAN_POINT('Ctrl Pts',(375.542104049251,73.4177427312109,470.000000551892));
#61587=CARTESIAN_POINT('Ctrl Pts',(375.996341387159,73.3324619346182,469.987990393875));
#61588=CARTESIAN_POINT('Ctrl Pts',(376.831352724996,72.9863614255434,469.944580424309));
#61589=CARTESIAN_POINT('Ctrl Pts',(377.212170325687,72.7255705995412,469.913791149419));
#61590=CARTESIAN_POINT('Ctrl Pts',(377.813499125764,72.1242417994645,469.855870958313));
#61591=CARTESIAN_POINT('Ctrl Pts',(378.074287218238,71.7434257096241,469.82495721765));
#61592=CARTESIAN_POINT('Ctrl Pts',(378.420385730544,70.9084195073471,469.781261919919));
#61593=CARTESIAN_POINT('Ctrl Pts',(378.505667770963,70.4541839515359,469.769126393098));
#61594=CARTESIAN_POINT('Ctrl Pts',(378.505667770963,70.0279927312111,469.769126393098));
#61595=CARTESIAN_POINT('Ctrl Pts',(378.505667770963,70.0279927312111,469.769126393098));
#61596=CARTESIAN_POINT('Ctrl Pts',(378.505667770963,69.6018015108863,469.769126393098));
#61597=CARTESIAN_POINT('Ctrl Pts',(378.420385730544,69.1475659550751,469.781261919919));
#61598=CARTESIAN_POINT('Ctrl Pts',(378.074287218238,68.3125597527981,469.82495721765));
#61599=CARTESIAN_POINT('Ctrl Pts',(377.813499125764,67.9317436629576,469.855870958313));
#61600=CARTESIAN_POINT('Ctrl Pts',(377.212170325687,67.3304148628808,469.913791149419));
#61601=CARTESIAN_POINT('Ctrl Pts',(376.831352724997,67.0696240368785,469.944580424309));
#61602=CARTESIAN_POINT('Ctrl Pts',(375.99634138716,66.7235235278036,469.987990393875));
#61603=CARTESIAN_POINT('Ctrl Pts',(375.542104049251,66.6382427312109,470.000000551892));
#61604=CARTESIAN_POINT('Ctrl Pts',(374.689731492675,66.6382427312108,470.000000551892));
#61605=CARTESIAN_POINT('Ctrl Pts',(374.235494154767,66.7235235278035,469.987990393875));
#61606=CARTESIAN_POINT('Ctrl Pts',(373.40048281693,67.0696240368783,469.944580424309));
#61607=CARTESIAN_POINT('Ctrl Pts',(373.019665216239,67.3304148628805,469.913791149419));
#61608=CARTESIAN_POINT('Ctrl Pts',(372.418336416162,67.9317436629572,469.855870958313));
#61609=CARTESIAN_POINT('Ctrl Pts',(372.157548323688,68.3125597527976,469.82495721765));
#61610=CARTESIAN_POINT('Ctrl Pts',(371.811449811382,69.1475659550746,469.781261919919));
#61611=CARTESIAN_POINT('Ctrl Pts',(371.726167770963,69.6018015108858,469.769126393098));
#61612=CARTESIAN_POINT('Ctrl Pts',(371.726167770963,70.0279927312106,469.769126393098));
#61613=CARTESIAN_POINT('Origin',(375.115917770964,55.0279927312109,462.203977458126));
#61614=CARTESIAN_POINT('',(378.505667770964,55.027992731211,469.769126393098));
#61615=CARTESIAN_POINT('',(378.505667770964,55.0279927312109,462.203977458126));
#61616=CARTESIAN_POINT('',(371.726167770964,55.0279927312099,469.769126393099));
#61617=CARTESIAN_POINT('Ctrl Pts',(371.726167770964,55.0279927312099,469.769126393098));
#61618=CARTESIAN_POINT('Ctrl Pts',(371.726167770964,55.4541839515347,469.769126393098));
#61619=CARTESIAN_POINT('Ctrl Pts',(371.811449811384,55.9084195073467,469.781261919919));
#61620=CARTESIAN_POINT('Ctrl Pts',(372.157548323689,56.7434257096237,469.82495721765));
#61621=CARTESIAN_POINT('Ctrl Pts',(372.418336416163,57.1242417994641,469.855870958314));
#61622=CARTESIAN_POINT('Ctrl Pts',(373.01966521624,57.7255705995409,469.913791149419));
#61623=CARTESIAN_POINT('Ctrl Pts',(373.40048281693,57.9863614255432,469.944580424309));
#61624=CARTESIAN_POINT('Ctrl Pts',(374.235494154768,58.3324619346181,469.987990393875));
#61625=CARTESIAN_POINT('Ctrl Pts',(374.689731492676,58.4177427312108,470.000000551892));
#61626=CARTESIAN_POINT('Ctrl Pts',(375.542104049252,58.4177427312109,470.000000551892));
#61627=CARTESIAN_POINT('Ctrl Pts',(375.99634138716,58.3324619346183,469.987990393875));
#61628=CARTESIAN_POINT('Ctrl Pts',(376.831352724997,57.9863614255434,469.944580424309));
#61629=CARTESIAN_POINT('Ctrl Pts',(377.212170325688,57.7255705995412,469.913791149419));
#61630=CARTESIAN_POINT('Ctrl Pts',(377.813499125765,57.1242417994645,469.855870958314));
#61631=CARTESIAN_POINT('Ctrl Pts',(378.074287218239,56.7434257096241,469.82495721765));
#61632=CARTESIAN_POINT('Ctrl Pts',(378.420385730545,55.9084195073471,469.781261919919));
#61633=CARTESIAN_POINT('Ctrl Pts',(378.505667770964,55.4541839515359,469.769126393098));
#61634=CARTESIAN_POINT('Ctrl Pts',(378.505667770964,55.0279927312111,469.769126393098));
#61635=CARTESIAN_POINT('Ctrl Pts',(378.505667770964,55.0279927312111,469.769126393098));
#61636=CARTESIAN_POINT('Ctrl Pts',(378.505667770964,54.6018015108864,469.769126393098));
#61637=CARTESIAN_POINT('Ctrl Pts',(378.420385730545,54.1475659550751,469.781261919919));
#61638=CARTESIAN_POINT('Ctrl Pts',(378.074287218239,53.3125597527981,469.82495721765));
#61639=CARTESIAN_POINT('Ctrl Pts',(377.813499125765,52.9317436629576,469.855870958314));
#61640=CARTESIAN_POINT('Ctrl Pts',(377.212170325688,52.3304148628809,469.913791149419));
#61641=CARTESIAN_POINT('Ctrl Pts',(376.831352724998,52.0696240368786,469.944580424309));
#61642=CARTESIAN_POINT('Ctrl Pts',(375.996341387161,51.7235235278036,469.987990393875));
#61643=CARTESIAN_POINT('Ctrl Pts',(375.542104049252,51.6382427312109,470.000000551892));
#61644=CARTESIAN_POINT('Ctrl Pts',(374.689731492677,51.6382427312109,470.000000551892));
#61645=CARTESIAN_POINT('Ctrl Pts',(374.235494154768,51.7235235278036,469.987990393875));
#61646=CARTESIAN_POINT('Ctrl Pts',(373.400482816931,52.0696240368784,469.944580424309));
#61647=CARTESIAN_POINT('Ctrl Pts',(373.01966521624,52.3304148628806,469.913791149419));
#61648=CARTESIAN_POINT('Ctrl Pts',(372.418336416164,52.9317436629573,469.855870958314));
#61649=CARTESIAN_POINT('Ctrl Pts',(372.157548323689,53.3125597527977,469.82495721765));
#61650=CARTESIAN_POINT('Ctrl Pts',(371.811449811384,54.1475659550746,469.781261919919));
#61651=CARTESIAN_POINT('Ctrl Pts',(371.726167770964,54.6018015108859,469.769126393098));
#61652=CARTESIAN_POINT('Ctrl Pts',(371.726167770964,55.0279927312106,469.769126393098));
#61653=CARTESIAN_POINT('Origin',(375.115917770961,95.0279927312111,422.490000551892));
#61654=CARTESIAN_POINT('',(397.615917770961,95.0279927312126,445.000000551892));
#61655=CARTESIAN_POINT('Origin',(375.115917770961,95.027992731211,445.000000551892));
#61656=CARTESIAN_POINT('Origin',(375.11591777096,120.027992731211,445.000000551892));
#61657=CARTESIAN_POINT('',(397.615917770958,145.027992731213,445.000000551892));
#61658=CARTESIAN_POINT('',(397.61591777096,120.027992731213,445.000000551892));
#61659=CARTESIAN_POINT('Origin',(375.115917770958,145.027992731211,445.000000551892));
#61660=CARTESIAN_POINT('Origin',(375.115917770963,67.527992731211,445.000000551892));
#61661=CARTESIAN_POINT('',(395.461568672241,50.0279927312126,459.527715079768));
#61662=CARTESIAN_POINT('',(400.115917770964,50.0279927312127,445.000000551893));
#61663=CARTESIAN_POINT('Origin',(375.115917770965,50.027992731211,445.000000551893));
#61664=CARTESIAN_POINT('Origin',(375.115917770965,50.027992731211,445.000000551893));
#61665=CARTESIAN_POINT('',(400.115917770962,85.027992731213,445.000000551892));
#61666=CARTESIAN_POINT('',(400.115917770963,67.5279927312129,445.000000551892));
#61667=CARTESIAN_POINT('',(354.770266869685,85.0279927312089,430.47228602402));
#61668=CARTESIAN_POINT('Origin',(375.115917770962,85.027992731211,445.000000551892));
#61669=CARTESIAN_POINT('Origin',(375.115917770962,85.027992731211,445.000000551892));
#61670=CARTESIAN_POINT('Origin',(375.115917770964,45.52799273121,445.000000551893));
#61671=CARTESIAN_POINT('',(391.392438491985,45.0279927312106,456.622172174192));
#61672=CARTESIAN_POINT('',(391.799351510011,45.527992731211,456.91272646475));
#61673=CARTESIAN_POINT('Origin',(375.115917770965,45.027992731211,445.000000551893));
#61674=CARTESIAN_POINT('Origin',(375.115917770965,45.0279927312111,424.990000551893));
#61675=CARTESIAN_POINT('Origin',(375.115917770958,144.527992731211,445.000000551892));
#61676=CARTESIAN_POINT('',(403.599829032745,140.027992731212,424.661200212869));
#61677=CARTESIAN_POINT('',(410.115917770958,140.027992731214,445.000000551892));
#61678=CARTESIAN_POINT('Origin',(375.115917770958,140.027992731211,445.000000551892));
#61679=CARTESIAN_POINT('Origin',(375.115917770958,140.027992731211,445.000000551892));
#61680=CARTESIAN_POINT('',(399.530698852489,145.027992731213,427.566743118444));
#61681=CARTESIAN_POINT('',(399.937611870515,144.527992731213,427.276188827887));
#61682=CARTESIAN_POINT('Origin',(375.115917770958,145.027992731211,445.000000551892));
#61683=CARTESIAN_POINT('Origin',(375.11591777096,117.52799273121,445.000000551892));
#61684=CARTESIAN_POINT('',(410.115917770961,95.027992731213,445.000000551892));
#61685=CARTESIAN_POINT('',(410.11591777096,117.527992731212,445.000000551892));
#61686=CARTESIAN_POINT('',(346.632006509173,95.0279927312094,424.66120021287));
#61687=CARTESIAN_POINT('Origin',(375.115917770961,95.027992731211,445.000000551892));
#61688=CARTESIAN_POINT('Origin',(375.115917770961,95.027992731211,445.000000551892));
#61689=CARTESIAN_POINT('Origin',(375.115917770958,145.027992731211,414.990000551892));
#61690=CARTESIAN_POINT('Origin',(375.115917770962,86.027992731211,445.000000551892));
#61691=CARTESIAN_POINT('',(353.956440833633,86.0279927312097,429.891177442905));
#61692=CARTESIAN_POINT('',(0.,0.,0.));
#61693=CARTESIAN_POINT('',(0.,0.,0.));
#61694=CARTESIAN_POINT('',(0.,0.,0.));
#61695=CARTESIAN_POINT('',(-172.24399665854,29.9999999999993,247.176654275314));
#61696=CARTESIAN_POINT('',(-197.823346276547,59.9999999999983,547.359914429512));
#61697=CARTESIAN_POINT('',(-69.8840827809313,89.9999999999977,820.115918322853));
#61698=CARTESIAN_POINT('',(272.756003893344,-29.9999999999996,-127.939263495619));
#61699=CARTESIAN_POINT('',(677.523827315906,-360.944014537578,853.66005091519));
#61700=CARTESIAN_POINT('',(417.673669784473,-390.944014537578,1006.1139404508));
#61701=CARTESIAN_POINT('',(116.409887416998,-420.944014537578,1008.21780292866));
#61702=CARTESIAN_POINT('',(-145.544132592325,-450.944014537578,859.407910096835));
#61703=CARTESIAN_POINT('',(826.333720147737,-330.944014537579,591.706030905864));
#61704=CARTESIAN_POINT('',(0.,0.,0.));
#61705=CARTESIAN_POINT('',(112.,-5.32907051820075E-14,-6.3948846218409E-13));
#61706=CARTESIAN_POINT('',(708.115918322864,-360.94401453758,708.115918322856));
#61707=CARTESIAN_POINT('',(820.115918322864,-360.94401453758,708.115918322855));
#61708=CARTESIAN_POINT('',(0.,0.,0.));
#61709=CARTESIAN_POINT('',(4.2632564145606E-13,-7.105427357601E-14,83.));
#61710=CARTESIAN_POINT('',(82.9999999999998,-1.77635683940025E-14,-4.9737991503207E-13));
#61711=CARTESIAN_POINT('',(112.,-1.24344978758018E-13,82.9999999999994));
#61712=CARTESIAN_POINT('',(194.999999999999,-7.99360577730113E-14,-1.06581410364015E-12));
#61713=CARTESIAN_POINT('',(112.,-3.5527136788005E-14,-4.9737991503207E-13));
#61714=CARTESIAN_POINT('',(195.,-1.68753899743024E-13,82.9999999999989));
#61715=CARTESIAN_POINT('',(83.0000000000003,-1.06581410364015E-13,82.9999999999994));
#61716=CARTESIAN_POINT('',(195.000000000004,-360.94401453758,807.000001103788));
#61717=CARTESIAN_POINT('',(4.65405491922866E-12,-360.944014537579,890.000001103789));
#61718=CARTESIAN_POINT('',(83.000000000004,-360.944014537579,807.000001103788));
#61719=CARTESIAN_POINT('',(112.000000000005,-360.944014537579,890.000001103788));
#61720=CARTESIAN_POINT('',(112.000000000004,-360.944014537579,807.000001103788));
#61721=CARTESIAN_POINT('',(195.000000000004,-360.944014537579,890.000001103788));
#61722=CARTESIAN_POINT('',(83.0000000000044,-360.944014537579,890.000001103788));
#61723=CARTESIAN_POINT('',(4.19220214098459E-12,-360.944014537579,807.000001103789));
#61724=CARTESIAN_POINT('',(0.,0.,0.));
#61725=CARTESIAN_POINT('',(7.105427357601E-13,-4.44089209850063E-13,130.));
#61726=CARTESIAN_POINT('',(3.5527136788005E-13,-1.77635683940025E-13,65.));
#61727=CARTESIAN_POINT('',(-6.3948846218409E-13,-175.,1.4210854715202E-13));
#61728=CARTESIAN_POINT('',(7.105427357601E-14,-175.,130.));
#61729=CARTESIAN_POINT('',(-2.8421709430404E-13,-175.,65.0000000000001));
#61730=CARTESIAN_POINT('',(638.231835541933,-185.944014537579,-2.55795384873636E-12));
#61731=CARTESIAN_POINT('',(638.231835541933,-185.944014537579,129.999999999997));
#61732=CARTESIAN_POINT('',(638.231835541933,-185.944014537579,64.9999999999974));
#61733=CARTESIAN_POINT('',(638.231835541932,-360.944014537579,-3.33955085807247E-12));
#61734=CARTESIAN_POINT('',(638.231835541933,-360.944014537579,129.999999999997));
#61735=CARTESIAN_POINT('',(638.231835541932,-360.944014537579,64.9999999999967));
#61736=CARTESIAN_POINT('',(0.,0.,0.));
#61737=CARTESIAN_POINT('',(0.,0.,0.));
#61738=CARTESIAN_POINT('',(-250.000000000001,220.,2.55795384873636E-12));
#61739=CARTESIAN_POINT('',(-250.000000000001,9.9475983006414E-13,1.49213974509621E-12));
#61740=CARTESIAN_POINT('',(0.,220.,1.4210854715202E-13));
#61741=CARTESIAN_POINT('',(0.,0.,0.));
#61742=CARTESIAN_POINT('',(0.,0.,0.));
#61743=CARTESIAN_POINT('',(0.,0.,0.));
#61744=CARTESIAN_POINT('',(0.,0.,0.));
#61745=CARTESIAN_POINT('',(0.,0.,0.));
#61746=CARTESIAN_POINT('',(0.,0.,0.));
#61747=CARTESIAN_POINT('',(0.,0.,0.));
#61748=CARTESIAN_POINT('',(0.,0.,0.));
#61749=CARTESIAN_POINT('',(0.,0.,0.));
#61750=UNCERTAINTY_MEASURE_WITH_UNIT(LENGTH_MEASURE(0.01),#61812,
'DISTANCE_ACCURACY_VALUE',
'Maximum model space distance between geometric entities at asserted c
onnectivities');
#61751=UNCERTAINTY_MEASURE_WITH_UNIT(LENGTH_MEASURE(0.01),#61812,
'DISTANCE_ACCURACY_VALUE',
'Maximum model space distance between geometric entities at asserted c
onnectivities');
#61752=UNCERTAINTY_MEASURE_WITH_UNIT(LENGTH_MEASURE(0.01),#61812,
'DISTANCE_ACCURACY_VALUE',
'Maximum model space distance between geometric entities at asserted c
onnectivities');
#61753=UNCERTAINTY_MEASURE_WITH_UNIT(LENGTH_MEASURE(0.01),#61812,
'DISTANCE_ACCURACY_VALUE',
'Maximum model space distance between geometric entities at asserted c
onnectivities');
#61754=UNCERTAINTY_MEASURE_WITH_UNIT(LENGTH_MEASURE(0.01),#61812,
'DISTANCE_ACCURACY_VALUE',
'Maximum model space distance between geometric entities at asserted c
onnectivities');
#61755=UNCERTAINTY_MEASURE_WITH_UNIT(LENGTH_MEASURE(0.01),#61812,
'DISTANCE_ACCURACY_VALUE',
'Maximum model space distance between geometric entities at asserted c
onnectivities');
#61756=UNCERTAINTY_MEASURE_WITH_UNIT(LENGTH_MEASURE(0.01),#61812,
'DISTANCE_ACCURACY_VALUE',
'Maximum model space distance between geometric entities at asserted c
onnectivities');
#61757=UNCERTAINTY_MEASURE_WITH_UNIT(LENGTH_MEASURE(0.01),#61812,
'DISTANCE_ACCURACY_VALUE',
'Maximum model space distance between geometric entities at asserted c
onnectivities');
#61758=UNCERTAINTY_MEASURE_WITH_UNIT(LENGTH_MEASURE(0.01),#61812,
'DISTANCE_ACCURACY_VALUE',
'Maximum model space distance between geometric entities at asserted c
onnectivities');
#61759=UNCERTAINTY_MEASURE_WITH_UNIT(LENGTH_MEASURE(0.01),#61812,
'DISTANCE_ACCURACY_VALUE',
'Maximum model space distance between geometric entities at asserted c
onnectivities');
#61760=UNCERTAINTY_MEASURE_WITH_UNIT(LENGTH_MEASURE(0.01),#61812,
'DISTANCE_ACCURACY_VALUE',
'Maximum model space distance between geometric entities at asserted c
onnectivities');
#61761=UNCERTAINTY_MEASURE_WITH_UNIT(LENGTH_MEASURE(0.01),#61812,
'DISTANCE_ACCURACY_VALUE',
'Maximum model space distance between geometric entities at asserted c
onnectivities');
#61762=UNCERTAINTY_MEASURE_WITH_UNIT(LENGTH_MEASURE(0.01),#61812,
'DISTANCE_ACCURACY_VALUE',
'Maximum model space distance between geometric entities at asserted c
onnectivities');
#61763=UNCERTAINTY_MEASURE_WITH_UNIT(LENGTH_MEASURE(0.01),#61812,
'DISTANCE_ACCURACY_VALUE',
'Maximum model space distance between geometric entities at asserted c
onnectivities');
#61764=UNCERTAINTY_MEASURE_WITH_UNIT(LENGTH_MEASURE(0.01),#61812,
'DISTANCE_ACCURACY_VALUE',
'Maximum model space distance between geometric entities at asserted c
onnectivities');
#61765=UNCERTAINTY_MEASURE_WITH_UNIT(LENGTH_MEASURE(0.01),#61812,
'DISTANCE_ACCURACY_VALUE',
'Maximum model space distance between geometric entities at asserted c
onnectivities');
#61766=UNCERTAINTY_MEASURE_WITH_UNIT(LENGTH_MEASURE(0.01),#61812,
'DISTANCE_ACCURACY_VALUE',
'Maximum model space distance between geometric entities at asserted c
onnectivities');
#61767=UNCERTAINTY_MEASURE_WITH_UNIT(LENGTH_MEASURE(0.01),#61812,
'DISTANCE_ACCURACY_VALUE',
'Maximum model space distance between geometric entities at asserted c
onnectivities');
#61768=UNCERTAINTY_MEASURE_WITH_UNIT(LENGTH_MEASURE(0.01),#61812,
'DISTANCE_ACCURACY_VALUE',
'Maximum model space distance between geometric entities at asserted c
onnectivities');
#61769=UNCERTAINTY_MEASURE_WITH_UNIT(LENGTH_MEASURE(0.01),#61812,
'DISTANCE_ACCURACY_VALUE',
'Maximum model space distance between geometric entities at asserted c
onnectivities');
#61770=UNCERTAINTY_MEASURE_WITH_UNIT(LENGTH_MEASURE(0.01),#61812,
'DISTANCE_ACCURACY_VALUE',
'Maximum model space distance between geometric entities at asserted c
onnectivities');
#61771=UNCERTAINTY_MEASURE_WITH_UNIT(LENGTH_MEASURE(0.01),#61812,
'DISTANCE_ACCURACY_VALUE',
'Maximum model space distance between geometric entities at asserted c
onnectivities');
#61772=UNCERTAINTY_MEASURE_WITH_UNIT(LENGTH_MEASURE(0.01),#61812,
'DISTANCE_ACCURACY_VALUE',
'Maximum model space distance between geometric entities at asserted c
onnectivities');
#61773=UNCERTAINTY_MEASURE_WITH_UNIT(LENGTH_MEASURE(0.01),#61812,
'DISTANCE_ACCURACY_VALUE',
'Maximum model space distance between geometric entities at asserted c
onnectivities');
#61774=UNCERTAINTY_MEASURE_WITH_UNIT(LENGTH_MEASURE(0.01),#61812,
'DISTANCE_ACCURACY_VALUE',
'Maximum model space distance between geometric entities at asserted c
onnectivities');
#61775=UNCERTAINTY_MEASURE_WITH_UNIT(LENGTH_MEASURE(0.01),#61812,
'DISTANCE_ACCURACY_VALUE',
'Maximum model space distance between geometric entities at asserted c
onnectivities');
#61776=UNCERTAINTY_MEASURE_WITH_UNIT(LENGTH_MEASURE(0.01),#61812,
'DISTANCE_ACCURACY_VALUE',
'Maximum model space distance between geometric entities at asserted c
onnectivities');
#61777=UNCERTAINTY_MEASURE_WITH_UNIT(LENGTH_MEASURE(0.01),#61812,
'DISTANCE_ACCURACY_VALUE',
'Maximum model space distance between geometric entities at asserted c
onnectivities');
#61778=UNCERTAINTY_MEASURE_WITH_UNIT(LENGTH_MEASURE(0.01),#61812,
'DISTANCE_ACCURACY_VALUE',
'Maximum model space distance between geometric entities at asserted c
onnectivities');
#61779=UNCERTAINTY_MEASURE_WITH_UNIT(LENGTH_MEASURE(0.01),#61812,
'DISTANCE_ACCURACY_VALUE',
'Maximum model space distance between geometric entities at asserted c
onnectivities');
#61780=UNCERTAINTY_MEASURE_WITH_UNIT(LENGTH_MEASURE(0.01),#61812,
'DISTANCE_ACCURACY_VALUE',
'Maximum model space distance between geometric entities at asserted c
onnectivities');
#61781=(
GEOMETRIC_REPRESENTATION_CONTEXT(3)
GLOBAL_UNCERTAINTY_ASSIGNED_CONTEXT((#61750))
GLOBAL_UNIT_ASSIGNED_CONTEXT((#61812,#61814,#61815))
REPRESENTATION_CONTEXT('','3D')
);
#61782=(
GEOMETRIC_REPRESENTATION_CONTEXT(3)
GLOBAL_UNCERTAINTY_ASSIGNED_CONTEXT((#61751))
GLOBAL_UNIT_ASSIGNED_CONTEXT((#61812,#61814,#61815))
REPRESENTATION_CONTEXT('','3D')
);
#61783=(
GEOMETRIC_REPRESENTATION_CONTEXT(3)
GLOBAL_UNCERTAINTY_ASSIGNED_CONTEXT((#61752))
GLOBAL_UNIT_ASSIGNED_CONTEXT((#61812,#61814,#61815))
REPRESENTATION_CONTEXT('','3D')
);
#61784=(
GEOMETRIC_REPRESENTATION_CONTEXT(3)
GLOBAL_UNCERTAINTY_ASSIGNED_CONTEXT((#61753))
GLOBAL_UNIT_ASSIGNED_CONTEXT((#61812,#61814,#61815))
REPRESENTATION_CONTEXT('','3D')
);
#61785=(
GEOMETRIC_REPRESENTATION_CONTEXT(3)
GLOBAL_UNCERTAINTY_ASSIGNED_CONTEXT((#61754))
GLOBAL_UNIT_ASSIGNED_CONTEXT((#61812,#61814,#61815))
REPRESENTATION_CONTEXT('','3D')
);
#61786=(
GEOMETRIC_REPRESENTATION_CONTEXT(3)
GLOBAL_UNCERTAINTY_ASSIGNED_CONTEXT((#61755))
GLOBAL_UNIT_ASSIGNED_CONTEXT((#61812,#61814,#61815))
REPRESENTATION_CONTEXT('','3D')
);
#61787=(
GEOMETRIC_REPRESENTATION_CONTEXT(3)
GLOBAL_UNCERTAINTY_ASSIGNED_CONTEXT((#61756))
GLOBAL_UNIT_ASSIGNED_CONTEXT((#61812,#61814,#61815))
REPRESENTATION_CONTEXT('','3D')
);
#61788=(
GEOMETRIC_REPRESENTATION_CONTEXT(3)
GLOBAL_UNCERTAINTY_ASSIGNED_CONTEXT((#61757))
GLOBAL_UNIT_ASSIGNED_CONTEXT((#61812,#61814,#61815))
REPRESENTATION_CONTEXT('','3D')
);
#61789=(
GEOMETRIC_REPRESENTATION_CONTEXT(3)
GLOBAL_UNCERTAINTY_ASSIGNED_CONTEXT((#61758))
GLOBAL_UNIT_ASSIGNED_CONTEXT((#61812,#61814,#61815))
REPRESENTATION_CONTEXT('','3D')
);
#61790=(
GEOMETRIC_REPRESENTATION_CONTEXT(3)
GLOBAL_UNCERTAINTY_ASSIGNED_CONTEXT((#61759))
GLOBAL_UNIT_ASSIGNED_CONTEXT((#61812,#61814,#61815))
REPRESENTATION_CONTEXT('','3D')
);
#61791=(
GEOMETRIC_REPRESENTATION_CONTEXT(3)
GLOBAL_UNCERTAINTY_ASSIGNED_CONTEXT((#61760))
GLOBAL_UNIT_ASSIGNED_CONTEXT((#61812,#61814,#61815))
REPRESENTATION_CONTEXT('','3D')
);
#61792=(
GEOMETRIC_REPRESENTATION_CONTEXT(3)
GLOBAL_UNCERTAINTY_ASSIGNED_CONTEXT((#61761))
GLOBAL_UNIT_ASSIGNED_CONTEXT((#61812,#61814,#61815))
REPRESENTATION_CONTEXT('','3D')
);
#61793=(
GEOMETRIC_REPRESENTATION_CONTEXT(3)
GLOBAL_UNCERTAINTY_ASSIGNED_CONTEXT((#61762))
GLOBAL_UNIT_ASSIGNED_CONTEXT((#61812,#61814,#61815))
REPRESENTATION_CONTEXT('','3D')
);
#61794=(
GEOMETRIC_REPRESENTATION_CONTEXT(3)
GLOBAL_UNCERTAINTY_ASSIGNED_CONTEXT((#61763))
GLOBAL_UNIT_ASSIGNED_CONTEXT((#61812,#61814,#61815))
REPRESENTATION_CONTEXT('','3D')
);
#61795=(
GEOMETRIC_REPRESENTATION_CONTEXT(3)
GLOBAL_UNCERTAINTY_ASSIGNED_CONTEXT((#61764))
GLOBAL_UNIT_ASSIGNED_CONTEXT((#61812,#61814,#61815))
REPRESENTATION_CONTEXT('','3D')
);
#61796=(
GEOMETRIC_REPRESENTATION_CONTEXT(3)
GLOBAL_UNCERTAINTY_ASSIGNED_CONTEXT((#61765))
GLOBAL_UNIT_ASSIGNED_CONTEXT((#61812,#61814,#61815))
REPRESENTATION_CONTEXT('','3D')
);
#61797=(
GEOMETRIC_REPRESENTATION_CONTEXT(3)
GLOBAL_UNCERTAINTY_ASSIGNED_CONTEXT((#61766))
GLOBAL_UNIT_ASSIGNED_CONTEXT((#61812,#61814,#61815))
REPRESENTATION_CONTEXT('','3D')
);
#61798=(
GEOMETRIC_REPRESENTATION_CONTEXT(3)
GLOBAL_UNCERTAINTY_ASSIGNED_CONTEXT((#61767))
GLOBAL_UNIT_ASSIGNED_CONTEXT((#61812,#61814,#61815))
REPRESENTATION_CONTEXT('','3D')
);
#61799=(
GEOMETRIC_REPRESENTATION_CONTEXT(3)
GLOBAL_UNCERTAINTY_ASSIGNED_CONTEXT((#61768))
GLOBAL_UNIT_ASSIGNED_CONTEXT((#61812,#61814,#61815))
REPRESENTATION_CONTEXT('','3D')
);
#61800=(
GEOMETRIC_REPRESENTATION_CONTEXT(3)
GLOBAL_UNCERTAINTY_ASSIGNED_CONTEXT((#61769))
GLOBAL_UNIT_ASSIGNED_CONTEXT((#61812,#61814,#61815))
REPRESENTATION_CONTEXT('','3D')
);
#61801=(
GEOMETRIC_REPRESENTATION_CONTEXT(3)
GLOBAL_UNCERTAINTY_ASSIGNED_CONTEXT((#61770))
GLOBAL_UNIT_ASSIGNED_CONTEXT((#61812,#61814,#61815))
REPRESENTATION_CONTEXT('','3D')
);
#61802=(
GEOMETRIC_REPRESENTATION_CONTEXT(3)
GLOBAL_UNCERTAINTY_ASSIGNED_CONTEXT((#61771))
GLOBAL_UNIT_ASSIGNED_CONTEXT((#61812,#61814,#61815))
REPRESENTATION_CONTEXT('','3D')
);
#61803=(
GEOMETRIC_REPRESENTATION_CONTEXT(3)
GLOBAL_UNCERTAINTY_ASSIGNED_CONTEXT((#61772))
GLOBAL_UNIT_ASSIGNED_CONTEXT((#61812,#61814,#61815))
REPRESENTATION_CONTEXT('','3D')
);
#61804=(
GEOMETRIC_REPRESENTATION_CONTEXT(3)
GLOBAL_UNCERTAINTY_ASSIGNED_CONTEXT((#61773))
GLOBAL_UNIT_ASSIGNED_CONTEXT((#61812,#61814,#61815))
REPRESENTATION_CONTEXT('','3D')
);
#61805=(
GEOMETRIC_REPRESENTATION_CONTEXT(3)
GLOBAL_UNCERTAINTY_ASSIGNED_CONTEXT((#61774))
GLOBAL_UNIT_ASSIGNED_CONTEXT((#61812,#61814,#61815))
REPRESENTATION_CONTEXT('','3D')
);
#61806=(
GEOMETRIC_REPRESENTATION_CONTEXT(3)
GLOBAL_UNCERTAINTY_ASSIGNED_CONTEXT((#61775))
GLOBAL_UNIT_ASSIGNED_CONTEXT((#61812,#61814,#61815))
REPRESENTATION_CONTEXT('','3D')
);
#61807=(
GEOMETRIC_REPRESENTATION_CONTEXT(3)
GLOBAL_UNCERTAINTY_ASSIGNED_CONTEXT((#61776))
GLOBAL_UNIT_ASSIGNED_CONTEXT((#61812,#61814,#61815))
REPRESENTATION_CONTEXT('','3D')
);
#61808=(
GEOMETRIC_REPRESENTATION_CONTEXT(3)
GLOBAL_UNCERTAINTY_ASSIGNED_CONTEXT((#61777))
GLOBAL_UNIT_ASSIGNED_CONTEXT((#61812,#61814,#61815))
REPRESENTATION_CONTEXT('','3D')
);
#61809=(
GEOMETRIC_REPRESENTATION_CONTEXT(3)
GLOBAL_UNCERTAINTY_ASSIGNED_CONTEXT((#61778))
GLOBAL_UNIT_ASSIGNED_CONTEXT((#61812,#61814,#61815))
REPRESENTATION_CONTEXT('','3D')
);
#61810=(
GEOMETRIC_REPRESENTATION_CONTEXT(3)
GLOBAL_UNCERTAINTY_ASSIGNED_CONTEXT((#61779))
GLOBAL_UNIT_ASSIGNED_CONTEXT((#61812,#61814,#61815))
REPRESENTATION_CONTEXT('','3D')
);
#61811=(
GEOMETRIC_REPRESENTATION_CONTEXT(3)
GLOBAL_UNCERTAINTY_ASSIGNED_CONTEXT((#61780))
GLOBAL_UNIT_ASSIGNED_CONTEXT((#61812,#61814,#61815))
REPRESENTATION_CONTEXT('','3D')
);
#61812=(
LENGTH_UNIT()
NAMED_UNIT(*)
SI_UNIT(.MILLI.,.METRE.)
);
#61813=(
LENGTH_UNIT()
NAMED_UNIT(*)
SI_UNIT($,.METRE.)
);
#61814=(
NAMED_UNIT(*)
PLANE_ANGLE_UNIT()
SI_UNIT($,.RADIAN.)
);
#61815=(
NAMED_UNIT(*)
SI_UNIT($,.STERADIAN.)
SOLID_ANGLE_UNIT()
);
#61816=SHAPE_DEFINITION_REPRESENTATION(#61846,#61968);
#61817=SHAPE_DEFINITION_REPRESENTATION(#61847,#61969);
#61818=SHAPE_DEFINITION_REPRESENTATION(#61848,#61970);
#61819=SHAPE_DEFINITION_REPRESENTATION(#61849,#61971);
#61820=SHAPE_DEFINITION_REPRESENTATION(#61850,#61972);
#61821=SHAPE_DEFINITION_REPRESENTATION(#61851,#61973);
#61822=SHAPE_DEFINITION_REPRESENTATION(#61852,#61974);
#61823=SHAPE_DEFINITION_REPRESENTATION(#61853,#61975);
#61824=SHAPE_DEFINITION_REPRESENTATION(#61854,#61976);
#61825=SHAPE_DEFINITION_REPRESENTATION(#61855,#61977);
#61826=SHAPE_DEFINITION_REPRESENTATION(#61856,#61978);
#61827=SHAPE_DEFINITION_REPRESENTATION(#61857,#61979);
#61828=SHAPE_DEFINITION_REPRESENTATION(#61858,#61980);
#61829=SHAPE_DEFINITION_REPRESENTATION(#61859,#61981);
#61830=SHAPE_DEFINITION_REPRESENTATION(#61860,#61982);
#61831=SHAPE_DEFINITION_REPRESENTATION(#61861,#61983);
#61832=SHAPE_DEFINITION_REPRESENTATION(#61862,#61984);
#61833=SHAPE_DEFINITION_REPRESENTATION(#61863,#61985);
#61834=SHAPE_DEFINITION_REPRESENTATION(#61864,#61986);
#61835=SHAPE_DEFINITION_REPRESENTATION(#61881,#61987);
#61836=SHAPE_DEFINITION_REPRESENTATION(#61882,#61988);
#61837=SHAPE_DEFINITION_REPRESENTATION(#61883,#61989);
#61838=SHAPE_DEFINITION_REPRESENTATION(#61884,#61990);
#61839=SHAPE_DEFINITION_REPRESENTATION(#61885,#61991);
#61840=SHAPE_DEFINITION_REPRESENTATION(#61902,#61992);
#61841=SHAPE_DEFINITION_REPRESENTATION(#61903,#61993);
#61842=SHAPE_DEFINITION_REPRESENTATION(#61904,#61994);
#61843=SHAPE_DEFINITION_REPRESENTATION(#61907,#61995);
#61844=SHAPE_DEFINITION_REPRESENTATION(#61908,#61996);
#61845=SHAPE_DEFINITION_REPRESENTATION(#61909,#61997);
#61846=PRODUCT_DEFINITION_SHAPE('',$,#61999);
#61847=PRODUCT_DEFINITION_SHAPE('',$,#62000);
#61848=PRODUCT_DEFINITION_SHAPE('',$,#62001);
#61849=PRODUCT_DEFINITION_SHAPE('',$,#62002);
#61850=PRODUCT_DEFINITION_SHAPE('',$,#62003);
#61851=PRODUCT_DEFINITION_SHAPE('',$,#62004);
#61852=PRODUCT_DEFINITION_SHAPE('',$,#62005);
#61853=PRODUCT_DEFINITION_SHAPE('',$,#62006);
#61854=PRODUCT_DEFINITION_SHAPE('',$,#62007);
#61855=PRODUCT_DEFINITION_SHAPE('',$,#62008);
#61856=PRODUCT_DEFINITION_SHAPE('',$,#62009);
#61857=PRODUCT_DEFINITION_SHAPE('',$,#62010);
#61858=PRODUCT_DEFINITION_SHAPE('',$,#62011);
#61859=PRODUCT_DEFINITION_SHAPE('',$,#62012);
#61860=PRODUCT_DEFINITION_SHAPE('',$,#62013);
#61861=PRODUCT_DEFINITION_SHAPE('',$,#62014);
#61862=PRODUCT_DEFINITION_SHAPE('',$,#62015);
#61863=PRODUCT_DEFINITION_SHAPE('',$,#62016);
#61864=PRODUCT_DEFINITION_SHAPE('',$,#62017);
#61865=PRODUCT_DEFINITION_SHAPE($,$,#298);
#61866=PRODUCT_DEFINITION_SHAPE($,$,#299);
#61867=PRODUCT_DEFINITION_SHAPE($,$,#300);
#61868=PRODUCT_DEFINITION_SHAPE($,$,#301);
#61869=PRODUCT_DEFINITION_SHAPE($,$,#302);
#61870=PRODUCT_DEFINITION_SHAPE($,$,#303);
#61871=PRODUCT_DEFINITION_SHAPE($,$,#304);
#61872=PRODUCT_DEFINITION_SHAPE($,$,#305);
#61873=PRODUCT_DEFINITION_SHAPE($,$,#306);
#61874=PRODUCT_DEFINITION_SHAPE($,$,#307);
#61875=PRODUCT_DEFINITION_SHAPE($,$,#308);
#61876=PRODUCT_DEFINITION_SHAPE($,$,#309);
#61877=PRODUCT_DEFINITION_SHAPE($,$,#310);
#61878=PRODUCT_DEFINITION_SHAPE($,$,#311);
#61879=PRODUCT_DEFINITION_SHAPE($,$,#312);
#61880=PRODUCT_DEFINITION_SHAPE($,$,#313);
#61881=PRODUCT_DEFINITION_SHAPE('',$,#62018);
#61882=PRODUCT_DEFINITION_SHAPE('',$,#62019);
#61883=PRODUCT_DEFINITION_SHAPE('',$,#62020);
#61884=PRODUCT_DEFINITION_SHAPE('',$,#62021);
#61885=PRODUCT_DEFINITION_SHAPE('',$,#62022);
#61886=PRODUCT_DEFINITION_SHAPE($,$,#314);
#61887=PRODUCT_DEFINITION_SHAPE($,$,#315);
#61888=PRODUCT_DEFINITION_SHAPE($,$,#316);
#61889=PRODUCT_DEFINITION_SHAPE($,$,#317);
#61890=PRODUCT_DEFINITION_SHAPE($,$,#318);
#61891=PRODUCT_DEFINITION_SHAPE($,$,#319);
#61892=PRODUCT_DEFINITION_SHAPE($,$,#320);
#61893=PRODUCT_DEFINITION_SHAPE($,$,#321);
#61894=PRODUCT_DEFINITION_SHAPE($,$,#322);
#61895=PRODUCT_DEFINITION_SHAPE($,$,#323);
#61896=PRODUCT_DEFINITION_SHAPE($,$,#324);
#61897=PRODUCT_DEFINITION_SHAPE($,$,#325);
#61898=PRODUCT_DEFINITION_SHAPE($,$,#326);
#61899=PRODUCT_DEFINITION_SHAPE($,$,#327);
#61900=PRODUCT_DEFINITION_SHAPE($,$,#328);
#61901=PRODUCT_DEFINITION_SHAPE($,$,#329);
#61902=PRODUCT_DEFINITION_SHAPE('',$,#62023);
#61903=PRODUCT_DEFINITION_SHAPE('',$,#62024);
#61904=PRODUCT_DEFINITION_SHAPE('',$,#62025);
#61905=PRODUCT_DEFINITION_SHAPE($,$,#330);
#61906=PRODUCT_DEFINITION_SHAPE($,$,#331);
#61907=PRODUCT_DEFINITION_SHAPE('',$,#62026);
#61908=PRODUCT_DEFINITION_SHAPE('',$,#62027);
#61909=PRODUCT_DEFINITION_SHAPE('',$,#62028);
#61910=PRODUCT_DEFINITION_SHAPE($,$,#332);
#61911=PRODUCT_DEFINITION_SHAPE($,$,#333);
#61912=PRODUCT_DEFINITION_SHAPE($,$,#334);
#61913=PRODUCT_DEFINITION_SHAPE($,$,#335);
#61914=PRODUCT_DEFINITION_SHAPE($,$,#336);
#61915=PRODUCT_DEFINITION_SHAPE($,$,#337);
#61916=PRODUCT_DEFINITION_SHAPE($,$,#338);
#61917=PRODUCT_DEFINITION_SHAPE($,$,#339);
#61918=PRODUCT_DEFINITION_SHAPE($,$,#340);
#61919=PRODUCT_DEFINITION_SHAPE($,$,#341);
#61920=PRODUCT_DEFINITION_SHAPE($,$,#342);
#61921=PRODUCT_DEFINITION_SHAPE($,$,#343);
#61922=PRODUCT_DEFINITION_SHAPE($,$,#344);
#61923=PRODUCT_DEFINITION_SHAPE($,$,#345);
#61924=PRODUCT_DEFINITION_SHAPE($,$,#346);
#61925=PRODUCT_DEFINITION_SHAPE($,$,#347);
#61926=PRODUCT_DEFINITION_SHAPE($,$,#348);
#61927=PRODUCT_DEFINITION_SHAPE($,$,#349);
#61928=PRODUCT_DEFINITION_SHAPE($,$,#350);
#61929=PRODUCT_DEFINITION_SHAPE($,$,#351);
#61930=PRODUCT_DEFINITION_SHAPE($,$,#352);
#61931=PRODUCT_DEFINITION_SHAPE($,$,#353);
#61932=PRODUCT_DEFINITION_SHAPE($,$,#354);
#61933=PRODUCT_DEFINITION_SHAPE($,$,#355);
#61934=PRODUCT_DEFINITION_SHAPE($,$,#356);
#61935=PRODUCT_DEFINITION_SHAPE($,$,#357);
#61936=PRODUCT_DEFINITION_SHAPE($,$,#358);
#61937=PRODUCT_DEFINITION_SHAPE($,$,#359);
#61938=PRODUCT_DEFINITION_SHAPE($,$,#360);
#61939=PRODUCT_DEFINITION_SHAPE($,$,#361);
#61940=PRODUCT_DEFINITION_SHAPE($,$,#362);
#61941=PRODUCT_DEFINITION_SHAPE($,$,#363);
#61942=PRODUCT_DEFINITION_SHAPE($,$,#364);
#61943=PRODUCT_DEFINITION_SHAPE($,$,#365);
#61944=PRODUCT_DEFINITION_SHAPE($,$,#366);
#61945=PRODUCT_DEFINITION_SHAPE($,$,#367);
#61946=PRODUCT_DEFINITION_SHAPE($,$,#368);
#61947=PRODUCT_DEFINITION_SHAPE($,$,#369);
#61948=PRODUCT_DEFINITION_SHAPE($,$,#370);
#61949=PRODUCT_DEFINITION_SHAPE($,$,#371);
#61950=PRODUCT_DEFINITION_SHAPE($,$,#372);
#61951=PRODUCT_DEFINITION_SHAPE($,$,#373);
#61952=PRODUCT_DEFINITION_SHAPE($,$,#374);
#61953=PRODUCT_DEFINITION_SHAPE($,$,#375);
#61954=PRODUCT_DEFINITION_SHAPE($,$,#376);
#61955=PRODUCT_DEFINITION_SHAPE($,$,#377);
#61956=PRODUCT_DEFINITION_SHAPE($,$,#378);
#61957=PRODUCT_DEFINITION_SHAPE($,$,#379);
#61958=PRODUCT_DEFINITION_SHAPE($,$,#380);
#61959=PRODUCT_DEFINITION_SHAPE($,$,#381);
#61960=PRODUCT_DEFINITION_SHAPE($,$,#382);
#61961=PRODUCT_DEFINITION_SHAPE($,$,#383);
#61962=PRODUCT_DEFINITION_SHAPE($,$,#384);
#61963=PRODUCT_DEFINITION_SHAPE($,$,#385);
#61964=PRODUCT_DEFINITION_SHAPE($,$,#386);
#61965=PRODUCT_DEFINITION_SHAPE($,$,#387);
#61966=PRODUCT_DEFINITION_SHAPE($,$,#388);
#61967=PRODUCT_DEFINITION_SHAPE($,$,#389);
#61968=SHAPE_REPRESENTATION('',(#34116,#38118,#38119,#38120,#38121,#38122,
#38123,#38124,#38125,#38126,#38127,#38128,#38129,#38130,#38131,#38132,#38133,
#38134,#38135,#38136,#38137,#38138,#38139,#38140,#38141,#38142,#38143,#38144,
#38145,#38146,#38147,#38148,#38149,#38150,#38151,#38152,#38153,#38154,#38155,
#38156,#38157,#38158,#38159,#38160,#38161,#38162,#38163,#38164,#38165,#38166,
#38167,#38168,#38169,#38170,#38171,#38172,#38173),#61781);
#61969=SHAPE_REPRESENTATION('',(#34117),#61782);
#61970=SHAPE_REPRESENTATION('',(#34153),#61783);
#61971=SHAPE_REPRESENTATION('',(#34392),#61784);
#61972=SHAPE_REPRESENTATION('',(#34420),#61785);
#61973=SHAPE_REPRESENTATION('',(#34448),#61786);
#61974=SHAPE_REPRESENTATION('',(#34476),#61787);
#61975=SHAPE_REPRESENTATION('',(#34512),#61788);
#61976=SHAPE_REPRESENTATION('',(#34528),#61789);
#61977=SHAPE_REPRESENTATION('',(#34568),#61790);
#61978=SHAPE_REPRESENTATION('',(#35040),#61791);
#61979=SHAPE_REPRESENTATION('',(#35191),#61792);
#61980=SHAPE_REPRESENTATION('',(#35702,#35945,#35946,#35947,#35948,#35949,
#35950,#35951,#35952,#35953,#35954,#35955,#35956,#35957,#35958,#35959,#35960),
#61793);
#61981=SHAPE_REPRESENTATION('',(#35703),#61794);
#61982=SHAPE_REPRESENTATION('',(#35762),#61795);
#61983=SHAPE_REPRESENTATION('',(#35823),#61796);
#61984=SHAPE_REPRESENTATION('',(#35884),#61797);
#61985=SHAPE_REPRESENTATION('',(#35909),#61798);
#61986=SHAPE_REPRESENTATION('',(#35922),#61799);
#61987=SHAPE_REPRESENTATION('',(#35961,#36131,#36132,#36133,#36134,#36135,
#36136,#36137,#36138,#36139,#36140,#36141,#36142,#36143,#36144,#36145,#36146),
#61800);
#61988=SHAPE_REPRESENTATION('',(#35962),#61801);
#61989=SHAPE_REPRESENTATION('',(#36032),#61802);
#61990=SHAPE_REPRESENTATION('',(#36110),#61803);
#61991=SHAPE_REPRESENTATION('',(#36122),#61804);
#61992=SHAPE_REPRESENTATION('',(#36147,#37244,#37245),#61805);
#61993=SHAPE_REPRESENTATION('',(#36148),#61806);
#61994=SHAPE_REPRESENTATION('',(#36744),#61807);
#61995=SHAPE_REPRESENTATION('',(#37246,#38116,#38117),#61808);
#61996=SHAPE_REPRESENTATION('',(#37247),#61809);
#61997=SHAPE_REPRESENTATION('',(#38087),#61810);
#61998=PRODUCT_DEFINITION_CONTEXT('part definition',#62090,'design');
#61999=PRODUCT_DEFINITION('Assembly47','MAT-059',#62029,#61998);
#62000=PRODUCT_DEFINITION('Shredder Cutting Blades',
'Shredder Cutting Blades',#62030,#61998);
#62001=PRODUCT_DEFINITION('Shaft Bearing Flange Units',
'Shaft Bearing Flange Units',#62031,#61998);
#62002=PRODUCT_DEFINITION('Bearing Housing Socket Screws',
'Bearing Housing Socket Screws',#62032,#61998);
#62003=PRODUCT_DEFINITION('Chamber Front Plate Socket Screws',
'Chamber Front Plate Socket Screws',#62033,#61998);
#62004=PRODUCT_DEFINITION('Extended Housing Socket Screw',
'Extended Housing Socket Screw',#62034,#61998);
#62005=PRODUCT_DEFINITION('Chamber Hex Head Bolts',
'Chamber Hex Head Bolts',#62035,#61998);
#62006=PRODUCT_DEFINITION('Infeed Hopper Chute','Infeed Hopper Chute',#62036,
#61998);
#62007=PRODUCT_DEFINITION('Discharge Chute Funnel',
'Discharge Chute Funnel',#62037,#61998);
#62008=PRODUCT_DEFINITION('Electric Drive Motor','Electric Drive Motor',
#62038,#61998);
#62009=PRODUCT_DEFINITION('Motor and Gearbox Mounting Plate',
'Motor and Gearbox Mounting Plate',#62039,#61998);
#62010=PRODUCT_DEFINITION('Machine Frame Stand','Machine Frame Stand',#62040,
#61998);
#62011=PRODUCT_DEFINITION('Shredder Cutting Chamber Housing',
'Shredder Cutting Chamber Housing',#62041,#61998);
#62012=PRODUCT_DEFINITION('Chamber Housing','Chamber Housing',#62042,#61998);
#62013=PRODUCT_DEFINITION('Left Side Plate','Left Side Plate',#62043,#61998);
#62014=PRODUCT_DEFINITION('Right Side Plate','Right Side Plate',#62044,
#61998);
#62015=PRODUCT_DEFINITION('Front Plate','Front Plate',#62045,#61998);
#62016=PRODUCT_DEFINITION('Stripper Fin','Stripper Fin',#62046,#61998);
#62017=PRODUCT_DEFINITION('Chamber Base Plate','Chamber Base Plate',#62047,
#61998);
#62018=PRODUCT_DEFINITION('Dual Cutter Shafts','Dual Cutter Shafts',#62048,
#61998);
#62019=PRODUCT_DEFINITION('Cutter Shaft A','Cutter Shaft A',#62049,#61998);
#62020=PRODUCT_DEFINITION('Cutter Shaft B','Cutter Shaft B',#62050,#61998);
#62021=PRODUCT_DEFINITION('Shaft Spacer','Shaft Spacer',#62051,#61998);
#62022=PRODUCT_DEFINITION('Shaft Washer','Shaft Washer',#62052,#61998);
#62023=PRODUCT_DEFINITION('Drive Reduction Gears',
'Drive Reduction Gears',#62053,#61998);
#62024=PRODUCT_DEFINITION('Large Spur Gear','Large Spur Gear',#62054,#61998);
#62025=PRODUCT_DEFINITION('Small Spur Gear','Small Spur Gear',#62055,#61998);
#62026=PRODUCT_DEFINITION('Gearbox Reducer Unit','Gearbox Reducer Unit',
#62056,#61998);
#62027=PRODUCT_DEFINITION('Gearbox Reducer','Gearbox Reducer',#62057,#61998);
#62028=PRODUCT_DEFINITION('Shaft Coupling','Shaft Coupling',#62058,#61998);
#62029=PRODUCT_DEFINITION_FORMATION('',$,#62092);
#62030=PRODUCT_DEFINITION_FORMATION('',$,#62093);
#62031=PRODUCT_DEFINITION_FORMATION('',$,#62094);
#62032=PRODUCT_DEFINITION_FORMATION('',$,#62095);
#62033=PRODUCT_DEFINITION_FORMATION('',$,#62096);
#62034=PRODUCT_DEFINITION_FORMATION('',$,#62097);
#62035=PRODUCT_DEFINITION_FORMATION('',$,#62098);
#62036=PRODUCT_DEFINITION_FORMATION('',$,#62099);
#62037=PRODUCT_DEFINITION_FORMATION('',$,#62100);
#62038=PRODUCT_DEFINITION_FORMATION('',$,#62101);
#62039=PRODUCT_DEFINITION_FORMATION('',$,#62102);
#62040=PRODUCT_DEFINITION_FORMATION('',$,#62103);
#62041=PRODUCT_DEFINITION_FORMATION('',$,#62104);
#62042=PRODUCT_DEFINITION_FORMATION('',$,#62105);
#62043=PRODUCT_DEFINITION_FORMATION('',$,#62106);
#62044=PRODUCT_DEFINITION_FORMATION('',$,#62107);
#62045=PRODUCT_DEFINITION_FORMATION('',$,#62108);
#62046=PRODUCT_DEFINITION_FORMATION('',$,#62109);
#62047=PRODUCT_DEFINITION_FORMATION('',$,#62110);
#62048=PRODUCT_DEFINITION_FORMATION('',$,#62111);
#62049=PRODUCT_DEFINITION_FORMATION('',$,#62112);
#62050=PRODUCT_DEFINITION_FORMATION('',$,#62113);
#62051=PRODUCT_DEFINITION_FORMATION('',$,#62114);
#62052=PRODUCT_DEFINITION_FORMATION('',$,#62115);
#62053=PRODUCT_DEFINITION_FORMATION('',$,#62116);
#62054=PRODUCT_DEFINITION_FORMATION('',$,#62117);
#62055=PRODUCT_DEFINITION_FORMATION('',$,#62118);
#62056=PRODUCT_DEFINITION_FORMATION('',$,#62119);
#62057=PRODUCT_DEFINITION_FORMATION('',$,#62120);
#62058=PRODUCT_DEFINITION_FORMATION('',$,#62121);
#62059=PRODUCT_RELATED_PRODUCT_CATEGORY('MAT-059',
'MAT-059',(#62092));
#62060=PRODUCT_RELATED_PRODUCT_CATEGORY('Shredder Cutting Blades',
'Shredder Cutting Blades',(#62093));
#62061=PRODUCT_RELATED_PRODUCT_CATEGORY('Shaft Bearing Flange Units',
'Shaft Bearing Flange Units',(#62094));
#62062=PRODUCT_RELATED_PRODUCT_CATEGORY('Bearing Housing Socket Screws',
'Bearing Housing Socket Screws',(#62095));
#62063=PRODUCT_RELATED_PRODUCT_CATEGORY(
'Chamber Front Plate Socket Screws','Chamber Front Plate Socket Screws',
(#62096));
#62064=PRODUCT_RELATED_PRODUCT_CATEGORY('Extended Housing Socket Screw',
'Extended Housing Socket Screw',(#62097));
#62065=PRODUCT_RELATED_PRODUCT_CATEGORY('Chamber Hex Head Bolts',
'Chamber Hex Head Bolts',(#62098));
#62066=PRODUCT_RELATED_PRODUCT_CATEGORY('Infeed Hopper Chute',
'Infeed Hopper Chute',(#62099));
#62067=PRODUCT_RELATED_PRODUCT_CATEGORY('Discharge Chute Funnel',
'Discharge Chute Funnel',(#62100));
#62068=PRODUCT_RELATED_PRODUCT_CATEGORY('Electric Drive Motor',
'Electric Drive Motor',(#62101));
#62069=PRODUCT_RELATED_PRODUCT_CATEGORY(
'Motor and Gearbox Mounting Plate','Motor and Gearbox Mounting Plate',(#62102));
#62070=PRODUCT_RELATED_PRODUCT_CATEGORY('Machine Frame Stand',
'Machine Frame Stand',(#62103));
#62071=PRODUCT_RELATED_PRODUCT_CATEGORY(
'Shredder Cutting Chamber Housing','Shredder Cutting Chamber Housing',(#62104));
#62072=PRODUCT_RELATED_PRODUCT_CATEGORY('Chamber Housing',
'Chamber Housing',(#62105));
#62073=PRODUCT_RELATED_PRODUCT_CATEGORY('Left Side Plate',
'Left Side Plate',(#62106));
#62074=PRODUCT_RELATED_PRODUCT_CATEGORY('Right Side Plate',
'Right Side Plate',(#62107));
#62075=PRODUCT_RELATED_PRODUCT_CATEGORY('Front Plate','Front Plate',(#62108));
#62076=PRODUCT_RELATED_PRODUCT_CATEGORY('Stripper Fin','Stripper Fin',(#62109));
#62077=PRODUCT_RELATED_PRODUCT_CATEGORY('Chamber Base Plate',
'Chamber Base Plate',(#62110));
#62078=PRODUCT_RELATED_PRODUCT_CATEGORY('Dual Cutter Shafts',
'Dual Cutter Shafts',(#62111));
#62079=PRODUCT_RELATED_PRODUCT_CATEGORY('Cutter Shaft A',
'Cutter Shaft A',(#62112));
#62080=PRODUCT_RELATED_PRODUCT_CATEGORY('Cutter Shaft B',
'Cutter Shaft B',(#62113));
#62081=PRODUCT_RELATED_PRODUCT_CATEGORY('Shaft Spacer','Shaft Spacer',(#62114));
#62082=PRODUCT_RELATED_PRODUCT_CATEGORY('Shaft Washer','Shaft Washer',(#62115));
#62083=PRODUCT_RELATED_PRODUCT_CATEGORY('Drive Reduction Gears',
'Drive Reduction Gears',(#62116));
#62084=PRODUCT_RELATED_PRODUCT_CATEGORY('Large Spur Gear',
'Large Spur Gear',(#62117));
#62085=PRODUCT_RELATED_PRODUCT_CATEGORY('Small Spur Gear',
'Small Spur Gear',(#62118));
#62086=PRODUCT_RELATED_PRODUCT_CATEGORY('Gearbox Reducer Unit',
'Gearbox Reducer Unit',(#62119));
#62087=PRODUCT_RELATED_PRODUCT_CATEGORY('Gearbox Reducer',
'Gearbox Reducer',(#62120));
#62088=PRODUCT_RELATED_PRODUCT_CATEGORY('Shaft Coupling',
'Shaft Coupling',(#62121));
#62089=APPLICATION_PROTOCOL_DEFINITION('international standard',
'ap242_managed_model_based_3d_engineering',2011,#62090);
#62090=APPLICATION_CONTEXT('Managed model based 3d engineering');
#62091=PRODUCT_CONTEXT('part definition',#62090,'mechanical');
#62092=PRODUCT('Assembly47','MAT-059',$,(#62091));
#62093=PRODUCT('Shredder Cutting Blades','Shredder Cutting Blades',$,(#62091));
#62094=PRODUCT('Shaft Bearing Flange Units',
'Shaft Bearing Flange Units',$,(#62091));
#62095=PRODUCT('Bearing Housing Socket Screws',
'Bearing Housing Socket Screws',$,(#62091));
#62096=PRODUCT('Chamber Front Plate Socket Screws',
'Chamber Front Plate Socket Screws',$,(#62091));
#62097=PRODUCT('Extended Housing Socket Screw',
'Extended Housing Socket Screw',$,(#62091));
#62098=PRODUCT('Chamber Hex Head Bolts','Chamber Hex Head Bolts',$,(#62091));
#62099=PRODUCT('Infeed Hopper Chute','Infeed Hopper Chute',$,(#62091));
#62100=PRODUCT('Discharge Chute Funnel','Discharge Chute Funnel',$,(#62091));
#62101=PRODUCT('Electric Drive Motor','Electric Drive Motor',$,(#62091));
#62102=PRODUCT('Motor and Gearbox Mounting Plate',
'Motor and Gearbox Mounting Plate',$,(#62091));
#62103=PRODUCT('Machine Frame Stand','Machine Frame Stand',$,(#62091));
#62104=PRODUCT('Shredder Cutting Chamber Housing',
'Shredder Cutting Chamber Housing',$,(#62091));
#62105=PRODUCT('Chamber Housing','Chamber Housing',$,(#62091));
#62106=PRODUCT('Left Side Plate','Left Side Plate',$,(#62091));
#62107=PRODUCT('Right Side Plate','Right Side Plate',$,(#62091));
#62108=PRODUCT('Front Plate','Front Plate',$,(#62091));
#62109=PRODUCT('Stripper Fin','Stripper Fin',$,(#62091));
#62110=PRODUCT('Chamber Base Plate','Chamber Base Plate',$,(#62091));
#62111=PRODUCT('Dual Cutter Shafts','Dual Cutter Shafts',$,(#62091));
#62112=PRODUCT('Cutter Shaft A','Cutter Shaft A',$,(#62091));
#62113=PRODUCT('Cutter Shaft B','Cutter Shaft B',$,(#62091));
#62114=PRODUCT('Shaft Spacer','Shaft Spacer',$,(#62091));
#62115=PRODUCT('Shaft Washer','Shaft Washer',$,(#62091));
#62116=PRODUCT('Drive Reduction Gears','Drive Reduction Gears',$,(#62091));
#62117=PRODUCT('Large Spur Gear','Large Spur Gear',$,(#62091));
#62118=PRODUCT('Small Spur Gear','Small Spur Gear',$,(#62091));
#62119=PRODUCT('Gearbox Reducer Unit','Gearbox Reducer Unit',$,(#62091));
#62120=PRODUCT('Gearbox Reducer','Gearbox Reducer',$,(#62091));
#62121=PRODUCT('Shaft Coupling','Shaft Coupling',$,(#62091));
#62122=PRESENTATION_STYLE_ASSIGNMENT((#62123));
#62123=SURFACE_STYLE_USAGE(.BOTH.,#62124);
#62124=SURFACE_SIDE_STYLE('',(#62125));
#62125=SURFACE_STYLE_FILL_AREA(#62126);
#62126=FILL_AREA_STYLE('Steel - Satin',(#62127));
#62127=FILL_AREA_STYLE_COLOUR('Steel - Satin',#62128);
#62128=COLOUR_RGB('Steel - Satin',0.627450980392157,0.627450980392157,0.627450980392157);
#62129=COLOUR_RGB('Dark Blue',0.08,0.2,0.34);
#62130=FILL_AREA_STYLE_COLOUR('',#62129);
#62131=FILL_AREA_STYLE('',(#62130));
#62132=SURFACE_STYLE_FILL_AREA(#62131);
#62133=SURFACE_SIDE_STYLE('',(#62132));
#62134=SURFACE_STYLE_USAGE(.BOTH.,#62133);
#62135=PRESENTATION_STYLE_ASSIGNMENT((#62134));
#62136=COLOUR_RGB('Light Blue',0.38,0.62,0.78);
#62137=FILL_AREA_STYLE_COLOUR('',#62136);
#62138=FILL_AREA_STYLE('',(#62137));
#62139=SURFACE_STYLE_FILL_AREA(#62138);
#62140=SURFACE_SIDE_STYLE('',(#62139));
#62141=SURFACE_STYLE_USAGE(.BOTH.,#62140);
#62142=PRESENTATION_STYLE_ASSIGNMENT((#62141));
#62143=COLOUR_RGB('Sky Blue',0.24,0.69,0.87);
#62144=FILL_AREA_STYLE_COLOUR('',#62143);
#62145=FILL_AREA_STYLE('',(#62144));
#62146=SURFACE_STYLE_FILL_AREA(#62145);
#62147=SURFACE_SIDE_STYLE('',(#62146));
#62148=SURFACE_STYLE_USAGE(.BOTH.,#62147);
#62149=PRESENTATION_STYLE_ASSIGNMENT((#62148));
#62150=COLOUR_RGB('Grey',0.48,0.52,0.57);
#62151=FILL_AREA_STYLE_COLOUR('',#62150);
#62152=FILL_AREA_STYLE('',(#62151));
#62153=SURFACE_STYLE_FILL_AREA(#62152);
#62154=SURFACE_SIDE_STYLE('',(#62153));
#62155=SURFACE_STYLE_USAGE(.BOTH.,#62154);
#62156=PRESENTATION_STYLE_ASSIGNMENT((#62155));
#62157=COLOUR_RGB('Black',0.12,0.14,0.17);
#62158=FILL_AREA_STYLE_COLOUR('',#62157);
#62159=FILL_AREA_STYLE('',(#62158));
#62160=SURFACE_STYLE_FILL_AREA(#62159);
#62161=SURFACE_SIDE_STYLE('',(#62160));
#62162=SURFACE_STYLE_USAGE(.BOTH.,#62161);
#62163=PRESENTATION_STYLE_ASSIGNMENT((#62162));
#62164=COLOUR_RGB('Off White',0.89,0.88,0.83);
#62165=FILL_AREA_STYLE_COLOUR('',#62164);
#62166=FILL_AREA_STYLE('',(#62165));
#62167=SURFACE_STYLE_FILL_AREA(#62166);
#62168=SURFACE_SIDE_STYLE('',(#62167));
#62169=SURFACE_STYLE_USAGE(.BOTH.,#62168);
#62170=PRESENTATION_STYLE_ASSIGNMENT((#62169));
ENDSEC;
END-ISO-10303-21;
